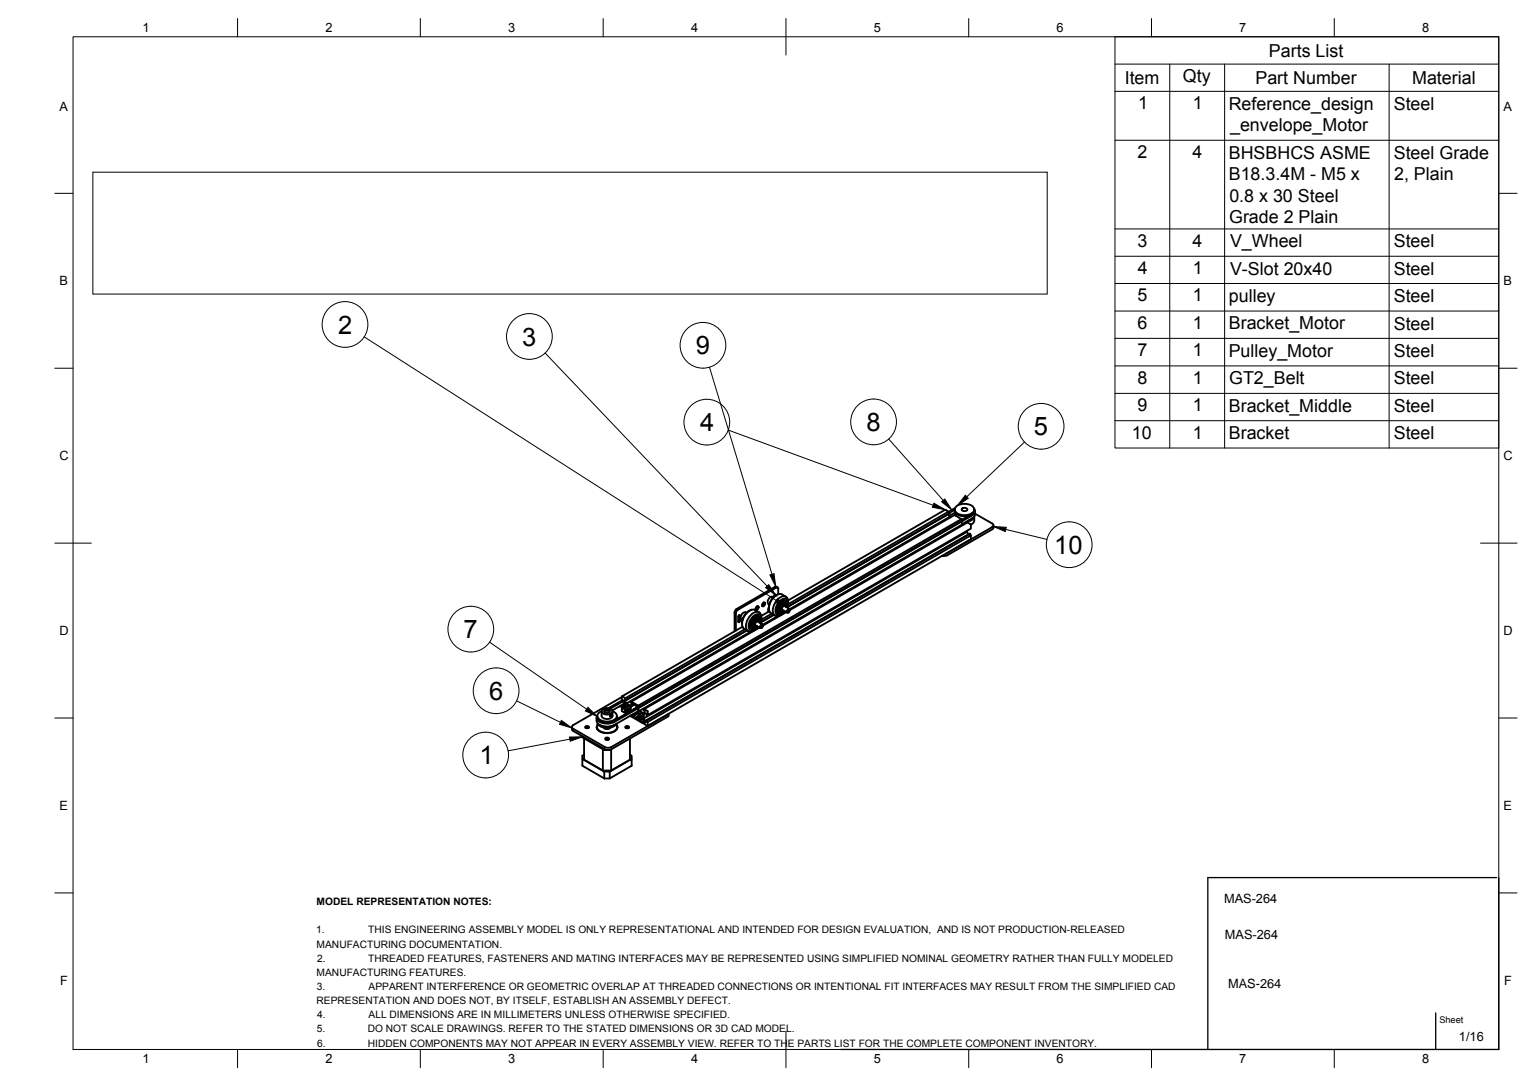
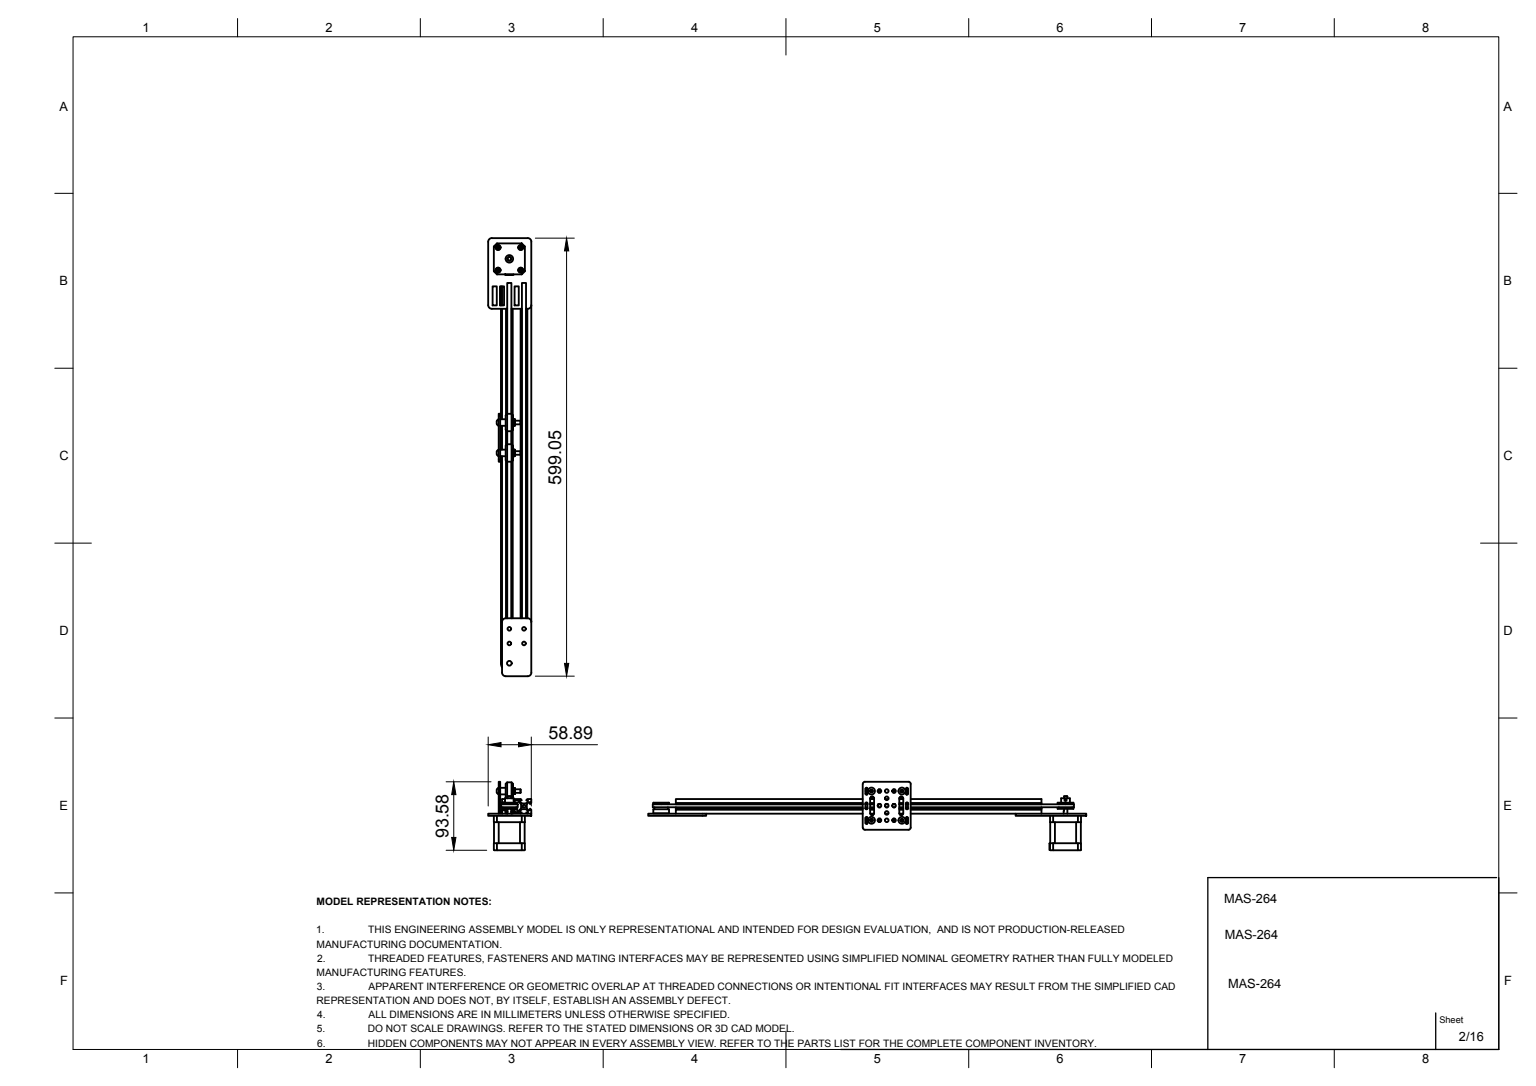
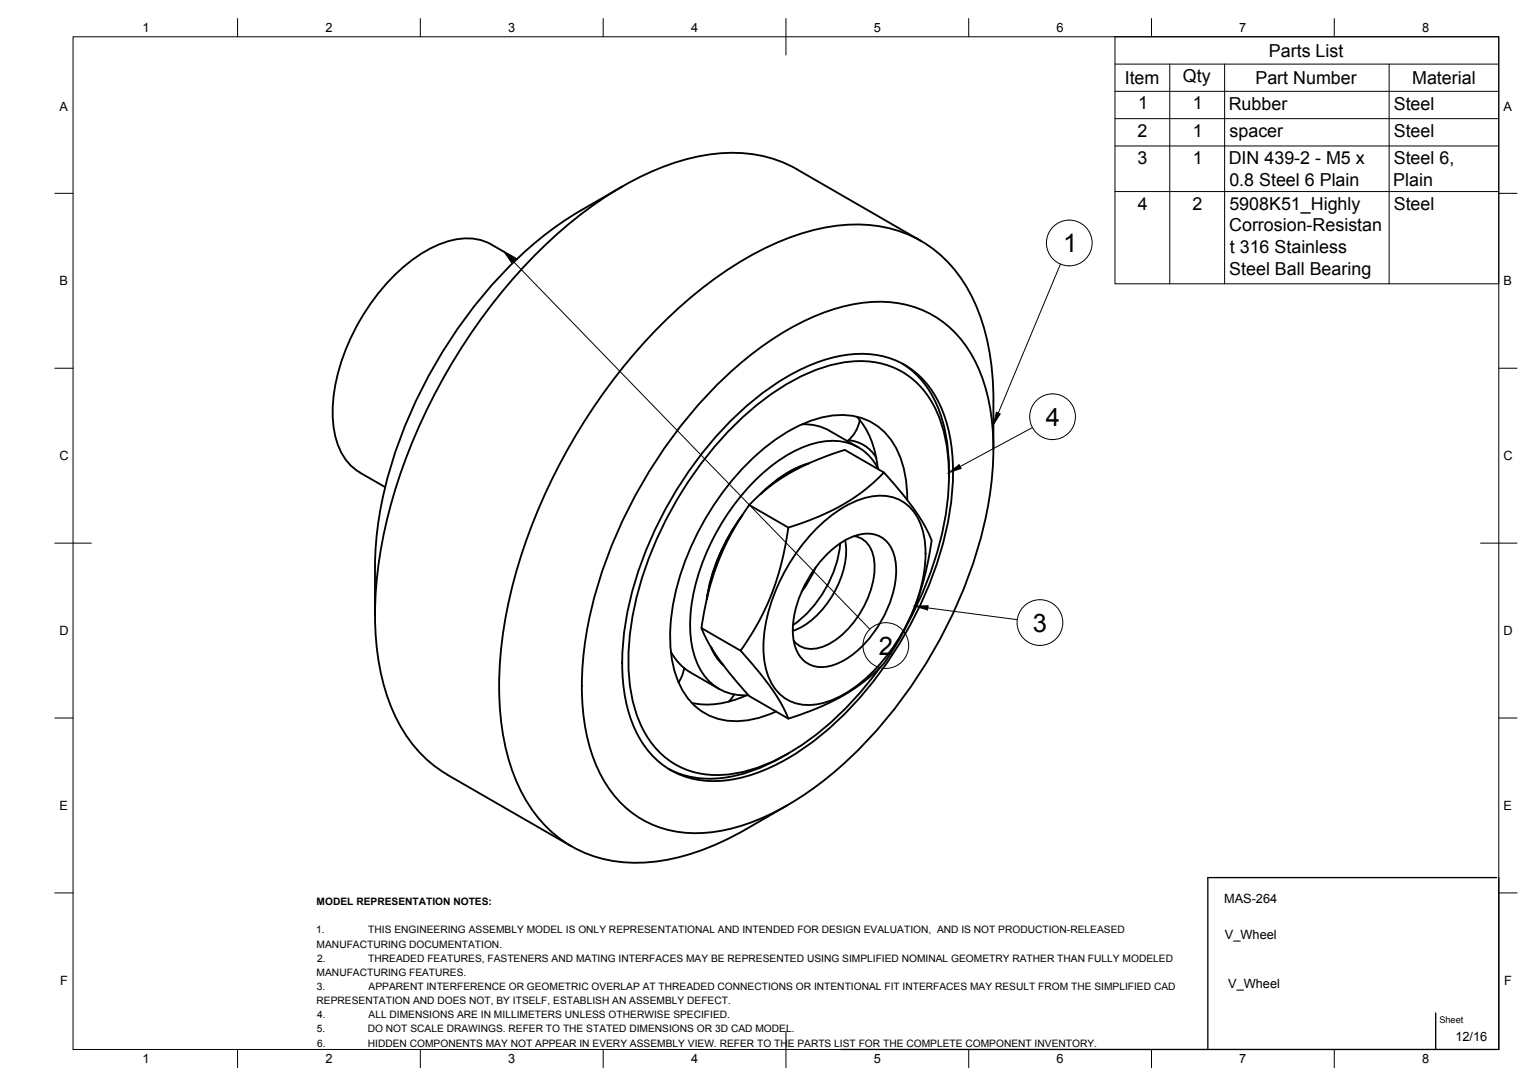
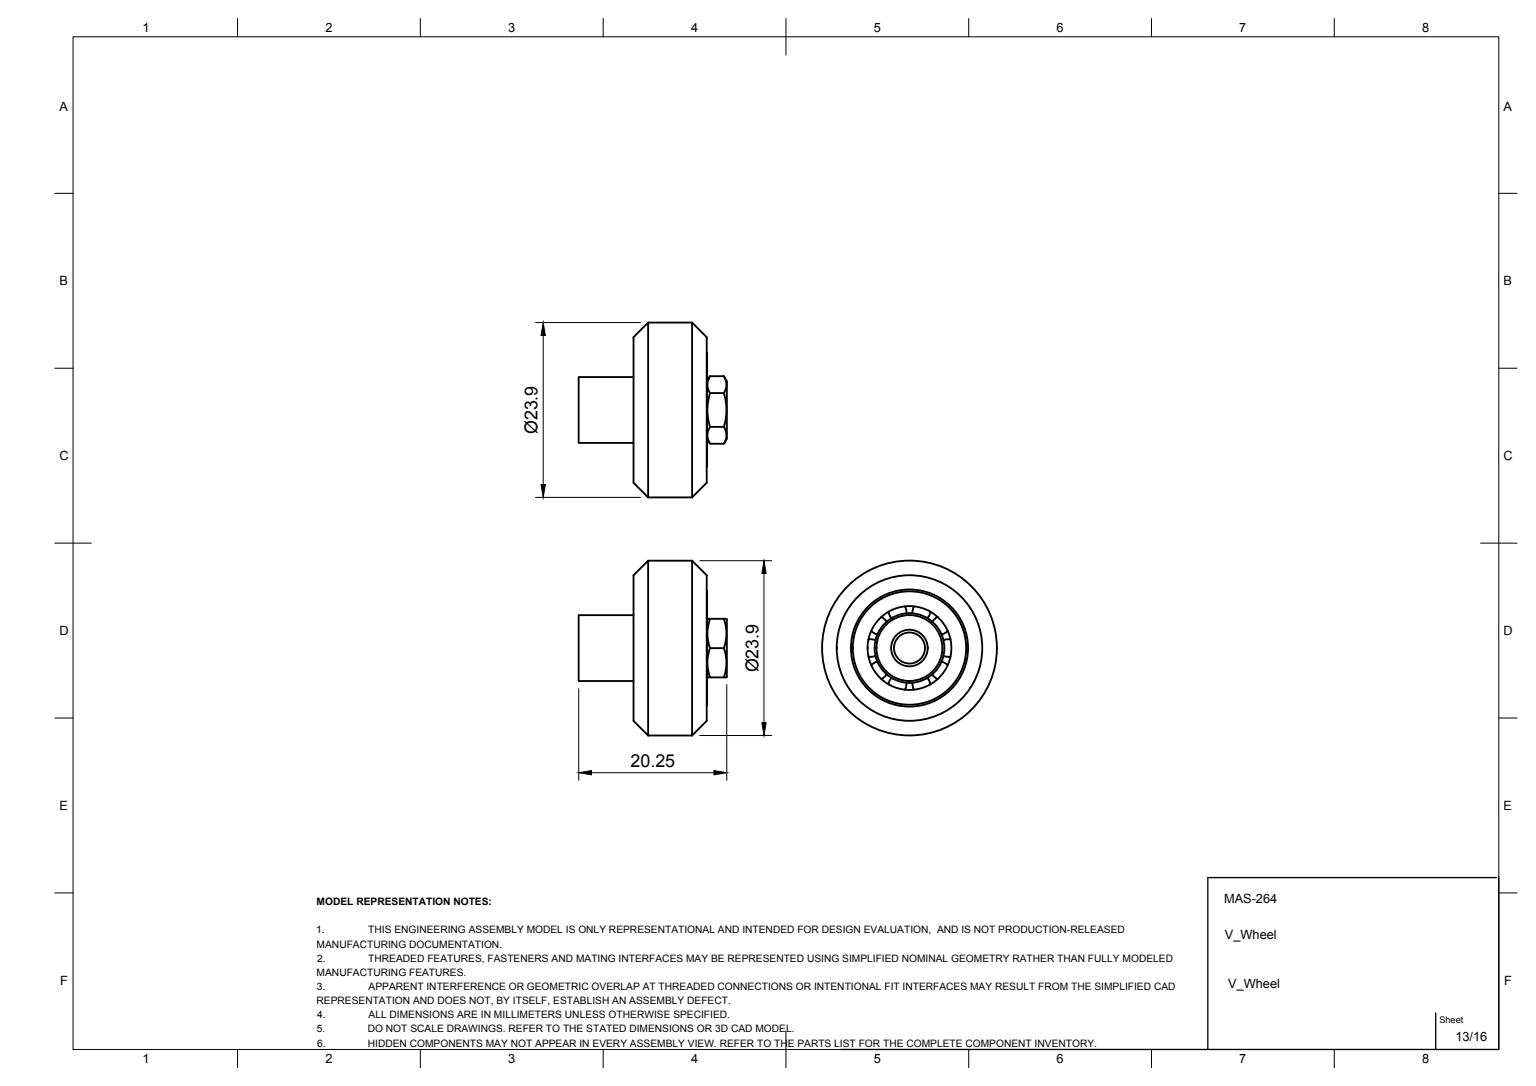
ISO-10303-21;
HEADER;
/* Generated by software containing ST-Developer
 * from STEP Tools, Inc. (www.steptools.com) 
 */

FILE_DESCRIPTION(
/* description */ (''),
/* implementation_level */ '2;1');

FILE_NAME(
/* name */ 'MAS-264',
/* time_stamp */ '2026-10-12T15:37:13-07:00',
/* author */ (''),
/* organization */ (''),
/* preprocessor_version */ 'ST-DEVELOPER v20.2',
/* originating_system */ 'Autodesk Translation Framework v15.15.0.0',
/* authorisation */ '');

FILE_SCHEMA (('AUTOMOTIVE_DESIGN { 1 0 10303 214 3 1 1 }'));
ENDSEC;

DATA;
#10=MECHANICAL_DESIGN_GEOMETRIC_PRESENTATION_REPRESENTATION('',(#326,#327,
#328,#329,#330,#331,#332,#333,#334,#335,#336,#337,#338,#339,#340,#341,#342,
#343,#344,#345,#346,#347,#348,#349,#350,#351,#352,#353,#354,#355,#356,#357),
#36460);
#11=ITEM_DEFINED_TRANSFORMATION($,$,#11888,#12004);
#12=ITEM_DEFINED_TRANSFORMATION($,$,#11901,#12005);
#13=ITEM_DEFINED_TRANSFORMATION($,$,#11910,#12006);
#14=ITEM_DEFINED_TRANSFORMATION($,$,#11930,#12007);
#15=ITEM_DEFINED_TRANSFORMATION($,$,#11930,#12008);
#16=ITEM_DEFINED_TRANSFORMATION($,$,#11439,#12421);
#17=ITEM_DEFINED_TRANSFORMATION($,$,#12393,#12422);
#18=ITEM_DEFINED_TRANSFORMATION($,$,#11887,#12423);
#19=ITEM_DEFINED_TRANSFORMATION($,$,#11887,#12424);
#20=ITEM_DEFINED_TRANSFORMATION($,$,#11887,#12425);
#21=ITEM_DEFINED_TRANSFORMATION($,$,#11887,#12426);
#22=ITEM_DEFINED_TRANSFORMATION($,$,#12009,#12427);
#23=ITEM_DEFINED_TRANSFORMATION($,$,#12118,#12428);
#24=ITEM_DEFINED_TRANSFORMATION($,$,#12135,#12429);
#25=ITEM_DEFINED_TRANSFORMATION($,$,#12189,#12430);
#26=ITEM_DEFINED_TRANSFORMATION($,$,#12212,#12431);
#27=ITEM_DEFINED_TRANSFORMATION($,$,#12231,#12432);
#28=ITEM_DEFINED_TRANSFORMATION($,$,#12359,#12433);
#29=ITEM_DEFINED_TRANSFORMATION($,$,#12393,#12434);
#30=ITEM_DEFINED_TRANSFORMATION($,$,#12393,#12435);
#31=ITEM_DEFINED_TRANSFORMATION($,$,#12393,#12436);
#32=(
REPRESENTATION_RELATIONSHIP($,$,#36519,#36518)
REPRESENTATION_RELATIONSHIP_WITH_TRANSFORMATION(#11)
SHAPE_REPRESENTATION_RELATIONSHIP()
);
#33=(
REPRESENTATION_RELATIONSHIP($,$,#36520,#36518)
REPRESENTATION_RELATIONSHIP_WITH_TRANSFORMATION(#12)
SHAPE_REPRESENTATION_RELATIONSHIP()
);
#34=(
REPRESENTATION_RELATIONSHIP($,$,#36521,#36518)
REPRESENTATION_RELATIONSHIP_WITH_TRANSFORMATION(#13)
SHAPE_REPRESENTATION_RELATIONSHIP()
);
#35=(
REPRESENTATION_RELATIONSHIP($,$,#36522,#36518)
REPRESENTATION_RELATIONSHIP_WITH_TRANSFORMATION(#14)
SHAPE_REPRESENTATION_RELATIONSHIP()
);
#36=(
REPRESENTATION_RELATIONSHIP($,$,#36522,#36518)
REPRESENTATION_RELATIONSHIP_WITH_TRANSFORMATION(#15)
SHAPE_REPRESENTATION_RELATIONSHIP()
);
#37=(
REPRESENTATION_RELATIONSHIP($,$,#36517,#36516)
REPRESENTATION_RELATIONSHIP_WITH_TRANSFORMATION(#16)
SHAPE_REPRESENTATION_RELATIONSHIP()
);
#38=(
REPRESENTATION_RELATIONSHIP($,$,#36530,#36516)
REPRESENTATION_RELATIONSHIP_WITH_TRANSFORMATION(#17)
SHAPE_REPRESENTATION_RELATIONSHIP()
);
#39=(
REPRESENTATION_RELATIONSHIP($,$,#36518,#36516)
REPRESENTATION_RELATIONSHIP_WITH_TRANSFORMATION(#18)
SHAPE_REPRESENTATION_RELATIONSHIP()
);
#40=(
REPRESENTATION_RELATIONSHIP($,$,#36518,#36516)
REPRESENTATION_RELATIONSHIP_WITH_TRANSFORMATION(#19)
SHAPE_REPRESENTATION_RELATIONSHIP()
);
#41=(
REPRESENTATION_RELATIONSHIP($,$,#36518,#36516)
REPRESENTATION_RELATIONSHIP_WITH_TRANSFORMATION(#20)
SHAPE_REPRESENTATION_RELATIONSHIP()
);
#42=(
REPRESENTATION_RELATIONSHIP($,$,#36518,#36516)
REPRESENTATION_RELATIONSHIP_WITH_TRANSFORMATION(#21)
SHAPE_REPRESENTATION_RELATIONSHIP()
);
#43=(
REPRESENTATION_RELATIONSHIP($,$,#36523,#36516)
REPRESENTATION_RELATIONSHIP_WITH_TRANSFORMATION(#22)
SHAPE_REPRESENTATION_RELATIONSHIP()
);
#44=(
REPRESENTATION_RELATIONSHIP($,$,#36524,#36516)
REPRESENTATION_RELATIONSHIP_WITH_TRANSFORMATION(#23)
SHAPE_REPRESENTATION_RELATIONSHIP()
);
#45=(
REPRESENTATION_RELATIONSHIP($,$,#36525,#36516)
REPRESENTATION_RELATIONSHIP_WITH_TRANSFORMATION(#24)
SHAPE_REPRESENTATION_RELATIONSHIP()
);
#46=(
REPRESENTATION_RELATIONSHIP($,$,#36526,#36516)
REPRESENTATION_RELATIONSHIP_WITH_TRANSFORMATION(#25)
SHAPE_REPRESENTATION_RELATIONSHIP()
);
#47=(
REPRESENTATION_RELATIONSHIP($,$,#36527,#36516)
REPRESENTATION_RELATIONSHIP_WITH_TRANSFORMATION(#26)
SHAPE_REPRESENTATION_RELATIONSHIP()
);
#48=(
REPRESENTATION_RELATIONSHIP($,$,#36528,#36516)
REPRESENTATION_RELATIONSHIP_WITH_TRANSFORMATION(#27)
SHAPE_REPRESENTATION_RELATIONSHIP()
);
#49=(
REPRESENTATION_RELATIONSHIP($,$,#36529,#36516)
REPRESENTATION_RELATIONSHIP_WITH_TRANSFORMATION(#28)
SHAPE_REPRESENTATION_RELATIONSHIP()
);
#50=(
REPRESENTATION_RELATIONSHIP($,$,#36530,#36516)
REPRESENTATION_RELATIONSHIP_WITH_TRANSFORMATION(#29)
SHAPE_REPRESENTATION_RELATIONSHIP()
);
#51=(
REPRESENTATION_RELATIONSHIP($,$,#36530,#36516)
REPRESENTATION_RELATIONSHIP_WITH_TRANSFORMATION(#30)
SHAPE_REPRESENTATION_RELATIONSHIP()
);
#52=(
REPRESENTATION_RELATIONSHIP($,$,#36530,#36516)
REPRESENTATION_RELATIONSHIP_WITH_TRANSFORMATION(#31)
SHAPE_REPRESENTATION_RELATIONSHIP()
);
#53=CONTEXT_DEPENDENT_SHAPE_REPRESENTATION(#32,#36487);
#54=CONTEXT_DEPENDENT_SHAPE_REPRESENTATION(#33,#36488);
#55=CONTEXT_DEPENDENT_SHAPE_REPRESENTATION(#34,#36489);
#56=CONTEXT_DEPENDENT_SHAPE_REPRESENTATION(#35,#36490);
#57=CONTEXT_DEPENDENT_SHAPE_REPRESENTATION(#36,#36491);
#58=CONTEXT_DEPENDENT_SHAPE_REPRESENTATION(#37,#36500);
#59=CONTEXT_DEPENDENT_SHAPE_REPRESENTATION(#38,#36501);
#60=CONTEXT_DEPENDENT_SHAPE_REPRESENTATION(#39,#36502);
#61=CONTEXT_DEPENDENT_SHAPE_REPRESENTATION(#40,#36503);
#62=CONTEXT_DEPENDENT_SHAPE_REPRESENTATION(#41,#36504);
#63=CONTEXT_DEPENDENT_SHAPE_REPRESENTATION(#42,#36505);
#64=CONTEXT_DEPENDENT_SHAPE_REPRESENTATION(#43,#36506);
#65=CONTEXT_DEPENDENT_SHAPE_REPRESENTATION(#44,#36507);
#66=CONTEXT_DEPENDENT_SHAPE_REPRESENTATION(#45,#36508);
#67=CONTEXT_DEPENDENT_SHAPE_REPRESENTATION(#46,#36509);
#68=CONTEXT_DEPENDENT_SHAPE_REPRESENTATION(#47,#36510);
#69=CONTEXT_DEPENDENT_SHAPE_REPRESENTATION(#48,#36511);
#70=CONTEXT_DEPENDENT_SHAPE_REPRESENTATION(#49,#36512);
#71=CONTEXT_DEPENDENT_SHAPE_REPRESENTATION(#50,#36513);
#72=CONTEXT_DEPENDENT_SHAPE_REPRESENTATION(#51,#36514);
#73=CONTEXT_DEPENDENT_SHAPE_REPRESENTATION(#52,#36515);
#74=NEXT_ASSEMBLY_USAGE_OCCURRENCE('Rubber:1','Rubber:1','Rubber:1',#36534,
#36535,'Rubber:1');
#75=NEXT_ASSEMBLY_USAGE_OCCURRENCE('Spacer:1','Spacer:1','Spacer:1',#36534,
#36536,'Spacer:1');
#76=NEXT_ASSEMBLY_USAGE_OCCURRENCE(
'Hexagon Thin Nut DIN 439-2 - M5 x 0.8 Steel 6 Plain v1:1',
'Hexagon Thin Nut DIN 439-2 - M5 x 0.8 Steel 6 Plain v1:1',
'Hexagon Thin Nut DIN 439-2 - M5 x 0.8 Steel 6 Plain v1:1',#36534,#36537,
'Hexagon Thin Nut DIN 439-2 - M5 x 0.8 Steel 6 Plain v1:1');
#77=NEXT_ASSEMBLY_USAGE_OCCURRENCE(
'5908K51_Highly Corrosion-Resistant 316 Stainless Steel Ball Bearing:1',
'5908K51_Highly Corrosion-Resistant 316 Stainless Steel Ball Bearing:1',
'5908K51_Highly Corrosion-Resistant 316 Stainless Steel Ball Bearing:1',
#36534,#36538,
'5908K51_Highly Corrosion-Resistant 316 Stainless Steel Ball Bearing:1');
#78=NEXT_ASSEMBLY_USAGE_OCCURRENCE(
'5908K51_Highly Corrosion-Resistant 316 Stainless Steel Ball Bearing:2',
'5908K51_Highly Corrosion-Resistant 316 Stainless Steel Ball Bearing:2',
'5908K51_Highly Corrosion-Resistant 316 Stainless Steel Ball Bearing:2',
#36534,#36538,
'5908K51_Highly Corrosion-Resistant 316 Stainless Steel Ball Bearing:2');
#79=NEXT_ASSEMBLY_USAGE_OCCURRENCE('Reference_design_envelope_Motor:1',
'Reference_design_envelope_Motor:1','Reference_design_envelope_Motor:1',
#36532,#36533,'Reference_design_envelope_Motor:1');
#80=NEXT_ASSEMBLY_USAGE_OCCURRENCE(
'BHSBHCS ASME B18.3.4M - M5 x 0.8 x 30 Steel Grade 2 Plain:1',
'BHSBHCS ASME B18.3.4M - M5 x 0.8 x 30 Steel Grade 2 Plain:1',
'BHSBHCS ASME B18.3.4M - M5 x 0.8 x 30 Steel Grade 2 Plain:1',#36532,#36546,
'BHSBHCS ASME B18.3.4M - M5 x 0.8 x 30 Steel Grade 2 Plain:1');
#81=NEXT_ASSEMBLY_USAGE_OCCURRENCE('V_Wheel:1','V_Wheel:1','V_Wheel:1',
#36532,#36534,'V_Wheel:1');
#82=NEXT_ASSEMBLY_USAGE_OCCURRENCE('V_Wheel:2','V_Wheel:2','V_Wheel:2',
#36532,#36534,'V_Wheel:2');
#83=NEXT_ASSEMBLY_USAGE_OCCURRENCE('V_Wheel:3','V_Wheel:3','V_Wheel:3',
#36532,#36534,'V_Wheel:3');
#84=NEXT_ASSEMBLY_USAGE_OCCURRENCE('V_Wheel:4','V_Wheel:4','V_Wheel:4',
#36532,#36534,'V_Wheel:4');
#85=NEXT_ASSEMBLY_USAGE_OCCURRENCE('V-Slot 20x40:1','V-Slot 20x40:1',
'V-Slot 20x40:1',#36532,#36539,'V-Slot 20x40:1');
#86=NEXT_ASSEMBLY_USAGE_OCCURRENCE('Pulley:1','Pulley:1','Pulley:1',#36532,
#36540,'Pulley:1');
#87=NEXT_ASSEMBLY_USAGE_OCCURRENCE('Bracket_Motor:1','Bracket_Motor:1',
'Bracket_Motor:1',#36532,#36541,'Bracket_Motor:1');
#88=NEXT_ASSEMBLY_USAGE_OCCURRENCE('Pulley_Motor:1','Pulley_Motor:1',
'Pulley_Motor:1',#36532,#36542,'Pulley_Motor:1');
#89=NEXT_ASSEMBLY_USAGE_OCCURRENCE('GT2_Belt:1','GT2_Belt:1',
'GT2_Belt:1',#36532,#36543,'GT2_Belt:1');
#90=NEXT_ASSEMBLY_USAGE_OCCURRENCE('Bracket_Middle:1',
'Bracket_Middle:1','Bracket_Middle:1',#36532,#36544,'Bracket_Middle:1');
#91=NEXT_ASSEMBLY_USAGE_OCCURRENCE('Bracket:1','Bracket:1','Bracket:1',
#36532,#36545,'Bracket:1');
#92=NEXT_ASSEMBLY_USAGE_OCCURRENCE(
'BHSBHCS ASME B18.3.4M - M5 x 0.8 x 30 Steel Grade 2 Plain:2',
'BHSBHCS ASME B18.3.4M - M5 x 0.8 x 30 Steel Grade 2 Plain:2',
'BHSBHCS ASME B18.3.4M - M5 x 0.8 x 30 Steel Grade 2 Plain:2',#36532,#36546,
'BHSBHCS ASME B18.3.4M - M5 x 0.8 x 30 Steel Grade 2 Plain:2');
#93=NEXT_ASSEMBLY_USAGE_OCCURRENCE(
'BHSBHCS ASME B18.3.4M - M5 x 0.8 x 30 Steel Grade 2 Plain:3',
'BHSBHCS ASME B18.3.4M - M5 x 0.8 x 30 Steel Grade 2 Plain:3',
'BHSBHCS ASME B18.3.4M - M5 x 0.8 x 30 Steel Grade 2 Plain:3',#36532,#36546,
'BHSBHCS ASME B18.3.4M - M5 x 0.8 x 30 Steel Grade 2 Plain:3');
#94=NEXT_ASSEMBLY_USAGE_OCCURRENCE(
'BHSBHCS ASME B18.3.4M - M5 x 0.8 x 30 Steel Grade 2 Plain:4',
'BHSBHCS ASME B18.3.4M - M5 x 0.8 x 30 Steel Grade 2 Plain:4',
'BHSBHCS ASME B18.3.4M - M5 x 0.8 x 30 Steel Grade 2 Plain:4',#36532,#36546,
'BHSBHCS ASME B18.3.4M - M5 x 0.8 x 30 Steel Grade 2 Plain:4');
#95=SPHERICAL_SURFACE('',#11984,1.21175743903915);
#96=SPHERICAL_SURFACE('',#11986,1.21175743903915);
#97=SPHERICAL_SURFACE('',#11988,1.21175743903915);
#98=SPHERICAL_SURFACE('',#11990,1.21175743903915);
#99=SPHERICAL_SURFACE('',#11992,1.21175743903915);
#100=SPHERICAL_SURFACE('',#11994,1.21175743903915);
#101=SPHERICAL_SURFACE('',#11996,1.21175743903915);
#102=SPHERICAL_SURFACE('',#11998,1.21175743903915);
#103=SPHERICAL_SURFACE('',#12000,1.21175743903915);
#104=SPHERICAL_SURFACE('',#12002,1.21175743903915);
#105=SPHERICAL_SURFACE('',#12419,5.16792277674902);
#106=SHAPE_REPRESENTATION_RELATIONSHIP('SRR','None',#36517,#119);
#107=SHAPE_REPRESENTATION_RELATIONSHIP('SRR','None',#36519,#120);
#108=SHAPE_REPRESENTATION_RELATIONSHIP('SRR','None',#36520,#121);
#109=SHAPE_REPRESENTATION_RELATIONSHIP('SRR','None',#36521,#122);
#110=SHAPE_REPRESENTATION_RELATIONSHIP('SRR','None',#36522,#123);
#111=SHAPE_REPRESENTATION_RELATIONSHIP('SRR','None',#36523,#124);
#112=SHAPE_REPRESENTATION_RELATIONSHIP('SRR','None',#36524,#125);
#113=SHAPE_REPRESENTATION_RELATIONSHIP('SRR','None',#36525,#126);
#114=SHAPE_REPRESENTATION_RELATIONSHIP('SRR','None',#36526,#127);
#115=SHAPE_REPRESENTATION_RELATIONSHIP('SRR','None',#36527,#128);
#116=SHAPE_REPRESENTATION_RELATIONSHIP('SRR','None',#36528,#129);
#117=SHAPE_REPRESENTATION_RELATIONSHIP('SRR','None',#36529,#130);
#118=SHAPE_REPRESENTATION_RELATIONSHIP('SRR','None',#36530,#131);
#119=ADVANCED_BREP_SHAPE_REPRESENTATION('',(#358,#359,#360,#361,#362,#363,
#364,#365),#36446);
#120=ADVANCED_BREP_SHAPE_REPRESENTATION('',(#366),#36448);
#121=ADVANCED_BREP_SHAPE_REPRESENTATION('',(#367),#36449);
#122=ADVANCED_BREP_SHAPE_REPRESENTATION('',(#368),#36450);
#123=ADVANCED_BREP_SHAPE_REPRESENTATION('',(#369,#370,#371,#372,#373,#374,
#375,#376,#377,#378,#379,#380,#381),#36451);
#124=ADVANCED_BREP_SHAPE_REPRESENTATION('',(#382),#36452);
#125=ADVANCED_BREP_SHAPE_REPRESENTATION('',(#383),#36453);
#126=ADVANCED_BREP_SHAPE_REPRESENTATION('',(#384),#36454);
#127=ADVANCED_BREP_SHAPE_REPRESENTATION('',(#385),#36455);
#128=ADVANCED_BREP_SHAPE_REPRESENTATION('',(#386),#36456);
#129=ADVANCED_BREP_SHAPE_REPRESENTATION('',(#387),#36457);
#130=ADVANCED_BREP_SHAPE_REPRESENTATION('',(#388),#36458);
#131=ADVANCED_BREP_SHAPE_REPRESENTATION('',(#389),#36459);
#132=FACE_BOUND('',#1845,.T.);
#133=FACE_BOUND('',#1846,.T.);
#134=FACE_BOUND('',#1847,.T.);
#135=FACE_BOUND('',#1848,.T.);
#136=FACE_BOUND('',#1849,.T.);
#137=FACE_BOUND('',#1863,.T.);
#138=FACE_BOUND('',#1865,.T.);
#139=FACE_BOUND('',#1883,.T.);
#140=FACE_BOUND('',#1884,.T.);
#141=FACE_BOUND('',#1885,.T.);
#142=FACE_BOUND('',#1886,.T.);
#143=FACE_BOUND('',#1887,.T.);
#144=FACE_BOUND('',#1893,.T.);
#145=FACE_BOUND('',#1917,.T.);
#146=FACE_BOUND('',#1920,.T.);
#147=FACE_BOUND('',#1921,.T.);
#148=FACE_BOUND('',#1922,.T.);
#149=FACE_BOUND('',#1923,.T.);
#150=FACE_BOUND('',#1924,.T.);
#151=FACE_BOUND('',#1945,.T.);
#152=FACE_BOUND('',#1947,.T.);
#153=FACE_BOUND('',#1954,.T.);
#154=FACE_BOUND('',#1956,.T.);
#155=FACE_BOUND('',#1957,.T.);
#156=FACE_BOUND('',#1958,.T.);
#157=FACE_BOUND('',#1959,.T.);
#158=FACE_BOUND('',#1960,.T.);
#159=FACE_BOUND('',#1976,.T.);
#160=FACE_BOUND('',#1979,.T.);
#161=FACE_BOUND('',#1984,.T.);
#162=FACE_BOUND('',#1986,.T.);
#163=FACE_BOUND('',#1997,.T.);
#164=FACE_BOUND('',#2000,.T.);
#165=FACE_BOUND('',#2009,.T.);
#166=FACE_BOUND('',#2011,.T.);
#167=FACE_BOUND('',#2017,.T.);
#168=FACE_BOUND('',#2019,.T.);
#169=FACE_BOUND('',#2028,.T.);
#170=FACE_BOUND('',#2030,.T.);
#171=FACE_BOUND('',#2032,.T.);
#172=FACE_BOUND('',#2091,.T.);
#173=FACE_BOUND('',#2092,.T.);
#174=FACE_BOUND('',#2093,.T.);
#175=FACE_BOUND('',#2142,.T.);
#176=FACE_BOUND('',#2143,.T.);
#177=FACE_BOUND('',#2144,.T.);
#178=FACE_BOUND('',#2146,.T.);
#179=FACE_BOUND('',#2149,.T.);
#180=FACE_BOUND('',#2151,.T.);
#181=FACE_BOUND('',#2155,.T.);
#182=FACE_BOUND('',#2191,.T.);
#183=FACE_BOUND('',#2192,.T.);
#184=FACE_BOUND('',#2193,.T.);
#185=FACE_BOUND('',#2194,.T.);
#186=FACE_BOUND('',#2195,.T.);
#187=FACE_BOUND('',#2196,.T.);
#188=FACE_BOUND('',#2197,.T.);
#189=FACE_BOUND('',#2198,.T.);
#190=FACE_BOUND('',#2200,.T.);
#191=FACE_BOUND('',#2201,.T.);
#192=FACE_BOUND('',#2202,.T.);
#193=FACE_BOUND('',#2203,.T.);
#194=FACE_BOUND('',#2204,.T.);
#195=FACE_BOUND('',#2205,.T.);
#196=FACE_BOUND('',#2206,.T.);
#197=FACE_BOUND('',#2207,.T.);
#198=FACE_BOUND('',#2211,.T.);
#199=FACE_BOUND('',#2213,.T.);
#200=FACE_BOUND('',#2215,.T.);
#201=FACE_BOUND('',#2218,.T.);
#202=FACE_BOUND('',#2221,.T.);
#203=FACE_BOUND('',#2224,.T.);
#204=FACE_BOUND('',#2226,.T.);
#205=FACE_BOUND('',#2228,.T.);
#206=FACE_BOUND('',#2238,.T.);
#207=FACE_BOUND('',#2295,.T.);
#208=FACE_BOUND('',#2296,.T.);
#209=FACE_BOUND('',#2297,.T.);
#210=FACE_BOUND('',#2298,.T.);
#211=FACE_BOUND('',#2299,.T.);
#212=FACE_BOUND('',#2300,.T.);
#213=FACE_BOUND('',#2301,.T.);
#214=FACE_BOUND('',#2302,.T.);
#215=FACE_BOUND('',#2303,.T.);
#216=FACE_BOUND('',#2304,.T.);
#217=FACE_BOUND('',#2305,.T.);
#218=FACE_BOUND('',#2306,.T.);
#219=FACE_BOUND('',#2307,.T.);
#220=FACE_BOUND('',#2308,.T.);
#221=FACE_BOUND('',#2309,.T.);
#222=FACE_BOUND('',#2310,.T.);
#223=FACE_BOUND('',#2311,.T.);
#224=FACE_BOUND('',#2312,.T.);
#225=FACE_BOUND('',#2313,.T.);
#226=FACE_BOUND('',#2314,.T.);
#227=FACE_BOUND('',#2315,.T.);
#228=FACE_BOUND('',#2316,.T.);
#229=FACE_BOUND('',#2317,.T.);
#230=FACE_BOUND('',#2319,.T.);
#231=FACE_BOUND('',#2320,.T.);
#232=FACE_BOUND('',#2321,.T.);
#233=FACE_BOUND('',#2322,.T.);
#234=FACE_BOUND('',#2323,.T.);
#235=FACE_BOUND('',#2324,.T.);
#236=FACE_BOUND('',#2325,.T.);
#237=FACE_BOUND('',#2326,.T.);
#238=FACE_BOUND('',#2327,.T.);
#239=FACE_BOUND('',#2328,.T.);
#240=FACE_BOUND('',#2329,.T.);
#241=FACE_BOUND('',#2330,.T.);
#242=FACE_BOUND('',#2331,.T.);
#243=FACE_BOUND('',#2332,.T.);
#244=FACE_BOUND('',#2333,.T.);
#245=FACE_BOUND('',#2334,.T.);
#246=FACE_BOUND('',#2335,.T.);
#247=FACE_BOUND('',#2336,.T.);
#248=FACE_BOUND('',#2337,.T.);
#249=FACE_BOUND('',#2338,.T.);
#250=FACE_BOUND('',#2339,.T.);
#251=FACE_BOUND('',#2340,.T.);
#252=FACE_BOUND('',#2341,.T.);
#253=FACE_BOUND('',#2356,.T.);
#254=FACE_BOUND('',#2357,.T.);
#255=FACE_BOUND('',#2358,.T.);
#256=FACE_BOUND('',#2359,.T.);
#257=FACE_BOUND('',#2360,.T.);
#258=FACE_BOUND('',#2362,.T.);
#259=FACE_BOUND('',#2363,.T.);
#260=FACE_BOUND('',#2364,.T.);
#261=FACE_BOUND('',#2365,.T.);
#262=FACE_BOUND('',#2366,.T.);
#263=FACE_BOUND('',#2370,.T.);
#264=FACE_BOUND('',#2386,.T.);
#265=(
BOUNDED_CURVE()
B_SPLINE_CURVE(2,(#24742,#24743,#24744,#24745,#24746,#24747,#24748,#24749,
#24750,#24751,#24752,#24753,#24754,#24755,#24756,#24757,#24758,#24759,#24760,
#24761,#24762,#24763,#24764,#24765,#24766,#24767,#24768,#24769,#24770,#24771,
#24772,#24773,#24774,#24775,#24776,#24777,#24778,#24779,#24780,#24781,#24782,
#24783,#24784,#24785,#24786,#24787,#24788,#24789,#24790,#24791,#24792,#24793,
#24794,#24795,#24796,#24797,#24798,#24799,#24800,#24801,#24802,#24803,#24804,
#24805,#24806,#24807,#24808,#24809,#24810,#24811,#24812,#24813,#24814,#24815,
#24816,#24817,#24818,#24819,#24820,#24821,#24822,#24823,#24824,#24825,#24826,
#24827,#24828,#24829,#24830,#24831,#24832,#24833,#24834,#24835,#24836,#24837,
#24838,#24839,#24840,#24841,#24842,#24843,#24844,#24845,#24846,#24847,#24848,
#24849,#24850,#24851,#24852,#24853,#24854,#24855,#24856,#24857,#24858,#24859,
#24860,#24861,#24862,#24863,#24864,#24865,#24866,#24867,#24868,#24869,#24870,
#24871,#24872,#24873,#24874,#24875,#24876,#24877,#24878,#24879,#24880,#24881,
#24882,#24883,#24884,#24885,#24886,#24887,#24888,#24889,#24890,#24891,#24892,
#24893,#24894,#24895,#24896,#24897,#24898,#24899,#24900,#24901,#24902,#24903,
#24904,#24905,#24906,#24907,#24908,#24909,#24910,#24911,#24912,#24913,#24914,
#24915,#24916,#24917,#24918,#24919,#24920,#24921,#24922,#24923,#24924,#24925,
#24926,#24927,#24928,#24929,#24930,#24931,#24932,#24933,#24934,#24935,#24936,
#24937,#24938,#24939,#24940,#24941,#24942,#24943,#24944,#24945,#24946,#24947,
#24948,#24949,#24950,#24951,#24952,#24953,#24954,#24955,#24956,#24957,#24958,
#24959,#24960,#24961,#24962,#24963,#24964,#24965,#24966,#24967,#24968,#24969,
#24970,#24971,#24972,#24973,#24974,#24975,#24976,#24977,#24978,#24979,#24980,
#24981,#24982,#24983,#24984,#24985,#24986,#24987,#24988,#24989,#24990,#24991,
#24992,#24993,#24994,#24995,#24996,#24997,#24998,#24999,#25000,#25001,#25002,
#25003,#25004,#25005,#25006,#25007,#25008,#25009,#25010,#25011,#25012,#25013,
#25014,#25015,#25016,#25017,#25018,#25019,#25020,#25021,#25022,#25023,#25024,
#25025,#25026,#25027,#25028,#25029,#25030,#25031,#25032,#25033,#25034,#25035,
#25036,#25037,#25038,#25039,#25040,#25041,#25042),.UNSPECIFIED.,.F.,.F.)
B_SPLINE_CURVE_WITH_KNOTS((3,2,2,2,2,2,2,2,2,2,2,2,2,2,2,2,2,2,2,2,2,2,
2,2,2,2,2,2,2,2,2,2,2,2,2,2,2,2,2,2,2,2,2,2,2,2,2,2,2,2,2,2,2,2,2,2,2,2,
2,2,2,2,2,2,2,2,2,2,2,2,2,2,2,2,2,2,2,2,2,2,2,2,2,2,2,2,2,2,2,2,2,2,2,2,
2,2,2,2,2,2,2,2,2,2,2,2,2,2,2,2,2,2,2,2,2,2,2,2,2,2,2,2,2,2,2,2,2,2,2,2,
2,2,2,2,2,2,2,2,2,2,2,2,2,2,2,2,2,2,2,2,3),(0.0578262804341777,0.063130434027066,
0.0694434774297724,0.0757565208324788,0.0820695642351851,0.0883826076378915,
0.0946956510405978,0.101008694443304,0.107321737846011,0.113634781248717,
0.119947824651423,0.12626086805413,0.132573911456836,0.138886954859542,
0.145199998262249,0.151513041664955,0.157826085067661,0.164139128470368,
0.170452171873074,0.17676521527578,0.183078258678487,0.189391302081193,
0.195704345483899,0.202017388886606,0.208330432289312,0.214643475692019,
0.220956519094725,0.227269562497431,0.233582605900138,0.239895649302844,
0.24620869270555,0.252521736108257,0.258834779510963,0.265147822913669,
0.271460866316376,0.277773909719082,0.284086953121788,0.290399996524495,
0.296713039927201,0.303026083329907,0.309339126732614,0.31565217013532,
0.321965213538027,0.328278256940733,0.334591300343439,0.340904343746146,
0.347217387148852,0.353530430551558,0.359843473954265,0.366156517356971,
0.372469560759677,0.378782604162384,0.38509564756509,0.391408690967797,
0.397721734370503,0.404034777773209,0.410347821175916,0.416660864578622,
0.422973907981328,0.429286951384035,0.435599994786741,0.441913038189447,
0.448226081592154,0.45453912499486,0.460852168397566,0.467165211800273,
0.473478255202979,0.479791298605685,0.486104342008392,0.492417385411098,
0.498730428813805,0.505043472216511,0.511356515619217,0.517669559021924,
0.52398260242463,0.530295645827336,0.536608689230043,0.542921732632749,
0.549234776035455,0.555547819438162,0.561860862840868,0.568173906243575,
0.574486949646281,0.580799993048987,0.587113036451693,0.5934260798544,0.599739123257106,
0.606052166659813,0.612365210062519,0.618678253465225,0.624991296867932,
0.631304340270638,0.637617383673344,0.643930427076051,0.650243470478757,
0.656556513881463,0.66286955728417,0.669182600686876,0.675495644089582,
0.681808687492289,0.688121730894995,0.694434774297702,0.700747817700408,
0.707060861103114,0.71337390450582,0.719686947908527,0.725999991311233,
0.732313034713939,0.738626078116646,0.744939121519352,0.751252164922059,
0.757565208324765,0.763878251727471,0.770191295130178,0.776504338532884,
0.78281738193559,0.789130425338297,0.795443468741003,0.80175651214371,0.808069555546416,
0.814382598949122,0.820695642351829,0.827008685754535,0.833321729157241,
0.839634772559948,0.845947815962654,0.85226085936536,0.858573902768067,
0.864886946170773,0.871199989573479,0.877513032976186,0.883826076378892,
0.890139119781598,0.896452163184305,0.902765206587011,0.909078249989718,
0.915391293392424,0.92170433679513,0.928017380197837,0.934330423600543,
0.940643467003249,0.946956510405956,0.953269553808662,0.959582597211368,
0.965895640614075,0.972208684016781,0.978521727419488,0.984834770822194,
0.9911478142249,0.997460857627607,1.),.UNSPECIFIED.)
CURVE()
GEOMETRIC_REPRESENTATION_ITEM()
RATIONAL_B_SPLINE_CURVE((0.964022189566827,0.887435933741894,1.,0.866025403784439,
1.,0.866025403784439,1.,0.866025403784439,1.,0.866025403784439,1.,0.866025403784439,
1.,0.866025403784439,1.,0.866025403784439,1.,0.866025403784439,1.,0.866025403784439,
1.,0.866025403784439,1.,0.866025403784439,1.,0.866025403784439,1.,0.866025403784439,
1.,0.866025403784439,1.,0.866025403784439,1.,0.866025403784439,1.,0.866025403784439,
1.,0.866025403784439,1.,0.866025403784439,1.,0.866025403784439,1.,0.866025403784439,
1.,0.866025403784439,1.,0.866025403784439,1.,0.866025403784439,1.,0.866025403784439,
1.,0.866025403784439,1.,0.866025403784439,1.,0.866025403784439,1.,0.866025403784439,
1.,0.866025403784439,1.,0.866025403784439,1.,0.866025403784439,1.,0.866025403784439,
1.,0.866025403784439,1.,0.866025403784439,1.,0.866025403784439,1.,0.866025403784439,
1.,0.866025403784439,1.,0.866025403784439,1.,0.866025403784439,1.,0.866025403784439,
1.,0.866025403784439,1.,0.866025403784439,1.,0.866025403784439,1.,0.866025403784439,
1.,0.866025403784439,1.,0.866025403784439,1.,0.866025403784439,1.,0.866025403784439,
1.,0.866025403784439,1.,0.866025403784439,1.,0.866025403784439,1.,0.866025403784439,
1.,0.866025403784439,1.,0.866025403784439,1.,0.866025403784439,1.,0.866025403784439,
1.,0.866025403784439,1.,0.866025403784439,1.,0.866025403784439,1.,0.866025403784439,
1.,0.866025403784439,1.,0.866025403784439,1.,0.866025403784439,1.,0.866025403784439,
1.,0.866025403784439,1.,0.866025403784439,1.,0.866025403784439,1.,0.866025403784439,
1.,0.866025403784439,1.,0.866025403784439,1.,0.866025403784439,1.,0.866025403784439,
1.,0.866025403784439,1.,0.866025403784439,1.,0.866025403784439,1.,0.866025403784439,
1.,0.866025403784439,1.,0.866025403784439,1.,0.866025403784439,1.,0.866025403784439,
1.,0.866025403784439,1.,0.866025403784439,1.,0.866025403784439,1.,0.866025403784439,
1.,0.866025403784439,1.,0.866025403784439,1.,0.866025403784439,1.,0.866025403784439,
1.,0.866025403784439,1.,0.866025403784439,1.,0.866025403784439,1.,0.866025403784439,
1.,0.866025403784439,1.,0.866025403784439,1.,0.866025403784439,1.,0.866025403784439,
1.,0.866025403784439,1.,0.866025403784439,1.,0.866025403784439,1.,0.866025403784439,
1.,0.866025403784439,1.,0.866025403784439,1.,0.866025403784439,1.,0.866025403784439,
1.,0.866025403784439,1.,0.866025403784439,1.,0.866025403784439,1.,0.866025403784439,
1.,0.866025403784439,1.,0.866025403784439,1.,0.866025403784439,1.,0.866025403784439,
1.,0.866025403784439,1.,0.866025403784439,1.,0.866025403784439,1.,0.866025403784439,
1.,0.866025403784439,1.,0.866025403784439,1.,0.866025403784439,1.,0.866025403784439,
1.,0.866025403784439,1.,0.866025403784439,1.,0.866025403784439,1.,0.866025403784439,
1.,0.866025403784439,1.,0.866025403784439,1.,0.866025403784439,1.,0.866025403784439,
1.,0.866025403784439,1.,0.866025403784439,1.,0.866025403784439,1.,0.866025403784439,
1.,0.866025403784439,1.,0.866025403784439,1.,0.866025403784439,1.,0.866025403784439,
1.,0.866025403784439,1.,0.866025403784439,1.,0.866025403784439,1.,0.866025403784439,
1.,0.866025403784439,1.,0.866025403784439,1.,0.866025403784439,1.,0.866025403784439,
1.,0.866025403784439,1.,0.866025403784439,1.,0.866025403784439,1.,0.946114646712328,
0.93557529156098))
REPRESENTATION_ITEM('')
);
#266=(
BOUNDED_CURVE()
B_SPLINE_CURVE(2,(#25685,#25686,#25687,#25688,#25689,#25690,#25691,#25692,
#25693,#25694,#25695,#25696,#25697,#25698,#25699,#25700,#25701,#25702,#25703,
#25704,#25705,#25706,#25707,#25708,#25709,#25710,#25711,#25712,#25713,#25714,
#25715,#25716,#25717,#25718,#25719,#25720,#25721,#25722,#25723,#25724,#25725,
#25726,#25727,#25728,#25729,#25730,#25731,#25732,#25733,#25734,#25735,#25736,
#25737,#25738,#25739,#25740,#25741,#25742,#25743,#25744,#25745,#25746,#25747,
#25748,#25749,#25750,#25751,#25752,#25753,#25754,#25755,#25756,#25757,#25758,
#25759,#25760,#25761,#25762,#25763,#25764,#25765,#25766,#25767,#25768,#25769,
#25770,#25771,#25772,#25773,#25774,#25775,#25776,#25777,#25778,#25779,#25780,
#25781,#25782,#25783,#25784,#25785,#25786,#25787,#25788,#25789,#25790,#25791,
#25792,#25793,#25794,#25795,#25796,#25797,#25798,#25799,#25800,#25801,#25802,
#25803,#25804,#25805,#25806,#25807,#25808,#25809,#25810,#25811,#25812,#25813,
#25814,#25815,#25816,#25817,#25818,#25819,#25820,#25821,#25822,#25823,#25824,
#25825,#25826,#25827,#25828,#25829,#25830,#25831,#25832,#25833,#25834,#25835,
#25836,#25837,#25838,#25839,#25840,#25841,#25842,#25843,#25844,#25845,#25846,
#25847,#25848,#25849,#25850,#25851,#25852,#25853,#25854,#25855,#25856,#25857,
#25858,#25859,#25860,#25861,#25862,#25863,#25864,#25865,#25866,#25867,#25868,
#25869,#25870,#25871,#25872,#25873,#25874,#25875,#25876,#25877,#25878,#25879,
#25880,#25881,#25882,#25883,#25884,#25885,#25886,#25887,#25888,#25889,#25890,
#25891,#25892,#25893,#25894,#25895,#25896,#25897,#25898,#25899,#25900,#25901,
#25902,#25903,#25904,#25905,#25906,#25907,#25908,#25909,#25910,#25911,#25912,
#25913,#25914,#25915,#25916,#25917,#25918,#25919,#25920,#25921,#25922,#25923,
#25924,#25925,#25926,#25927,#25928,#25929,#25930,#25931,#25932,#25933,#25934,
#25935,#25936,#25937,#25938,#25939,#25940,#25941,#25942,#25943,#25944,#25945,
#25946,#25947,#25948,#25949,#25950,#25951,#25952,#25953,#25954,#25955,#25956,
#25957,#25958,#25959,#25960,#25961,#25962,#25963,#25964,#25965,#25966,#25967,
#25968,#25969,#25970,#25971,#25972,#25973,#25974,#25975,#25976,#25977,#25978,
#25979,#25980,#25981,#25982,#25983,#25984,#25985),.UNSPECIFIED.,.F.,.F.)
B_SPLINE_CURVE_WITH_KNOTS((3,2,2,2,2,2,2,2,2,2,2,2,2,2,2,2,2,2,2,2,2,2,
2,2,2,2,2,2,2,2,2,2,2,2,2,2,2,2,2,2,2,2,2,2,2,2,2,2,2,2,2,2,2,2,2,2,2,2,
2,2,2,2,2,2,2,2,2,2,2,2,2,2,2,2,2,2,2,2,2,2,2,2,2,2,2,2,2,2,2,2,2,2,2,2,
2,2,2,2,2,2,2,2,2,2,2,2,2,2,2,2,2,2,2,2,2,2,2,2,2,2,2,2,2,2,2,2,2,2,2,2,
2,2,2,2,2,2,2,2,2,2,2,2,2,2,2,2,2,2,2,2,3),(0.0624132680173737,0.063130431687086,
0.0694434748554471,0.0757565180238082,0.0820695611921693,0.0883826043605304,
0.0946956475288915,0.101008690697253,0.107321733865614,0.113634777033975,
0.119947820202336,0.126260863370697,0.132573906539058,0.138886949707419,
0.14519999287578,0.151513036044142,0.157826079212503,0.164139122380864,
0.170452165549225,0.176765208717586,0.183078251885947,0.189391295054308,
0.195704338222669,0.20201738139103,0.208330424559392,0.214643467727753,
0.220956510896114,0.227269554064475,0.233582597232836,0.239895640401197,
0.246208683569558,0.252521726737919,0.258834769906281,0.265147813074642,
0.271460856243003,0.277773899411364,0.284086942579725,0.290399985748086,
0.296713028916447,0.303026072084808,0.309339115253169,0.31565215842153,
0.321965201589892,0.328278244758253,0.334591287926614,0.340904331094975,
0.347217374263336,0.353530417431697,0.359843460600058,0.366156503768419,
0.37246954693678,0.378782590105142,0.385095633273503,0.391408676441864,
0.397721719610225,0.404034762778586,0.410347805946947,0.416660849115308,
0.422973892283669,0.42928693545203,0.435599978620392,0.441913021788753,
0.448226064957114,0.454539108125475,0.460852151293836,0.467165194462197,
0.473478237630558,0.479791280798919,0.48610432396728,0.492417367135642,
0.498730410304003,0.505043453472364,0.511356496640725,0.517669539809086,
0.523982582977447,0.530295626145808,0.536608669314169,0.542921712482531,
0.549234755650892,0.555547798819253,0.561860841987614,0.568173885155975,
0.574486928324336,0.580799971492697,0.587113014661058,0.593426057829419,
0.599739100997781,0.606052144166142,0.612365187334503,0.618678230502864,
0.624991273671225,0.631304316839586,0.637617360007947,0.643930403176308,
0.650243446344669,0.656556489513031,0.662869532681392,0.669182575849753,
0.675495619018114,0.681808662186475,0.688121705354836,0.694434748523197,
0.700747791691558,0.707060834859919,0.713373878028281,0.719686921196642,
0.725999964365003,0.732313007533364,0.738626050701725,0.744939093870086,
0.751252137038447,0.757565180206808,0.763878223375169,0.770191266543531,
0.776504309711892,0.782817352880253,0.789130396048614,0.795443439216975,
0.801756482385336,0.808069525553697,0.814382568722058,0.820695611890419,
0.827008655058781,0.833321698227142,0.839634741395503,0.845947784563864,
0.852260827732225,0.858573870900586,0.864886914068947,0.871199957237308,
0.87751300040567,0.88382604357403,0.890139086742392,0.896452129910753,0.902765173079114,
0.909078216247475,0.915391259415836,0.921704302584197,0.928017345752558,
0.934330388920919,0.940643432089281,0.946956475257642,0.953269518426003,
0.959582561594364,0.965895604762725,0.972208647931086,0.978521691099447,
0.984834734267808,0.99114777743617,0.997460820604531,1.),.UNSPECIFIED.)
CURVE()
GEOMETRIC_REPRESENTATION_ITEM()
RATIONAL_B_SPLINE_CURVE((0.973018780871376,0.984780444152242,1.,0.866025403784439,
1.,0.866025403784439,1.,0.866025403784439,1.,0.866025403784439,1.,0.866025403784439,
1.,0.866025403784439,1.,0.866025403784439,1.,0.866025403784439,1.,0.866025403784439,
1.,0.866025403784439,1.,0.866025403784439,1.,0.866025403784439,1.,0.866025403784439,
1.,0.866025403784439,1.,0.866025403784439,1.,0.866025403784439,1.,0.866025403784439,
1.,0.866025403784439,1.,0.866025403784439,1.,0.866025403784439,1.,0.866025403784439,
1.,0.866025403784439,1.,0.866025403784439,1.,0.866025403784439,1.,0.866025403784439,
1.,0.866025403784439,1.,0.866025403784439,1.,0.866025403784439,1.,0.866025403784439,
1.,0.866025403784439,1.,0.866025403784439,1.,0.866025403784439,1.,0.866025403784439,
1.,0.866025403784439,1.,0.866025403784439,1.,0.866025403784439,1.,0.866025403784439,
1.,0.866025403784439,1.,0.866025403784439,1.,0.866025403784439,1.,0.866025403784439,
1.,0.866025403784439,1.,0.866025403784439,1.,0.866025403784439,1.,0.866025403784439,
1.,0.866025403784439,1.,0.866025403784439,1.,0.866025403784439,1.,0.866025403784439,
1.,0.866025403784439,1.,0.866025403784439,1.,0.866025403784439,1.,0.866025403784439,
1.,0.866025403784439,1.,0.866025403784439,1.,0.866025403784439,1.,0.866025403784439,
1.,0.866025403784439,1.,0.866025403784439,1.,0.866025403784439,1.,0.866025403784439,
1.,0.866025403784439,1.,0.866025403784439,1.,0.866025403784439,1.,0.866025403784439,
1.,0.866025403784439,1.,0.866025403784439,1.,0.866025403784439,1.,0.866025403784439,
1.,0.866025403784439,1.,0.866025403784439,1.,0.866025403784439,1.,0.866025403784439,
1.,0.866025403784439,1.,0.866025403784439,1.,0.866025403784439,1.,0.866025403784439,
1.,0.866025403784439,1.,0.866025403784439,1.,0.866025403784439,1.,0.866025403784439,
1.,0.866025403784439,1.,0.866025403784439,1.,0.866025403784439,1.,0.866025403784439,
1.,0.866025403784439,1.,0.866025403784439,1.,0.866025403784439,1.,0.866025403784439,
1.,0.866025403784439,1.,0.866025403784439,1.,0.866025403784439,1.,0.866025403784439,
1.,0.866025403784439,1.,0.866025403784439,1.,0.866025403784439,1.,0.866025403784439,
1.,0.866025403784439,1.,0.866025403784439,1.,0.866025403784439,1.,0.866025403784439,
1.,0.866025403784439,1.,0.866025403784439,1.,0.866025403784439,1.,0.866025403784439,
1.,0.866025403784439,1.,0.866025403784439,1.,0.866025403784439,1.,0.866025403784439,
1.,0.866025403784439,1.,0.866025403784439,1.,0.866025403784439,1.,0.866025403784439,
1.,0.866025403784439,1.,0.866025403784439,1.,0.866025403784439,1.,0.866025403784439,
1.,0.866025403784439,1.,0.866025403784439,1.,0.866025403784439,1.,0.866025403784439,
1.,0.866025403784439,1.,0.866025403784439,1.,0.866025403784439,1.,0.866025403784439,
1.,0.866025403784439,1.,0.866025403784439,1.,0.866025403784439,1.,0.866025403784439,
1.,0.866025403784439,1.,0.866025403784439,1.,0.866025403784439,1.,0.866025403784439,
1.,0.866025403784439,1.,0.866025403784439,1.,0.866025403784439,1.,0.866025403784439,
1.,0.866025403784439,1.,0.866025403784439,1.,0.866025403784439,1.,0.866025403784439,
1.,0.866025403784439,1.,0.866025403784439,1.,0.866025403784439,1.,0.866025403784439,
1.,0.866025403784439,1.,0.866025403784439,1.,0.866025403784439,1.,0.946114646713198,
0.93557529156132))
REPRESENTATION_ITEM('')
);
#267=(
BOUNDED_CURVE()
B_SPLINE_CURVE(2,(#27292,#27293,#27294,#27295,#27296,#27297,#27298,#27299,
#27300,#27301,#27302,#27303,#27304,#27305,#27306,#27307,#27308,#27309,#27310,
#27311,#27312,#27313,#27314,#27315,#27316,#27317,#27318,#27319,#27320,#27321,
#27322,#27323,#27324,#27325,#27326,#27327,#27328,#27329,#27330,#27331,#27332,
#27333,#27334,#27335,#27336,#27337,#27338,#27339,#27340,#27341,#27342,#27343,
#27344,#27345,#27346,#27347,#27348,#27349,#27350,#27351,#27352,#27353,#27354,
#27355,#27356,#27357,#27358,#27359,#27360,#27361,#27362,#27363,#27364,#27365,
#27366,#27367,#27368,#27369,#27370,#27371,#27372,#27373,#27374,#27375,#27376,
#27377,#27378,#27379,#27380,#27381,#27382,#27383,#27384,#27385,#27386,#27387,
#27388,#27389,#27390,#27391,#27392,#27393,#27394,#27395,#27396,#27397,#27398,
#27399,#27400,#27401,#27402,#27403,#27404,#27405,#27406,#27407,#27408,#27409,
#27410,#27411,#27412,#27413,#27414,#27415,#27416,#27417,#27418,#27419,#27420,
#27421,#27422,#27423,#27424,#27425,#27426,#27427,#27428,#27429,#27430,#27431,
#27432,#27433,#27434,#27435,#27436,#27437,#27438,#27439,#27440,#27441,#27442,
#27443,#27444,#27445,#27446,#27447,#27448,#27449,#27450,#27451,#27452,#27453,
#27454,#27455,#27456,#27457,#27458,#27459,#27460,#27461,#27462,#27463,#27464,
#27465,#27466,#27467,#27468,#27469,#27470,#27471,#27472,#27473,#27474,#27475,
#27476,#27477,#27478,#27479,#27480,#27481,#27482,#27483,#27484,#27485,#27486,
#27487,#27488,#27489,#27490,#27491,#27492,#27493,#27494,#27495,#27496,#27497,
#27498,#27499,#27500,#27501,#27502,#27503,#27504,#27505,#27506,#27507,#27508,
#27509,#27510,#27511,#27512,#27513,#27514,#27515,#27516,#27517,#27518,#27519,
#27520,#27521,#27522,#27523,#27524,#27525,#27526,#27527,#27528,#27529,#27530,
#27531,#27532,#27533,#27534,#27535,#27536,#27537,#27538,#27539,#27540,#27541,
#27542,#27543,#27544,#27545,#27546,#27547,#27548,#27549,#27550,#27551,#27552,
#27553,#27554,#27555,#27556,#27557,#27558,#27559,#27560,#27561,#27562,#27563,
#27564,#27565,#27566,#27567,#27568,#27569,#27570,#27571,#27572,#27573,#27574,
#27575,#27576,#27577,#27578,#27579,#27580,#27581,#27582,#27583,#27584,#27585,
#27586,#27587,#27588,#27589,#27590,#27591,#27592),.UNSPECIFIED.,.F.,.F.)
B_SPLINE_CURVE_WITH_KNOTS((3,2,2,2,2,2,2,2,2,2,2,2,2,2,2,2,2,2,2,2,2,2,
2,2,2,2,2,2,2,2,2,2,2,2,2,2,2,2,2,2,2,2,2,2,2,2,2,2,2,2,2,2,2,2,2,2,2,2,
2,2,2,2,2,2,2,2,2,2,2,2,2,2,2,2,2,2,2,2,2,2,2,2,2,2,2,2,2,2,2,2,2,2,2,2,
2,2,2,2,2,2,2,2,2,2,2,2,2,2,2,2,2,2,2,2,2,2,2,2,2,2,2,2,2,2,2,2,2,2,2,2,
2,2,2,2,2,2,2,2,2,2,2,2,2,2,2,2,2,2,2,2,3),(0.0578262804341777,0.0631304340270661,
0.0694434774297724,0.0757565208324788,0.0820695642351851,0.0883826076378915,
0.0946956510405978,0.101008694443304,0.107321737846011,0.113634781248717,
0.119947824651423,0.12626086805413,0.132573911456836,0.138886954859542,
0.145199998262249,0.151513041664955,0.157826085067661,0.164139128470368,
0.170452171873074,0.17676521527578,0.183078258678487,0.189391302081193,
0.195704345483899,0.202017388886606,0.208330432289312,0.214643475692019,
0.220956519094725,0.227269562497431,0.233582605900138,0.239895649302844,
0.24620869270555,0.252521736108257,0.258834779510963,0.265147822913669,
0.271460866316376,0.277773909719082,0.284086953121788,0.290399996524495,
0.296713039927201,0.303026083329908,0.309339126732614,0.31565217013532,
0.321965213538027,0.328278256940733,0.334591300343439,0.340904343746146,
0.347217387148852,0.353530430551558,0.359843473954265,0.366156517356971,
0.372469560759677,0.378782604162384,0.38509564756509,0.391408690967797,
0.397721734370503,0.404034777773209,0.410347821175916,0.416660864578622,
0.422973907981328,0.429286951384035,0.435599994786741,0.441913038189447,
0.448226081592154,0.45453912499486,0.460852168397566,0.467165211800273,
0.473478255202979,0.479791298605685,0.486104342008392,0.492417385411098,
0.498730428813805,0.505043472216511,0.511356515619217,0.517669559021924,
0.52398260242463,0.530295645827336,0.536608689230043,0.542921732632749,
0.549234776035455,0.555547819438162,0.561860862840868,0.568173906243575,
0.574486949646281,0.580799993048987,0.587113036451693,0.5934260798544,0.599739123257106,
0.606052166659813,0.612365210062519,0.618678253465225,0.624991296867932,
0.631304340270638,0.637617383673344,0.643930427076051,0.650243470478757,
0.656556513881463,0.66286955728417,0.669182600686876,0.675495644089582,
0.681808687492289,0.688121730894995,0.694434774297702,0.700747817700408,
0.707060861103114,0.71337390450582,0.719686947908527,0.725999991311233,
0.732313034713939,0.738626078116646,0.744939121519352,0.751252164922059,
0.757565208324765,0.763878251727471,0.770191295130178,0.776504338532884,
0.78281738193559,0.789130425338297,0.795443468741003,0.80175651214371,0.808069555546416,
0.814382598949122,0.820695642351829,0.827008685754535,0.833321729157241,
0.839634772559948,0.845947815962654,0.85226085936536,0.858573902768067,
0.864886946170773,0.871199989573479,0.877513032976186,0.883826076378892,
0.890139119781598,0.896452163184305,0.902765206587011,0.909078249989718,
0.915391293392424,0.92170433679513,0.928017380197837,0.934330423600543,
0.940643467003249,0.946956510405956,0.953269553808662,0.959582597211368,
0.965895640614075,0.972208684016781,0.978521727419488,0.984834770822194,
0.9911478142249,0.997460857627607,1.),.UNSPECIFIED.)
CURVE()
GEOMETRIC_REPRESENTATION_ITEM()
RATIONAL_B_SPLINE_CURVE((0.964022189566827,0.887435933741894,1.,0.866025403784439,
1.,0.866025403784439,1.,0.866025403784439,1.,0.866025403784439,1.,0.866025403784439,
1.,0.866025403784439,1.,0.866025403784439,1.,0.866025403784439,1.,0.866025403784439,
1.,0.866025403784439,1.,0.866025403784439,1.,0.866025403784439,1.,0.866025403784439,
1.,0.866025403784439,1.,0.866025403784439,1.,0.866025403784439,1.,0.866025403784439,
1.,0.866025403784439,1.,0.866025403784439,1.,0.866025403784439,1.,0.866025403784439,
1.,0.866025403784439,1.,0.866025403784439,1.,0.866025403784439,1.,0.866025403784439,
1.,0.866025403784439,1.,0.866025403784439,1.,0.866025403784439,1.,0.866025403784439,
1.,0.866025403784439,1.,0.866025403784439,1.,0.866025403784439,1.,0.866025403784439,
1.,0.866025403784439,1.,0.866025403784439,1.,0.866025403784439,1.,0.866025403784439,
1.,0.866025403784439,1.,0.866025403784439,1.,0.866025403784439,1.,0.866025403784439,
1.,0.866025403784439,1.,0.866025403784439,1.,0.866025403784439,1.,0.866025403784439,
1.,0.866025403784439,1.,0.866025403784439,1.,0.866025403784439,1.,0.866025403784439,
1.,0.866025403784439,1.,0.866025403784439,1.,0.866025403784439,1.,0.866025403784439,
1.,0.866025403784439,1.,0.866025403784439,1.,0.866025403784439,1.,0.866025403784439,
1.,0.866025403784439,1.,0.866025403784439,1.,0.866025403784439,1.,0.866025403784439,
1.,0.866025403784439,1.,0.866025403784439,1.,0.866025403784439,1.,0.866025403784439,
1.,0.866025403784439,1.,0.866025403784439,1.,0.866025403784439,1.,0.866025403784439,
1.,0.866025403784439,1.,0.866025403784439,1.,0.866025403784439,1.,0.866025403784439,
1.,0.866025403784439,1.,0.866025403784439,1.,0.866025403784439,1.,0.866025403784439,
1.,0.866025403784439,1.,0.866025403784439,1.,0.866025403784439,1.,0.866025403784439,
1.,0.866025403784439,1.,0.866025403784439,1.,0.866025403784439,1.,0.866025403784439,
1.,0.866025403784439,1.,0.866025403784439,1.,0.866025403784439,1.,0.866025403784439,
1.,0.866025403784439,1.,0.866025403784439,1.,0.866025403784439,1.,0.866025403784439,
1.,0.866025403784439,1.,0.866025403784439,1.,0.866025403784439,1.,0.866025403784439,
1.,0.866025403784439,1.,0.866025403784439,1.,0.866025403784439,1.,0.866025403784439,
1.,0.866025403784439,1.,0.866025403784439,1.,0.866025403784439,1.,0.866025403784439,
1.,0.866025403784439,1.,0.866025403784439,1.,0.866025403784439,1.,0.866025403784439,
1.,0.866025403784439,1.,0.866025403784439,1.,0.866025403784439,1.,0.866025403784439,
1.,0.866025403784439,1.,0.866025403784439,1.,0.866025403784439,1.,0.866025403784439,
1.,0.866025403784439,1.,0.866025403784439,1.,0.866025403784439,1.,0.866025403784439,
1.,0.866025403784439,1.,0.866025403784439,1.,0.866025403784439,1.,0.866025403784439,
1.,0.866025403784439,1.,0.866025403784439,1.,0.866025403784439,1.,0.866025403784439,
1.,0.866025403784439,1.,0.866025403784439,1.,0.866025403784439,1.,0.866025403784439,
1.,0.866025403784439,1.,0.866025403784439,1.,0.866025403784439,1.,0.866025403784439,
1.,0.866025403784439,1.,0.866025403784439,1.,0.866025403784439,1.,0.866025403784439,
1.,0.866025403784439,1.,0.866025403784439,1.,0.866025403784439,1.,0.866025403784439,
1.,0.866025403784439,1.,0.866025403784439,1.,0.866025403784439,1.,0.946114646712328,
0.93557529156098))
REPRESENTATION_ITEM('')
);
#268=(
BOUNDED_CURVE()
B_SPLINE_CURVE(2,(#28234,#28235,#28236,#28237,#28238,#28239,#28240,#28241,
#28242,#28243,#28244,#28245,#28246,#28247,#28248,#28249,#28250,#28251,#28252,
#28253,#28254,#28255,#28256,#28257,#28258,#28259,#28260,#28261,#28262,#28263,
#28264,#28265,#28266,#28267,#28268,#28269,#28270,#28271,#28272,#28273,#28274,
#28275,#28276,#28277,#28278,#28279,#28280,#28281,#28282,#28283,#28284,#28285,
#28286,#28287,#28288,#28289,#28290,#28291,#28292,#28293,#28294,#28295,#28296,
#28297,#28298,#28299,#28300,#28301,#28302,#28303,#28304,#28305,#28306,#28307,
#28308,#28309,#28310,#28311,#28312,#28313,#28314,#28315,#28316,#28317,#28318,
#28319,#28320,#28321,#28322,#28323,#28324,#28325,#28326,#28327,#28328,#28329,
#28330,#28331,#28332,#28333,#28334,#28335,#28336,#28337,#28338,#28339,#28340,
#28341,#28342,#28343,#28344,#28345,#28346,#28347,#28348,#28349,#28350,#28351,
#28352,#28353,#28354,#28355,#28356,#28357,#28358,#28359,#28360,#28361,#28362,
#28363,#28364,#28365,#28366,#28367,#28368,#28369,#28370,#28371,#28372,#28373,
#28374,#28375,#28376,#28377,#28378,#28379,#28380,#28381,#28382,#28383,#28384,
#28385,#28386,#28387,#28388,#28389,#28390,#28391,#28392,#28393,#28394,#28395,
#28396,#28397,#28398,#28399,#28400,#28401,#28402,#28403,#28404,#28405,#28406,
#28407,#28408,#28409,#28410,#28411,#28412,#28413,#28414,#28415,#28416,#28417,
#28418,#28419,#28420,#28421,#28422,#28423,#28424,#28425,#28426,#28427,#28428,
#28429,#28430,#28431,#28432,#28433,#28434,#28435,#28436,#28437,#28438,#28439,
#28440,#28441,#28442,#28443,#28444,#28445,#28446,#28447,#28448,#28449,#28450,
#28451,#28452,#28453,#28454,#28455,#28456,#28457,#28458,#28459,#28460,#28461,
#28462,#28463,#28464,#28465,#28466,#28467,#28468,#28469,#28470,#28471,#28472,
#28473,#28474,#28475,#28476,#28477,#28478,#28479,#28480,#28481,#28482,#28483,
#28484,#28485,#28486,#28487,#28488,#28489,#28490,#28491,#28492,#28493,#28494,
#28495,#28496,#28497,#28498,#28499,#28500,#28501,#28502,#28503,#28504,#28505,
#28506,#28507,#28508,#28509,#28510,#28511,#28512,#28513,#28514,#28515,#28516,
#28517,#28518,#28519,#28520,#28521,#28522,#28523,#28524,#28525,#28526,#28527,
#28528,#28529,#28530,#28531,#28532,#28533,#28534),.UNSPECIFIED.,.F.,.F.)
B_SPLINE_CURVE_WITH_KNOTS((3,2,2,2,2,2,2,2,2,2,2,2,2,2,2,2,2,2,2,2,2,2,
2,2,2,2,2,2,2,2,2,2,2,2,2,2,2,2,2,2,2,2,2,2,2,2,2,2,2,2,2,2,2,2,2,2,2,2,
2,2,2,2,2,2,2,2,2,2,2,2,2,2,2,2,2,2,2,2,2,2,2,2,2,2,2,2,2,2,2,2,2,2,2,2,
2,2,2,2,2,2,2,2,2,2,2,2,2,2,2,2,2,2,2,2,2,2,2,2,2,2,2,2,2,2,2,2,2,2,2,2,
2,2,2,2,2,2,2,2,2,2,2,2,2,2,2,2,2,2,2,2,3),(0.0624132680173737,0.0631304316871764,
0.0694434748563336,0.0757565180254908,0.082069561194648,0.0883826043638051,
0.0946956475329623,0.101008690702119,0.107321733871277,0.113634777040434,
0.119947820209591,0.126260863378748,0.132573906547905,0.138886949717063,
0.14519999288622,0.151513036055377,0.157826079224534,0.164139122393691,
0.170452165562848,0.176765208732006,0.183078251901163,0.18939129507032,
0.195704338239477,0.202017381408634,0.208330424577791,0.214643467746949,
0.220956510916106,0.227269554085263,0.23358259725442,0.239895640423577,
0.246208683592735,0.252521726761892,0.258834769931049,0.265147813100206,
0.271460856269363,0.27777389943852,0.284086942607678,0.290399985776835,
0.296713028945992,0.303026072115149,0.309339115284306,0.315652158453464,
0.321965201622621,0.328278244791778,0.334591287960935,0.340904331130092,
0.347217374299249,0.353530417468407,0.359843460637564,0.366156503806721,
0.372469546975878,0.378782590145035,0.385095633314192,0.39140867648335,
0.397721719652507,0.404034762821664,0.410347805990821,0.416660849159978,
0.422973892329136,0.429286935498293,0.43559997866745,0.441913021836607,
0.448226065005764,0.454539108174921,0.460852151344079,0.467165194513236,
0.473478237682393,0.47979128085155,0.486104324020707,0.492417367189865,
0.498730410359022,0.505043453528179,0.511356496697336,0.517669539866493,
0.52398258303565,0.530295626204808,0.536608669373965,0.542921712543122,
0.549234755712279,0.555547798881436,0.561860842050594,0.568173885219751,
0.574486928388908,0.580799971558065,0.587113014727222,0.593426057896379,
0.599739101065537,0.606052144234694,0.612365187403851,0.618678230573008,
0.624991273742165,0.631304316911322,0.63761736008048,0.643930403249637,
0.650243446418794,0.656556489587951,0.662869532757108,0.669182575926266,
0.675495619095423,0.68180866226458,0.688121705433737,0.694434748602894,
0.700747791772051,0.707060834941208,0.713373878110366,0.719686921279523,
0.72599996444868,0.732313007617837,0.738626050786994,0.744939093956152,
0.751252137125309,0.757565180294466,0.763878223463623,0.77019126663278,
0.776504309801938,0.782817352971095,0.789130396140252,0.795443439309409,
0.801756482478566,0.808069525647723,0.814382568816881,0.820695611986038,
0.827008655155195,0.833321698324352,0.839634741493509,0.845947784662667,
0.852260827831824,0.858573871000981,0.864886914170138,0.871199957339295,
0.877513000508452,0.883826043677609,0.890139086846767,0.896452130015924,
0.902765173185081,0.909078216354238,0.915391259523395,0.921704302692553,
0.92801734586171,0.934330389030867,0.940643432200024,0.946956475369181,
0.953269518538338,0.959582561707496,0.965895604876653,0.97220864804581,
0.978521691214967,0.984834734384124,0.991147777553281,0.997460820722439,
1.),.UNSPECIFIED.)
CURVE()
GEOMETRIC_REPRESENTATION_ITEM()
RATIONAL_B_SPLINE_CURVE((0.973018780871375,0.984780444152242,1.,0.866025403784439,
1.,0.866025403784439,1.,0.866025403784439,1.,0.866025403784439,1.,0.866025403784439,
1.,0.866025403784439,1.,0.866025403784439,1.,0.866025403784439,1.,0.866025403784439,
1.,0.866025403784439,1.,0.866025403784439,1.,0.866025403784439,1.,0.866025403784439,
1.,0.866025403784439,1.,0.866025403784439,1.,0.866025403784439,1.,0.866025403784439,
1.,0.866025403784439,1.,0.866025403784439,1.,0.866025403784439,1.,0.866025403784439,
1.,0.866025403784439,1.,0.866025403784439,1.,0.866025403784439,1.,0.866025403784439,
1.,0.866025403784439,1.,0.866025403784439,1.,0.866025403784439,1.,0.866025403784439,
1.,0.866025403784439,1.,0.866025403784439,1.,0.866025403784439,1.,0.866025403784439,
1.,0.866025403784439,1.,0.866025403784439,1.,0.866025403784439,1.,0.866025403784439,
1.,0.866025403784439,1.,0.866025403784439,1.,0.866025403784439,1.,0.866025403784439,
1.,0.866025403784439,1.,0.866025403784439,1.,0.866025403784439,1.,0.866025403784439,
1.,0.866025403784439,1.,0.866025403784439,1.,0.866025403784439,1.,0.866025403784439,
1.,0.866025403784439,1.,0.866025403784439,1.,0.866025403784439,1.,0.866025403784439,
1.,0.866025403784439,1.,0.866025403784439,1.,0.866025403784439,1.,0.866025403784439,
1.,0.866025403784439,1.,0.866025403784439,1.,0.866025403784439,1.,0.866025403784439,
1.,0.866025403784439,1.,0.866025403784439,1.,0.866025403784439,1.,0.866025403784439,
1.,0.866025403784439,1.,0.866025403784439,1.,0.866025403784439,1.,0.866025403784439,
1.,0.866025403784439,1.,0.866025403784439,1.,0.866025403784439,1.,0.866025403784439,
1.,0.866025403784439,1.,0.866025403784439,1.,0.866025403784439,1.,0.866025403784439,
1.,0.866025403784439,1.,0.866025403784439,1.,0.866025403784439,1.,0.866025403784439,
1.,0.866025403784439,1.,0.866025403784439,1.,0.866025403784439,1.,0.866025403784439,
1.,0.866025403784439,1.,0.866025403784439,1.,0.866025403784439,1.,0.866025403784439,
1.,0.866025403784439,1.,0.866025403784439,1.,0.866025403784439,1.,0.866025403784439,
1.,0.866025403784439,1.,0.866025403784439,1.,0.866025403784439,1.,0.866025403784439,
1.,0.866025403784439,1.,0.866025403784439,1.,0.866025403784439,1.,0.866025403784439,
1.,0.866025403784439,1.,0.866025403784439,1.,0.866025403784439,1.,0.866025403784439,
1.,0.866025403784439,1.,0.866025403784439,1.,0.866025403784439,1.,0.866025403784439,
1.,0.866025403784439,1.,0.866025403784439,1.,0.866025403784439,1.,0.866025403784439,
1.,0.866025403784439,1.,0.866025403784439,1.,0.866025403784439,1.,0.866025403784439,
1.,0.866025403784439,1.,0.866025403784439,1.,0.866025403784439,1.,0.866025403784439,
1.,0.866025403784439,1.,0.866025403784439,1.,0.866025403784439,1.,0.866025403784439,
1.,0.866025403784439,1.,0.866025403784439,1.,0.866025403784439,1.,0.866025403784439,
1.,0.866025403784439,1.,0.866025403784439,1.,0.866025403784439,1.,0.866025403784439,
1.,0.866025403784439,1.,0.866025403784439,1.,0.866025403784439,1.,0.866025403784439,
1.,0.866025403784439,1.,0.866025403784439,1.,0.866025403784439,1.,0.866025403784439,
1.,0.866025403784439,1.,0.866025403784439,1.,0.866025403784439,1.,0.866025403784439,
1.,0.866025403784439,1.,0.866025403784439,1.,0.866025403784439,1.,0.946114646713198,
0.93557529156132))
REPRESENTATION_ITEM('')
);
#269=(
BOUNDED_CURVE()
B_SPLINE_CURVE(2,(#29818,#29819,#29820,#29821,#29822,#29823,#29824,#29825,
#29826,#29827,#29828,#29829,#29830,#29831,#29832,#29833,#29834,#29835,#29836,
#29837,#29838,#29839,#29840,#29841,#29842,#29843,#29844,#29845,#29846,#29847,
#29848,#29849,#29850,#29851,#29852,#29853,#29854,#29855,#29856,#29857,#29858,
#29859,#29860,#29861,#29862,#29863,#29864,#29865,#29866,#29867,#29868,#29869,
#29870,#29871,#29872,#29873,#29874,#29875,#29876,#29877,#29878,#29879,#29880,
#29881,#29882,#29883,#29884,#29885,#29886,#29887,#29888,#29889,#29890,#29891,
#29892,#29893,#29894,#29895,#29896,#29897,#29898,#29899,#29900,#29901,#29902,
#29903,#29904,#29905,#29906,#29907,#29908,#29909,#29910,#29911,#29912,#29913,
#29914,#29915,#29916,#29917,#29918,#29919,#29920,#29921,#29922,#29923,#29924,
#29925,#29926,#29927,#29928,#29929,#29930,#29931,#29932,#29933,#29934,#29935,
#29936,#29937,#29938,#29939,#29940,#29941,#29942,#29943,#29944,#29945,#29946,
#29947,#29948,#29949,#29950,#29951,#29952,#29953,#29954,#29955,#29956,#29957,
#29958,#29959,#29960,#29961,#29962,#29963,#29964,#29965,#29966,#29967,#29968,
#29969,#29970,#29971,#29972,#29973,#29974,#29975,#29976,#29977,#29978,#29979,
#29980,#29981,#29982,#29983,#29984,#29985,#29986,#29987,#29988,#29989,#29990,
#29991,#29992,#29993,#29994,#29995,#29996,#29997,#29998,#29999,#30000,#30001,
#30002,#30003,#30004,#30005,#30006,#30007,#30008,#30009,#30010,#30011,#30012,
#30013,#30014,#30015,#30016,#30017,#30018,#30019,#30020,#30021,#30022,#30023,
#30024,#30025,#30026,#30027,#30028,#30029,#30030,#30031,#30032,#30033,#30034,
#30035,#30036,#30037,#30038,#30039,#30040,#30041,#30042,#30043,#30044,#30045,
#30046,#30047,#30048,#30049,#30050,#30051,#30052,#30053,#30054,#30055,#30056,
#30057,#30058,#30059,#30060,#30061,#30062,#30063,#30064,#30065,#30066,#30067,
#30068,#30069,#30070,#30071,#30072,#30073,#30074,#30075,#30076,#30077,#30078,
#30079,#30080,#30081,#30082,#30083,#30084,#30085,#30086,#30087,#30088,#30089,
#30090,#30091,#30092,#30093,#30094,#30095,#30096,#30097,#30098,#30099,#30100,
#30101,#30102,#30103,#30104,#30105,#30106,#30107,#30108,#30109,#30110,#30111,
#30112,#30113,#30114,#30115,#30116,#30117,#30118),.UNSPECIFIED.,.F.,.F.)
B_SPLINE_CURVE_WITH_KNOTS((3,2,2,2,2,2,2,2,2,2,2,2,2,2,2,2,2,2,2,2,2,2,
2,2,2,2,2,2,2,2,2,2,2,2,2,2,2,2,2,2,2,2,2,2,2,2,2,2,2,2,2,2,2,2,2,2,2,2,
2,2,2,2,2,2,2,2,2,2,2,2,2,2,2,2,2,2,2,2,2,2,2,2,2,2,2,2,2,2,2,2,2,2,2,2,
2,2,2,2,2,2,2,2,2,2,2,2,2,2,2,2,2,2,2,2,2,2,2,2,2,2,2,2,2,2,2,2,2,2,2,2,
2,2,2,2,2,2,2,2,2,2,2,2,2,2,2,2,2,2,2,2,3),(0.0578262804341777,0.063130434027066,
0.0694434774297724,0.0757565208324788,0.0820695642351851,0.0883826076378915,
0.0946956510405978,0.101008694443304,0.107321737846011,0.113634781248717,
0.119947824651423,0.12626086805413,0.132573911456836,0.138886954859542,
0.145199998262249,0.151513041664955,0.157826085067661,0.164139128470368,
0.170452171873074,0.17676521527578,0.183078258678487,0.189391302081193,
0.195704345483899,0.202017388886606,0.208330432289312,0.214643475692019,
0.220956519094725,0.227269562497431,0.233582605900138,0.239895649302844,
0.24620869270555,0.252521736108257,0.258834779510963,0.265147822913669,
0.271460866316376,0.277773909719082,0.284086953121788,0.290399996524495,
0.296713039927201,0.303026083329907,0.309339126732614,0.31565217013532,
0.321965213538027,0.328278256940733,0.334591300343439,0.340904343746146,
0.347217387148852,0.353530430551558,0.359843473954265,0.366156517356971,
0.372469560759677,0.378782604162384,0.38509564756509,0.391408690967797,
0.397721734370503,0.404034777773209,0.410347821175916,0.416660864578622,
0.422973907981328,0.429286951384035,0.435599994786741,0.441913038189447,
0.448226081592154,0.45453912499486,0.460852168397566,0.467165211800273,
0.473478255202979,0.479791298605685,0.486104342008392,0.492417385411098,
0.498730428813805,0.505043472216511,0.511356515619217,0.517669559021924,
0.52398260242463,0.530295645827336,0.536608689230043,0.542921732632749,
0.549234776035455,0.555547819438162,0.561860862840868,0.568173906243575,
0.574486949646281,0.580799993048987,0.587113036451693,0.5934260798544,0.599739123257106,
0.606052166659813,0.612365210062519,0.618678253465225,0.624991296867932,
0.631304340270638,0.637617383673344,0.643930427076051,0.650243470478757,
0.656556513881463,0.66286955728417,0.669182600686876,0.675495644089582,
0.681808687492289,0.688121730894995,0.694434774297702,0.700747817700408,
0.707060861103114,0.71337390450582,0.719686947908527,0.725999991311233,
0.732313034713939,0.738626078116646,0.744939121519352,0.751252164922059,
0.757565208324765,0.763878251727471,0.770191295130178,0.776504338532884,
0.78281738193559,0.789130425338297,0.795443468741003,0.80175651214371,0.808069555546416,
0.814382598949122,0.820695642351829,0.827008685754535,0.833321729157241,
0.839634772559948,0.845947815962654,0.85226085936536,0.858573902768067,
0.864886946170773,0.871199989573479,0.877513032976186,0.883826076378892,
0.890139119781598,0.896452163184305,0.902765206587011,0.909078249989718,
0.915391293392424,0.92170433679513,0.928017380197837,0.934330423600543,
0.940643467003249,0.946956510405956,0.953269553808662,0.959582597211368,
0.965895640614075,0.972208684016781,0.978521727419488,0.984834770822194,
0.9911478142249,0.997460857627607,1.),.UNSPECIFIED.)
CURVE()
GEOMETRIC_REPRESENTATION_ITEM()
RATIONAL_B_SPLINE_CURVE((0.964022189566827,0.887435933741894,1.,0.866025403784439,
1.,0.866025403784439,1.,0.866025403784439,1.,0.866025403784439,1.,0.866025403784439,
1.,0.866025403784439,1.,0.866025403784439,1.,0.866025403784439,1.,0.866025403784439,
1.,0.866025403784439,1.,0.866025403784439,1.,0.866025403784439,1.,0.866025403784439,
1.,0.866025403784439,1.,0.866025403784439,1.,0.866025403784439,1.,0.866025403784439,
1.,0.866025403784439,1.,0.866025403784439,1.,0.866025403784439,1.,0.866025403784439,
1.,0.866025403784439,1.,0.866025403784439,1.,0.866025403784439,1.,0.866025403784439,
1.,0.866025403784439,1.,0.866025403784439,1.,0.866025403784439,1.,0.866025403784439,
1.,0.866025403784439,1.,0.866025403784439,1.,0.866025403784439,1.,0.866025403784439,
1.,0.866025403784439,1.,0.866025403784439,1.,0.866025403784439,1.,0.866025403784439,
1.,0.866025403784439,1.,0.866025403784439,1.,0.866025403784439,1.,0.866025403784439,
1.,0.866025403784439,1.,0.866025403784439,1.,0.866025403784439,1.,0.866025403784439,
1.,0.866025403784439,1.,0.866025403784439,1.,0.866025403784439,1.,0.866025403784439,
1.,0.866025403784439,1.,0.866025403784439,1.,0.866025403784439,1.,0.866025403784439,
1.,0.866025403784439,1.,0.866025403784439,1.,0.866025403784439,1.,0.866025403784439,
1.,0.866025403784439,1.,0.866025403784439,1.,0.866025403784439,1.,0.866025403784439,
1.,0.866025403784439,1.,0.866025403784439,1.,0.866025403784439,1.,0.866025403784439,
1.,0.866025403784439,1.,0.866025403784439,1.,0.866025403784439,1.,0.866025403784439,
1.,0.866025403784439,1.,0.866025403784439,1.,0.866025403784439,1.,0.866025403784439,
1.,0.866025403784439,1.,0.866025403784439,1.,0.866025403784439,1.,0.866025403784439,
1.,0.866025403784439,1.,0.866025403784439,1.,0.866025403784439,1.,0.866025403784439,
1.,0.866025403784439,1.,0.866025403784439,1.,0.866025403784439,1.,0.866025403784439,
1.,0.866025403784439,1.,0.866025403784439,1.,0.866025403784439,1.,0.866025403784439,
1.,0.866025403784439,1.,0.866025403784439,1.,0.866025403784439,1.,0.866025403784439,
1.,0.866025403784439,1.,0.866025403784439,1.,0.866025403784439,1.,0.866025403784439,
1.,0.866025403784439,1.,0.866025403784439,1.,0.866025403784439,1.,0.866025403784439,
1.,0.866025403784439,1.,0.866025403784439,1.,0.866025403784439,1.,0.866025403784439,
1.,0.866025403784439,1.,0.866025403784439,1.,0.866025403784439,1.,0.866025403784439,
1.,0.866025403784439,1.,0.866025403784439,1.,0.866025403784439,1.,0.866025403784439,
1.,0.866025403784439,1.,0.866025403784439,1.,0.866025403784439,1.,0.866025403784439,
1.,0.866025403784439,1.,0.866025403784439,1.,0.866025403784439,1.,0.866025403784439,
1.,0.866025403784439,1.,0.866025403784439,1.,0.866025403784439,1.,0.866025403784439,
1.,0.866025403784439,1.,0.866025403784439,1.,0.866025403784439,1.,0.866025403784439,
1.,0.866025403784439,1.,0.866025403784439,1.,0.866025403784439,1.,0.866025403784439,
1.,0.866025403784439,1.,0.866025403784439,1.,0.866025403784439,1.,0.866025403784439,
1.,0.866025403784439,1.,0.866025403784439,1.,0.866025403784439,1.,0.866025403784439,
1.,0.866025403784439,1.,0.866025403784439,1.,0.866025403784439,1.,0.866025403784439,
1.,0.866025403784439,1.,0.866025403784439,1.,0.866025403784439,1.,0.946114646712328,
0.93557529156098))
REPRESENTATION_ITEM('')
);
#270=(
BOUNDED_CURVE()
B_SPLINE_CURVE(2,(#30760,#30761,#30762,#30763,#30764,#30765,#30766,#30767,
#30768,#30769,#30770,#30771,#30772,#30773,#30774,#30775,#30776,#30777,#30778,
#30779,#30780,#30781,#30782,#30783,#30784,#30785,#30786,#30787,#30788,#30789,
#30790,#30791,#30792,#30793,#30794,#30795,#30796,#30797,#30798,#30799,#30800,
#30801,#30802,#30803,#30804,#30805,#30806,#30807,#30808,#30809,#30810,#30811,
#30812,#30813,#30814,#30815,#30816,#30817,#30818,#30819,#30820,#30821,#30822,
#30823,#30824,#30825,#30826,#30827,#30828,#30829,#30830,#30831,#30832,#30833,
#30834,#30835,#30836,#30837,#30838,#30839,#30840,#30841,#30842,#30843,#30844,
#30845,#30846,#30847,#30848,#30849,#30850,#30851,#30852,#30853,#30854,#30855,
#30856,#30857,#30858,#30859,#30860,#30861,#30862,#30863,#30864,#30865,#30866,
#30867,#30868,#30869,#30870,#30871,#30872,#30873,#30874,#30875,#30876,#30877,
#30878,#30879,#30880,#30881,#30882,#30883,#30884,#30885,#30886,#30887,#30888,
#30889,#30890,#30891,#30892,#30893,#30894,#30895,#30896,#30897,#30898,#30899,
#30900,#30901,#30902,#30903,#30904,#30905,#30906,#30907,#30908,#30909,#30910,
#30911,#30912,#30913,#30914,#30915,#30916,#30917,#30918,#30919,#30920,#30921,
#30922,#30923,#30924,#30925,#30926,#30927,#30928,#30929,#30930,#30931,#30932,
#30933,#30934,#30935,#30936,#30937,#30938,#30939,#30940,#30941,#30942,#30943,
#30944,#30945,#30946,#30947,#30948,#30949,#30950,#30951,#30952,#30953,#30954,
#30955,#30956,#30957,#30958,#30959,#30960,#30961,#30962,#30963,#30964,#30965,
#30966,#30967,#30968,#30969,#30970,#30971,#30972,#30973,#30974,#30975,#30976,
#30977,#30978,#30979,#30980,#30981,#30982,#30983,#30984,#30985,#30986,#30987,
#30988,#30989,#30990,#30991,#30992,#30993,#30994,#30995,#30996,#30997,#30998,
#30999,#31000,#31001,#31002,#31003,#31004,#31005,#31006,#31007,#31008,#31009,
#31010,#31011,#31012,#31013,#31014,#31015,#31016,#31017,#31018,#31019,#31020,
#31021,#31022,#31023,#31024,#31025,#31026,#31027,#31028,#31029,#31030,#31031,
#31032,#31033,#31034,#31035,#31036,#31037,#31038,#31039,#31040,#31041,#31042,
#31043,#31044,#31045,#31046,#31047,#31048,#31049,#31050,#31051,#31052,#31053,
#31054,#31055,#31056,#31057,#31058,#31059,#31060),.UNSPECIFIED.,.F.,.F.)
B_SPLINE_CURVE_WITH_KNOTS((3,2,2,2,2,2,2,2,2,2,2,2,2,2,2,2,2,2,2,2,2,2,
2,2,2,2,2,2,2,2,2,2,2,2,2,2,2,2,2,2,2,2,2,2,2,2,2,2,2,2,2,2,2,2,2,2,2,2,
2,2,2,2,2,2,2,2,2,2,2,2,2,2,2,2,2,2,2,2,2,2,2,2,2,2,2,2,2,2,2,2,2,2,2,2,
2,2,2,2,2,2,2,2,2,2,2,2,2,2,2,2,2,2,2,2,2,2,2,2,2,2,2,2,2,2,2,2,2,2,2,2,
2,2,2,2,2,2,2,2,2,2,2,2,2,2,2,2,2,2,2,2,3),(0.0624132680173737,0.0631304316870872,
0.0694434748554592,0.0757565180238312,0.0820695611922032,0.0883826043605751,
0.0946956475289471,0.101008690697319,0.107321733865691,0.113634777034063,
0.119947820202435,0.126260863370807,0.132573906539179,0.138886949707551,
0.145199992875923,0.151513036044295,0.157826079212667,0.164139122381039,
0.170452165549411,0.176765208717783,0.183078251886155,0.189391295054527,
0.195704338222899,0.202017381391271,0.208330424559643,0.214643467728015,
0.220956510896387,0.227269554064759,0.233582597233131,0.239895640401503,
0.246208683569875,0.252521726738247,0.258834769906619,0.26514781307499,
0.271460856243362,0.277773899411734,0.284086942580106,0.290399985748478,
0.29671302891685,0.303026072085222,0.309339115253594,0.315652158421966,
0.321965201590338,0.32827824475871,0.334591287927082,0.340904331095454,
0.347217374263826,0.353530417432198,0.35984346060057,0.366156503768942,
0.372469546937314,0.378782590105686,0.385095633274058,0.39140867644243,
0.397721719610802,0.404034762779174,0.410347805947546,0.416660849115918,
0.42297389228429,0.429286935452662,0.435599978621034,0.441913021789406,
0.448226064957778,0.45453910812615,0.460852151294522,0.467165194462894,
0.473478237631266,0.479791280799638,0.48610432396801,0.492417367136382,
0.498730410304754,0.505043453473126,0.511356496641498,0.51766953980987,
0.523982582978242,0.530295626146613,0.536608669314985,0.542921712483357,
0.549234755651729,0.555547798820101,0.561860841988473,0.568173885156845,
0.574486928325217,0.580799971493589,0.587113014661961,0.593426057830333,
0.599739100998705,0.606052144167077,0.612365187335449,0.618678230503821,
0.624991273672193,0.631304316840565,0.637617360008937,0.643930403177309,
0.650243446345681,0.656556489514053,0.662869532682425,0.669182575850797,
0.675495619019169,0.681808662187541,0.688121705355913,0.694434748524285,
0.700747791692657,0.707060834861029,0.713373878029401,0.719686921197773,
0.725999964366145,0.732313007534517,0.738626050702889,0.744939093871261,
0.751252137039633,0.757565180208005,0.763878223376377,0.770191266544749,
0.776504309713121,0.782817352881493,0.789130396049865,0.795443439218236,
0.801756482386608,0.80806952555498,0.814382568723352,0.820695611891724,
0.827008655060096,0.833321698228468,0.83963474139684,0.845947784565212,
0.852260827733584,0.858573870901956,0.864886914070328,0.8711999572387,0.877513000407072,
0.883826043575444,0.890139086743816,0.896452129912188,0.90276517308056,
0.909078216248932,0.915391259417304,0.921704302585676,0.928017345754048,
0.93433038892242,0.940643432090792,0.946956475259164,0.953269518427536,
0.959582561595908,0.96589560476428,0.972208647932652,0.978521691101024,
0.984834734269396,0.991147777437768,0.99746082060614,1.),.UNSPECIFIED.)
CURVE()
GEOMETRIC_REPRESENTATION_ITEM()
RATIONAL_B_SPLINE_CURVE((0.973018780871376,0.984780444152242,1.,0.866025403784439,
1.,0.866025403784439,1.,0.866025403784439,1.,0.866025403784439,1.,0.866025403784439,
1.,0.866025403784439,1.,0.866025403784439,1.,0.866025403784439,1.,0.866025403784439,
1.,0.866025403784439,1.,0.866025403784439,1.,0.866025403784439,1.,0.866025403784439,
1.,0.866025403784439,1.,0.866025403784439,1.,0.866025403784439,1.,0.866025403784439,
1.,0.866025403784439,1.,0.866025403784439,1.,0.866025403784439,1.,0.866025403784439,
1.,0.866025403784439,1.,0.866025403784439,1.,0.866025403784439,1.,0.866025403784439,
1.,0.866025403784439,1.,0.866025403784439,1.,0.866025403784439,1.,0.866025403784439,
1.,0.866025403784439,1.,0.866025403784439,1.,0.866025403784439,1.,0.866025403784439,
1.,0.866025403784439,1.,0.866025403784439,1.,0.866025403784439,1.,0.866025403784439,
1.,0.866025403784439,1.,0.866025403784439,1.,0.866025403784439,1.,0.866025403784439,
1.,0.866025403784439,1.,0.866025403784439,1.,0.866025403784439,1.,0.866025403784439,
1.,0.866025403784439,1.,0.866025403784439,1.,0.866025403784439,1.,0.866025403784439,
1.,0.866025403784439,1.,0.866025403784439,1.,0.866025403784439,1.,0.866025403784439,
1.,0.866025403784439,1.,0.866025403784439,1.,0.866025403784439,1.,0.866025403784439,
1.,0.866025403784439,1.,0.866025403784439,1.,0.866025403784439,1.,0.866025403784439,
1.,0.866025403784439,1.,0.866025403784439,1.,0.866025403784439,1.,0.866025403784439,
1.,0.866025403784439,1.,0.866025403784439,1.,0.866025403784439,1.,0.866025403784439,
1.,0.866025403784439,1.,0.866025403784439,1.,0.866025403784439,1.,0.866025403784439,
1.,0.866025403784439,1.,0.866025403784439,1.,0.866025403784439,1.,0.866025403784439,
1.,0.866025403784439,1.,0.866025403784439,1.,0.866025403784439,1.,0.866025403784439,
1.,0.866025403784439,1.,0.866025403784439,1.,0.866025403784439,1.,0.866025403784439,
1.,0.866025403784439,1.,0.866025403784439,1.,0.866025403784439,1.,0.866025403784439,
1.,0.866025403784439,1.,0.866025403784439,1.,0.866025403784439,1.,0.866025403784439,
1.,0.866025403784439,1.,0.866025403784439,1.,0.866025403784439,1.,0.866025403784439,
1.,0.866025403784439,1.,0.866025403784439,1.,0.866025403784439,1.,0.866025403784439,
1.,0.866025403784439,1.,0.866025403784439,1.,0.866025403784439,1.,0.866025403784439,
1.,0.866025403784439,1.,0.866025403784439,1.,0.866025403784439,1.,0.866025403784439,
1.,0.866025403784439,1.,0.866025403784439,1.,0.866025403784439,1.,0.866025403784439,
1.,0.866025403784439,1.,0.866025403784439,1.,0.866025403784439,1.,0.866025403784439,
1.,0.866025403784439,1.,0.866025403784439,1.,0.866025403784439,1.,0.866025403784439,
1.,0.866025403784439,1.,0.866025403784439,1.,0.866025403784439,1.,0.866025403784439,
1.,0.866025403784439,1.,0.866025403784439,1.,0.866025403784439,1.,0.866025403784439,
1.,0.866025403784439,1.,0.866025403784439,1.,0.866025403784439,1.,0.866025403784439,
1.,0.866025403784439,1.,0.866025403784439,1.,0.866025403784439,1.,0.866025403784439,
1.,0.866025403784439,1.,0.866025403784439,1.,0.866025403784439,1.,0.866025403784439,
1.,0.866025403784439,1.,0.866025403784439,1.,0.866025403784439,1.,0.866025403784439,
1.,0.866025403784439,1.,0.866025403784439,1.,0.866025403784439,1.,0.946114646713198,
0.93557529156132))
REPRESENTATION_ITEM('')
);
#271=(
BOUNDED_CURVE()
B_SPLINE_CURVE(2,(#32344,#32345,#32346,#32347,#32348,#32349,#32350,#32351,
#32352,#32353,#32354,#32355,#32356,#32357,#32358,#32359,#32360,#32361,#32362,
#32363,#32364,#32365,#32366,#32367,#32368,#32369,#32370,#32371,#32372,#32373,
#32374,#32375,#32376,#32377,#32378,#32379,#32380,#32381,#32382,#32383,#32384,
#32385,#32386,#32387,#32388,#32389,#32390,#32391,#32392,#32393,#32394,#32395,
#32396,#32397,#32398,#32399,#32400,#32401,#32402,#32403,#32404,#32405,#32406,
#32407,#32408,#32409,#32410,#32411,#32412,#32413,#32414,#32415,#32416,#32417,
#32418,#32419,#32420,#32421,#32422,#32423,#32424,#32425,#32426,#32427,#32428,
#32429,#32430,#32431,#32432,#32433,#32434,#32435,#32436,#32437,#32438,#32439,
#32440,#32441,#32442,#32443,#32444,#32445,#32446,#32447,#32448,#32449,#32450,
#32451,#32452,#32453,#32454,#32455,#32456,#32457,#32458,#32459,#32460,#32461,
#32462,#32463,#32464,#32465,#32466,#32467,#32468,#32469,#32470,#32471,#32472,
#32473,#32474,#32475,#32476,#32477,#32478,#32479,#32480,#32481,#32482,#32483,
#32484,#32485,#32486,#32487,#32488,#32489,#32490,#32491,#32492,#32493,#32494,
#32495,#32496,#32497,#32498,#32499,#32500,#32501,#32502,#32503,#32504,#32505,
#32506,#32507,#32508,#32509,#32510,#32511,#32512,#32513,#32514,#32515,#32516,
#32517,#32518,#32519,#32520,#32521,#32522,#32523,#32524,#32525,#32526,#32527,
#32528,#32529,#32530,#32531,#32532,#32533,#32534,#32535,#32536,#32537,#32538,
#32539,#32540,#32541,#32542,#32543,#32544,#32545,#32546,#32547,#32548,#32549,
#32550,#32551,#32552,#32553,#32554,#32555,#32556,#32557,#32558,#32559,#32560,
#32561,#32562,#32563,#32564,#32565,#32566,#32567,#32568,#32569,#32570,#32571,
#32572,#32573,#32574,#32575,#32576,#32577,#32578,#32579,#32580,#32581,#32582,
#32583,#32584,#32585,#32586,#32587,#32588,#32589,#32590,#32591,#32592,#32593,
#32594,#32595,#32596,#32597,#32598,#32599,#32600,#32601,#32602,#32603,#32604,
#32605,#32606,#32607,#32608,#32609,#32610,#32611,#32612,#32613,#32614,#32615,
#32616,#32617,#32618,#32619,#32620,#32621,#32622,#32623,#32624,#32625,#32626,
#32627,#32628,#32629,#32630,#32631,#32632,#32633,#32634,#32635,#32636,#32637,
#32638,#32639,#32640,#32641,#32642,#32643,#32644),.UNSPECIFIED.,.F.,.F.)
B_SPLINE_CURVE_WITH_KNOTS((3,2,2,2,2,2,2,2,2,2,2,2,2,2,2,2,2,2,2,2,2,2,
2,2,2,2,2,2,2,2,2,2,2,2,2,2,2,2,2,2,2,2,2,2,2,2,2,2,2,2,2,2,2,2,2,2,2,2,
2,2,2,2,2,2,2,2,2,2,2,2,2,2,2,2,2,2,2,2,2,2,2,2,2,2,2,2,2,2,2,2,2,2,2,2,
2,2,2,2,2,2,2,2,2,2,2,2,2,2,2,2,2,2,2,2,2,2,2,2,2,2,2,2,2,2,2,2,2,2,2,2,
2,2,2,2,2,2,2,2,2,2,2,2,2,2,2,2,2,2,2,2,3),(0.0578262804341777,0.0631304340270661,
0.0694434774297724,0.0757565208324788,0.0820695642351851,0.0883826076378915,
0.0946956510405978,0.101008694443304,0.107321737846011,0.113634781248717,
0.119947824651423,0.12626086805413,0.132573911456836,0.138886954859542,
0.145199998262249,0.151513041664955,0.157826085067661,0.164139128470368,
0.170452171873074,0.17676521527578,0.183078258678487,0.189391302081193,
0.195704345483899,0.202017388886606,0.208330432289312,0.214643475692019,
0.220956519094725,0.227269562497431,0.233582605900138,0.239895649302844,
0.24620869270555,0.252521736108257,0.258834779510963,0.265147822913669,
0.271460866316376,0.277773909719082,0.284086953121788,0.290399996524495,
0.296713039927201,0.303026083329907,0.309339126732614,0.31565217013532,
0.321965213538027,0.328278256940733,0.334591300343439,0.340904343746146,
0.347217387148852,0.353530430551558,0.359843473954265,0.366156517356971,
0.372469560759677,0.378782604162384,0.38509564756509,0.391408690967796,
0.397721734370503,0.404034777773209,0.410347821175916,0.416660864578622,
0.422973907981328,0.429286951384035,0.435599994786741,0.441913038189447,
0.448226081592154,0.45453912499486,0.460852168397566,0.467165211800273,
0.473478255202979,0.479791298605685,0.486104342008392,0.492417385411098,
0.498730428813805,0.505043472216511,0.511356515619217,0.517669559021924,
0.52398260242463,0.530295645827336,0.536608689230043,0.542921732632749,
0.549234776035455,0.555547819438162,0.561860862840868,0.568173906243574,
0.574486949646281,0.580799993048987,0.587113036451694,0.5934260798544,0.599739123257106,
0.606052166659813,0.612365210062519,0.618678253465225,0.624991296867932,
0.631304340270638,0.637617383673344,0.643930427076051,0.650243470478757,
0.656556513881463,0.66286955728417,0.669182600686876,0.675495644089583,
0.681808687492289,0.688121730894995,0.694434774297702,0.700747817700408,
0.707060861103114,0.71337390450582,0.719686947908527,0.725999991311233,
0.73231303471394,0.738626078116646,0.744939121519352,0.751252164922059,
0.757565208324765,0.763878251727471,0.770191295130178,0.776504338532884,
0.78281738193559,0.789130425338297,0.795443468741003,0.80175651214371,0.808069555546416,
0.814382598949122,0.820695642351829,0.827008685754535,0.833321729157241,
0.839634772559948,0.845947815962654,0.85226085936536,0.858573902768067,
0.864886946170773,0.871199989573479,0.877513032976186,0.883826076378892,
0.890139119781598,0.896452163184305,0.902765206587011,0.909078249989718,
0.915391293392424,0.92170433679513,0.928017380197837,0.934330423600543,
0.940643467003249,0.946956510405956,0.953269553808662,0.959582597211368,
0.965895640614075,0.972208684016781,0.978521727419487,0.984834770822194,
0.9911478142249,0.997460857627607,1.),.UNSPECIFIED.)
CURVE()
GEOMETRIC_REPRESENTATION_ITEM()
RATIONAL_B_SPLINE_CURVE((0.964022189566828,0.887435933741894,1.,0.866025403784439,
1.,0.866025403784439,1.,0.866025403784439,1.,0.866025403784439,1.,0.866025403784439,
1.,0.866025403784439,1.,0.866025403784439,1.,0.866025403784439,1.,0.866025403784439,
1.,0.866025403784439,1.,0.866025403784439,1.,0.866025403784439,1.,0.866025403784439,
1.,0.866025403784439,1.,0.866025403784439,1.,0.866025403784439,1.,0.866025403784439,
1.,0.866025403784439,1.,0.866025403784439,1.,0.866025403784439,1.,0.866025403784439,
1.,0.866025403784439,1.,0.866025403784439,1.,0.866025403784439,1.,0.866025403784439,
1.,0.866025403784439,1.,0.866025403784439,1.,0.866025403784439,1.,0.866025403784439,
1.,0.866025403784439,1.,0.866025403784439,1.,0.866025403784439,1.,0.866025403784439,
1.,0.866025403784439,1.,0.866025403784439,1.,0.866025403784439,1.,0.866025403784439,
1.,0.866025403784439,1.,0.866025403784439,1.,0.866025403784439,1.,0.866025403784439,
1.,0.866025403784439,1.,0.866025403784439,1.,0.866025403784439,1.,0.866025403784439,
1.,0.866025403784439,1.,0.866025403784439,1.,0.866025403784439,1.,0.866025403784439,
1.,0.866025403784439,1.,0.866025403784439,1.,0.866025403784439,1.,0.866025403784439,
1.,0.866025403784439,1.,0.866025403784439,1.,0.866025403784439,1.,0.866025403784439,
1.,0.866025403784439,1.,0.866025403784439,1.,0.866025403784439,1.,0.866025403784439,
1.,0.866025403784439,1.,0.866025403784439,1.,0.866025403784439,1.,0.866025403784439,
1.,0.866025403784439,1.,0.866025403784439,1.,0.866025403784439,1.,0.866025403784439,
1.,0.866025403784439,1.,0.866025403784439,1.,0.866025403784439,1.,0.866025403784439,
1.,0.866025403784439,1.,0.866025403784439,1.,0.866025403784439,1.,0.866025403784439,
1.,0.866025403784439,1.,0.866025403784439,1.,0.866025403784439,1.,0.866025403784439,
1.,0.866025403784439,1.,0.866025403784439,1.,0.866025403784439,1.,0.866025403784439,
1.,0.866025403784439,1.,0.866025403784439,1.,0.866025403784439,1.,0.866025403784439,
1.,0.866025403784439,1.,0.866025403784439,1.,0.866025403784439,1.,0.866025403784439,
1.,0.866025403784439,1.,0.866025403784439,1.,0.866025403784439,1.,0.866025403784439,
1.,0.866025403784439,1.,0.866025403784439,1.,0.866025403784439,1.,0.866025403784439,
1.,0.866025403784439,1.,0.866025403784439,1.,0.866025403784439,1.,0.866025403784439,
1.,0.866025403784439,1.,0.866025403784439,1.,0.866025403784439,1.,0.866025403784439,
1.,0.866025403784439,1.,0.866025403784439,1.,0.866025403784439,1.,0.866025403784439,
1.,0.866025403784439,1.,0.866025403784439,1.,0.866025403784439,1.,0.866025403784439,
1.,0.866025403784439,1.,0.866025403784439,1.,0.866025403784439,1.,0.866025403784439,
1.,0.866025403784439,1.,0.866025403784439,1.,0.866025403784439,1.,0.866025403784439,
1.,0.866025403784439,1.,0.866025403784439,1.,0.866025403784439,1.,0.866025403784439,
1.,0.866025403784439,1.,0.866025403784439,1.,0.866025403784439,1.,0.866025403784439,
1.,0.866025403784439,1.,0.866025403784439,1.,0.866025403784439,1.,0.866025403784439,
1.,0.866025403784439,1.,0.866025403784439,1.,0.866025403784439,1.,0.866025403784439,
1.,0.866025403784439,1.,0.866025403784439,1.,0.866025403784439,1.,0.866025403784439,
1.,0.866025403784439,1.,0.866025403784439,1.,0.866025403784439,1.,0.946114646712328,
0.93557529156098))
REPRESENTATION_ITEM('')
);
#272=(
BOUNDED_CURVE()
B_SPLINE_CURVE(2,(#33286,#33287,#33288,#33289,#33290,#33291,#33292,#33293,
#33294,#33295,#33296,#33297,#33298,#33299,#33300,#33301,#33302,#33303,#33304,
#33305,#33306,#33307,#33308,#33309,#33310,#33311,#33312,#33313,#33314,#33315,
#33316,#33317,#33318,#33319,#33320,#33321,#33322,#33323,#33324,#33325,#33326,
#33327,#33328,#33329,#33330,#33331,#33332,#33333,#33334,#33335,#33336,#33337,
#33338,#33339,#33340,#33341,#33342,#33343,#33344,#33345,#33346,#33347,#33348,
#33349,#33350,#33351,#33352,#33353,#33354,#33355,#33356,#33357,#33358,#33359,
#33360,#33361,#33362,#33363,#33364,#33365,#33366,#33367,#33368,#33369,#33370,
#33371,#33372,#33373,#33374,#33375,#33376,#33377,#33378,#33379,#33380,#33381,
#33382,#33383,#33384,#33385,#33386,#33387,#33388,#33389,#33390,#33391,#33392,
#33393,#33394,#33395,#33396,#33397,#33398,#33399,#33400,#33401,#33402,#33403,
#33404,#33405,#33406,#33407,#33408,#33409,#33410,#33411,#33412,#33413,#33414,
#33415,#33416,#33417,#33418,#33419,#33420,#33421,#33422,#33423,#33424,#33425,
#33426,#33427,#33428,#33429,#33430,#33431,#33432,#33433,#33434,#33435,#33436,
#33437,#33438,#33439,#33440,#33441,#33442,#33443,#33444,#33445,#33446,#33447,
#33448,#33449,#33450,#33451,#33452,#33453,#33454,#33455,#33456,#33457,#33458,
#33459,#33460,#33461,#33462,#33463,#33464,#33465,#33466,#33467,#33468,#33469,
#33470,#33471,#33472,#33473,#33474,#33475,#33476,#33477,#33478,#33479,#33480,
#33481,#33482,#33483,#33484,#33485,#33486,#33487,#33488,#33489,#33490,#33491,
#33492,#33493,#33494,#33495,#33496,#33497,#33498,#33499,#33500,#33501,#33502,
#33503,#33504,#33505,#33506,#33507,#33508,#33509,#33510,#33511,#33512,#33513,
#33514,#33515,#33516,#33517,#33518,#33519,#33520,#33521,#33522,#33523,#33524,
#33525,#33526,#33527,#33528,#33529,#33530,#33531,#33532,#33533,#33534,#33535,
#33536,#33537,#33538,#33539,#33540,#33541,#33542,#33543,#33544,#33545,#33546,
#33547,#33548,#33549,#33550,#33551,#33552,#33553,#33554,#33555,#33556,#33557,
#33558,#33559,#33560,#33561,#33562,#33563,#33564,#33565,#33566,#33567,#33568,
#33569,#33570,#33571,#33572,#33573,#33574,#33575,#33576,#33577,#33578,#33579,
#33580,#33581,#33582,#33583,#33584,#33585,#33586),.UNSPECIFIED.,.F.,.F.)
B_SPLINE_CURVE_WITH_KNOTS((3,2,2,2,2,2,2,2,2,2,2,2,2,2,2,2,2,2,2,2,2,2,
2,2,2,2,2,2,2,2,2,2,2,2,2,2,2,2,2,2,2,2,2,2,2,2,2,2,2,2,2,2,2,2,2,2,2,2,
2,2,2,2,2,2,2,2,2,2,2,2,2,2,2,2,2,2,2,2,2,2,2,2,2,2,2,2,2,2,2,2,2,2,2,2,
2,2,2,2,2,2,2,2,2,2,2,2,2,2,2,2,2,2,2,2,2,2,2,2,2,2,2,2,2,2,2,2,2,2,2,2,
2,2,2,2,2,2,2,2,2,2,2,2,2,2,2,2,2,2,2,2,3),(0.0624132680173737,0.0631304316872321,
0.0694434748568796,0.0757565180265271,0.0820695611961746,0.088382604365822,
0.0946956475354695,0.101008690705117,0.107321733874764,0.113634777044412,
0.119947820214059,0.126260863383707,0.132573906553354,0.138886949723002,
0.145199992892649,0.151513036062297,0.157826079231944,0.164139122401592,
0.170452165571239,0.176765208740887,0.183078251910534,0.189391295080182,
0.195704338249829,0.202017381419477,0.208330424589124,0.214643467758772,
0.220956510928419,0.227269554098067,0.233582597267714,0.239895640437362,
0.246208683607009,0.252521726776657,0.258834769946304,0.265147813115952,
0.271460856285599,0.277773899455247,0.284086942624894,0.290399985794542,
0.296713028964189,0.303026072133836,0.309339115303484,0.315652158473131,
0.321965201642779,0.328278244812426,0.334591287982074,0.340904331151721,
0.347217374321369,0.353530417491016,0.359843460660664,0.366156503830311,
0.372469546999959,0.378782590169606,0.385095633339254,0.391408676508901,
0.397721719678549,0.404034762848196,0.410347806017844,0.416660849187491,
0.422973892357139,0.429286935526786,0.435599978696434,0.441913021866081,
0.448226065035729,0.454539108205376,0.460852151375024,0.467165194544671,
0.473478237714319,0.479791280883966,0.486104324053614,0.492417367223261,
0.498730410392908,0.505043453562556,0.511356496732204,0.517669539901851,
0.523982583071499,0.530295626241146,0.536608669410793,0.542921712580441,
0.549234755750089,0.555547798919736,0.561860842089383,0.568173885259031,
0.574486928428678,0.580799971598326,0.587113014767973,0.593426057937621,
0.599739101107268,0.606052144276916,0.612365187446563,0.618678230616211,
0.624991273785858,0.631304316955506,0.637617360125153,0.643930403294801,
0.650243446464448,0.656556489634096,0.662869532803743,0.669182575973391,
0.675495619143038,0.681808662312686,0.688121705482333,0.694434748651981,
0.700747791821628,0.707060834991275,0.713373878160923,0.719686921330571,
0.725999964500218,0.732313007669865,0.738626050839513,0.74493909400916,
0.751252137178808,0.757565180348455,0.763878223518103,0.77019126668775,
0.776504309857398,0.782817353027045,0.789130396196693,0.79544343936634,
0.801756482535988,0.808069525705635,0.814382568875283,0.82069561204493,
0.827008655214578,0.833321698384225,0.839634741553873,0.84594778472352,
0.852260827893168,0.858573871062815,0.864886914232463,0.87119995740211,
0.877513000571758,0.883826043741405,0.890139086911052,0.8964521300807,0.902765173250348,
0.909078216419995,0.915391259589642,0.92170430275929,0.928017345928937,
0.934330389098585,0.940643432268232,0.94695647543788,0.953269518607527,
0.959582561777175,0.965895604946822,0.97220864811647,0.978521691286117,
0.984834734455765,0.991147777625412,0.99746082079506,1.),.UNSPECIFIED.)
CURVE()
GEOMETRIC_REPRESENTATION_ITEM()
RATIONAL_B_SPLINE_CURVE((0.973018780871376,0.984780444152243,1.,0.866025403784439,
1.,0.866025403784439,1.,0.866025403784439,1.,0.866025403784439,1.,0.866025403784439,
1.,0.866025403784439,1.,0.866025403784439,1.,0.866025403784439,1.,0.866025403784439,
1.,0.866025403784439,1.,0.866025403784439,1.,0.866025403784439,1.,0.866025403784439,
1.,0.866025403784439,1.,0.866025403784439,1.,0.866025403784439,1.,0.866025403784439,
1.,0.866025403784439,1.,0.866025403784439,1.,0.866025403784439,1.,0.866025403784439,
1.,0.866025403784439,1.,0.866025403784439,1.,0.866025403784439,1.,0.866025403784439,
1.,0.866025403784439,1.,0.866025403784439,1.,0.866025403784439,1.,0.866025403784439,
1.,0.866025403784439,1.,0.866025403784439,1.,0.866025403784439,1.,0.866025403784439,
1.,0.866025403784439,1.,0.866025403784439,1.,0.866025403784439,1.,0.866025403784439,
1.,0.866025403784439,1.,0.866025403784439,1.,0.866025403784439,1.,0.866025403784439,
1.,0.866025403784439,1.,0.866025403784439,1.,0.866025403784439,1.,0.866025403784439,
1.,0.866025403784439,1.,0.866025403784439,1.,0.866025403784439,1.,0.866025403784439,
1.,0.866025403784439,1.,0.866025403784439,1.,0.866025403784439,1.,0.866025403784439,
1.,0.866025403784439,1.,0.866025403784439,1.,0.866025403784439,1.,0.866025403784439,
1.,0.866025403784439,1.,0.866025403784439,1.,0.866025403784439,1.,0.866025403784439,
1.,0.866025403784439,1.,0.866025403784439,1.,0.866025403784439,1.,0.866025403784439,
1.,0.866025403784439,1.,0.866025403784439,1.,0.866025403784439,1.,0.866025403784439,
1.,0.866025403784439,1.,0.866025403784439,1.,0.866025403784439,1.,0.866025403784439,
1.,0.866025403784439,1.,0.866025403784439,1.,0.866025403784439,1.,0.866025403784439,
1.,0.866025403784439,1.,0.866025403784439,1.,0.866025403784439,1.,0.866025403784439,
1.,0.866025403784439,1.,0.866025403784439,1.,0.866025403784439,1.,0.866025403784439,
1.,0.866025403784439,1.,0.866025403784439,1.,0.866025403784439,1.,0.866025403784439,
1.,0.866025403784439,1.,0.866025403784439,1.,0.866025403784439,1.,0.866025403784439,
1.,0.866025403784439,1.,0.866025403784439,1.,0.866025403784439,1.,0.866025403784439,
1.,0.866025403784439,1.,0.866025403784439,1.,0.866025403784439,1.,0.866025403784439,
1.,0.866025403784439,1.,0.866025403784439,1.,0.866025403784439,1.,0.866025403784439,
1.,0.866025403784439,1.,0.866025403784439,1.,0.866025403784439,1.,0.866025403784439,
1.,0.866025403784439,1.,0.866025403784439,1.,0.866025403784439,1.,0.866025403784439,
1.,0.866025403784439,1.,0.866025403784439,1.,0.866025403784439,1.,0.866025403784439,
1.,0.866025403784439,1.,0.866025403784439,1.,0.866025403784439,1.,0.866025403784439,
1.,0.866025403784439,1.,0.866025403784439,1.,0.866025403784439,1.,0.866025403784439,
1.,0.866025403784439,1.,0.866025403784439,1.,0.866025403784439,1.,0.866025403784439,
1.,0.866025403784439,1.,0.866025403784439,1.,0.866025403784439,1.,0.866025403784439,
1.,0.866025403784439,1.,0.866025403784439,1.,0.866025403784439,1.,0.866025403784439,
1.,0.866025403784439,1.,0.866025403784439,1.,0.866025403784439,1.,0.866025403784439,
1.,0.866025403784439,1.,0.866025403784439,1.,0.866025403784439,1.,0.866025403784439,
1.,0.866025403784439,1.,0.866025403784439,1.,0.866025403784439,1.,0.946114646713198,
0.93557529156132))
REPRESENTATION_ITEM('')
);
#273=(
BOUNDED_CURVE()
B_SPLINE_CURVE(2,(#34305,#34306,#34307),.UNSPECIFIED.,.F.,.F.)
B_SPLINE_CURVE_WITH_KNOTS((3,3),(3.14998285709622,4.30410895504795),
 .UNSPECIFIED.)
CURVE()
GEOMETRIC_REPRESENTATION_ITEM()
RATIONAL_B_SPLINE_CURVE((6.34638554216859,6.34638554216859,5.62867319679424))
REPRESENTATION_ITEM('')
);
#274=(
BOUNDED_CURVE()
B_SPLINE_CURVE(2,(#34312,#34313,#34314),.UNSPECIFIED.,.F.,.F.)
B_SPLINE_CURVE_WITH_KNOTS((3,3),(1.9958567591426,3.14998285709622),
 .UNSPECIFIED.)
CURVE()
GEOMETRIC_REPRESENTATION_ITEM()
RATIONAL_B_SPLINE_CURVE((5.62867319679188,6.34638554216859,6.34638554216859))
REPRESENTATION_ITEM('')
);
#275=(
BOUNDED_CURVE()
B_SPLINE_CURVE(2,(#34670,#34671,#34672),.UNSPECIFIED.,.F.,.F.)
B_SPLINE_CURVE_WITH_KNOTS((3,3),(0.000209851267233562,0.467659076247017),
 .UNSPECIFIED.)
CURVE()
GEOMETRIC_REPRESENTATION_ITEM()
RATIONAL_B_SPLINE_CURVE((1.00013898062186,1.15486101937814,1.00013898062186))
REPRESENTATION_ITEM('')
);
#276=(
BOUNDED_CURVE()
B_SPLINE_CURVE(2,(#34675,#34676,#34677),.UNSPECIFIED.,.F.,.F.)
B_SPLINE_CURVE_WITH_KNOTS((3,3),(0.000209851267233844,0.467659076247017),
 .UNSPECIFIED.)
CURVE()
GEOMETRIC_REPRESENTATION_ITEM()
RATIONAL_B_SPLINE_CURVE((1.00013898062186,1.15486101937814,1.00013898062186))
REPRESENTATION_ITEM('')
);
#277=(
BOUNDED_CURVE()
B_SPLINE_CURVE(2,(#34680,#34681,#34682),.UNSPECIFIED.,.F.,.F.)
B_SPLINE_CURVE_WITH_KNOTS((3,3),(0.000209851267233554,0.467659076247016),
 .UNSPECIFIED.)
CURVE()
GEOMETRIC_REPRESENTATION_ITEM()
RATIONAL_B_SPLINE_CURVE((1.00013898062186,1.15486101937814,1.00013898062186))
REPRESENTATION_ITEM('')
);
#278=(
BOUNDED_CURVE()
B_SPLINE_CURVE(2,(#34685,#34686,#34687),.UNSPECIFIED.,.F.,.F.)
B_SPLINE_CURVE_WITH_KNOTS((3,3),(0.000209851267233599,0.467659076247016),
 .UNSPECIFIED.)
CURVE()
GEOMETRIC_REPRESENTATION_ITEM()
RATIONAL_B_SPLINE_CURVE((1.00013898062186,1.15486101937814,1.00013898062186))
REPRESENTATION_ITEM('')
);
#279=(
BOUNDED_CURVE()
B_SPLINE_CURVE(2,(#34691,#34692,#34693),.UNSPECIFIED.,.F.,.F.)
B_SPLINE_CURVE_WITH_KNOTS((3,3),(1.01019060757112,1.41893400293227),
 .UNSPECIFIED.)
CURVE()
GEOMETRIC_REPRESENTATION_ITEM()
RATIONAL_B_SPLINE_CURVE((1.78107349850061,1.78107349850061,1.65319817466611))
REPRESENTATION_ITEM('')
);
#280=(
BOUNDED_CURVE()
B_SPLINE_CURVE(2,(#34698,#34699,#34700),.UNSPECIFIED.,.F.,.F.)
B_SPLINE_CURVE_WITH_KNOTS((3,3),(0.601447212209968,1.01019060757112),
 .UNSPECIFIED.)
CURVE()
GEOMETRIC_REPRESENTATION_ITEM()
RATIONAL_B_SPLINE_CURVE((1.65319817466611,1.78107349850061,1.78107349850061))
REPRESENTATION_ITEM('')
);
#281=(
BOUNDED_CURVE()
B_SPLINE_CURVE(2,(#34702,#34703,#34704),.UNSPECIFIED.,.F.,.F.)
B_SPLINE_CURVE_WITH_KNOTS((3,3),(0.000209851267233684,0.467659076247016),
 .UNSPECIFIED.)
CURVE()
GEOMETRIC_REPRESENTATION_ITEM()
RATIONAL_B_SPLINE_CURVE((1.00013898062186,1.15486101937814,1.00013898062186))
REPRESENTATION_ITEM('')
);
#282=(
BOUNDED_CURVE()
B_SPLINE_CURVE(2,(#34705,#34706,#34707),.UNSPECIFIED.,.F.,.F.)
B_SPLINE_CURVE_WITH_KNOTS((3,3),(0.000209851267233646,0.467659076247016),
 .UNSPECIFIED.)
CURVE()
GEOMETRIC_REPRESENTATION_ITEM()
RATIONAL_B_SPLINE_CURVE((1.00013898062186,1.15486101937814,1.00013898062186))
REPRESENTATION_ITEM('')
);
#283=(
BOUNDED_CURVE()
B_SPLINE_CURVE(2,(#34708,#34709,#34710),.UNSPECIFIED.,.F.,.F.)
B_SPLINE_CURVE_WITH_KNOTS((3,3),(0.000209851267233851,0.467659076247016),
 .UNSPECIFIED.)
CURVE()
GEOMETRIC_REPRESENTATION_ITEM()
RATIONAL_B_SPLINE_CURVE((1.00013898062186,1.15486101937814,1.00013898062186))
REPRESENTATION_ITEM('')
);
#284=(
BOUNDED_CURVE()
B_SPLINE_CURVE(2,(#34713,#34714,#34715),.UNSPECIFIED.,.F.,.F.)
B_SPLINE_CURVE_WITH_KNOTS((3,3),(0.000209851267233802,0.467659076247016),
 .UNSPECIFIED.)
CURVE()
GEOMETRIC_REPRESENTATION_ITEM()
RATIONAL_B_SPLINE_CURVE((1.00013898062186,1.15486101937814,1.00013898062186))
REPRESENTATION_ITEM('')
);
#285=(
BOUNDED_CURVE()
B_SPLINE_CURVE(2,(#34719,#34720,#34721),.UNSPECIFIED.,.F.,.F.)
B_SPLINE_CURVE_WITH_KNOTS((3,3),(-1.50076840907249,-1.07539867696182),
 .UNSPECIFIED.)
CURVE()
GEOMETRIC_REPRESENTATION_ITEM()
RATIONAL_B_SPLINE_CURVE((1.71537600115701,1.84806079660852,1.84806079660852))
REPRESENTATION_ITEM('')
);
#286=(
BOUNDED_CURVE()
B_SPLINE_CURVE(2,(#34723,#34724,#34725),.UNSPECIFIED.,.F.,.F.)
B_SPLINE_CURVE_WITH_KNOTS((3,3),(-1.07539867696182,-0.650028944851149),
 .UNSPECIFIED.)
CURVE()
GEOMETRIC_REPRESENTATION_ITEM()
RATIONAL_B_SPLINE_CURVE((1.84806079660852,1.84806079660852,1.71537600115701))
REPRESENTATION_ITEM('')
);
#287=(
BOUNDED_CURVE()
B_SPLINE_CURVE(2,(#34729,#34730,#34731),.UNSPECIFIED.,.F.,.F.)
B_SPLINE_CURVE_WITH_KNOTS((3,3),(0.000209851267233587,0.467659076247016),
 .UNSPECIFIED.)
CURVE()
GEOMETRIC_REPRESENTATION_ITEM()
RATIONAL_B_SPLINE_CURVE((1.00013898062186,1.15486101937814,1.00013898062186))
REPRESENTATION_ITEM('')
);
#288=(
BOUNDED_CURVE()
B_SPLINE_CURVE(2,(#34734,#34735,#34736),.UNSPECIFIED.,.F.,.F.)
B_SPLINE_CURVE_WITH_KNOTS((3,3),(0.000209851267233473,0.467659076247016),
 .UNSPECIFIED.)
CURVE()
GEOMETRIC_REPRESENTATION_ITEM()
RATIONAL_B_SPLINE_CURVE((1.00013898062186,1.15486101937814,1.00013898062186))
REPRESENTATION_ITEM('')
);
#289=(
BOUNDED_SURFACE()
B_SPLINE_SURFACE(1,2,((#24102,#24103,#24104,#24105,#24106,#24107,#24108,
#24109,#24110,#24111,#24112,#24113,#24114,#24115,#24116,#24117,#24118,#24119,
#24120,#24121,#24122,#24123,#24124,#24125,#24126,#24127,#24128,#24129,#24130,
#24131,#24132,#24133,#24134,#24135,#24136,#24137,#24138,#24139,#24140,#24141,
#24142,#24143,#24144,#24145,#24146,#24147,#24148,#24149,#24150,#24151,#24152,
#24153,#24154,#24155,#24156,#24157,#24158,#24159,#24160,#24161,#24162,#24163,
#24164,#24165,#24166,#24167,#24168,#24169,#24170,#24171,#24172,#24173,#24174,
#24175,#24176,#24177,#24178,#24179,#24180,#24181,#24182,#24183,#24184,#24185,
#24186,#24187,#24188,#24189,#24190,#24191,#24192,#24193,#24194,#24195,#24196,
#24197,#24198,#24199,#24200,#24201,#24202,#24203,#24204,#24205,#24206,#24207,
#24208,#24209,#24210,#24211,#24212,#24213,#24214,#24215,#24216,#24217,#24218,
#24219,#24220,#24221,#24222,#24223,#24224,#24225,#24226,#24227,#24228,#24229,
#24230,#24231,#24232,#24233,#24234,#24235,#24236,#24237,#24238,#24239,#24240,
#24241,#24242,#24243,#24244,#24245,#24246,#24247,#24248,#24249,#24250,#24251,
#24252,#24253,#24254,#24255,#24256,#24257,#24258,#24259,#24260,#24261,#24262,
#24263,#24264,#24265,#24266,#24267,#24268,#24269,#24270,#24271,#24272,#24273,
#24274,#24275,#24276,#24277,#24278,#24279,#24280,#24281,#24282,#24283,#24284,
#24285,#24286,#24287,#24288,#24289,#24290,#24291,#24292,#24293,#24294,#24295,
#24296,#24297,#24298,#24299,#24300,#24301,#24302,#24303,#24304,#24305,#24306,
#24307,#24308,#24309,#24310,#24311,#24312,#24313,#24314,#24315,#24316,#24317,
#24318,#24319,#24320,#24321,#24322,#24323,#24324,#24325,#24326,#24327,#24328,
#24329,#24330,#24331,#24332,#24333,#24334,#24335,#24336,#24337,#24338,#24339,
#24340,#24341,#24342,#24343,#24344,#24345,#24346,#24347,#24348,#24349,#24350,
#24351,#24352,#24353,#24354,#24355,#24356,#24357,#24358,#24359,#24360,#24361,
#24362,#24363,#24364,#24365,#24366,#24367,#24368,#24369,#24370,#24371,#24372,
#24373,#24374,#24375,#24376,#24377,#24378,#24379,#24380,#24381,#24382,#24383,
#24384,#24385,#24386,#24387,#24388,#24389,#24390,#24391,#24392,#24393,#24394,
#24395,#24396,#24397,#24398,#24399,#24400,#24401,#24402,#24403,#24404,#24405,
#24406,#24407,#24408,#24409,#24410,#24411,#24412,#24413,#24414,#24415,#24416,
#24417,#24418,#24419,#24420),(#24421,#24422,#24423,#24424,#24425,#24426,
#24427,#24428,#24429,#24430,#24431,#24432,#24433,#24434,#24435,#24436,#24437,
#24438,#24439,#24440,#24441,#24442,#24443,#24444,#24445,#24446,#24447,#24448,
#24449,#24450,#24451,#24452,#24453,#24454,#24455,#24456,#24457,#24458,#24459,
#24460,#24461,#24462,#24463,#24464,#24465,#24466,#24467,#24468,#24469,#24470,
#24471,#24472,#24473,#24474,#24475,#24476,#24477,#24478,#24479,#24480,#24481,
#24482,#24483,#24484,#24485,#24486,#24487,#24488,#24489,#24490,#24491,#24492,
#24493,#24494,#24495,#24496,#24497,#24498,#24499,#24500,#24501,#24502,#24503,
#24504,#24505,#24506,#24507,#24508,#24509,#24510,#24511,#24512,#24513,#24514,
#24515,#24516,#24517,#24518,#24519,#24520,#24521,#24522,#24523,#24524,#24525,
#24526,#24527,#24528,#24529,#24530,#24531,#24532,#24533,#24534,#24535,#24536,
#24537,#24538,#24539,#24540,#24541,#24542,#24543,#24544,#24545,#24546,#24547,
#24548,#24549,#24550,#24551,#24552,#24553,#24554,#24555,#24556,#24557,#24558,
#24559,#24560,#24561,#24562,#24563,#24564,#24565,#24566,#24567,#24568,#24569,
#24570,#24571,#24572,#24573,#24574,#24575,#24576,#24577,#24578,#24579,#24580,
#24581,#24582,#24583,#24584,#24585,#24586,#24587,#24588,#24589,#24590,#24591,
#24592,#24593,#24594,#24595,#24596,#24597,#24598,#24599,#24600,#24601,#24602,
#24603,#24604,#24605,#24606,#24607,#24608,#24609,#24610,#24611,#24612,#24613,
#24614,#24615,#24616,#24617,#24618,#24619,#24620,#24621,#24622,#24623,#24624,
#24625,#24626,#24627,#24628,#24629,#24630,#24631,#24632,#24633,#24634,#24635,
#24636,#24637,#24638,#24639,#24640,#24641,#24642,#24643,#24644,#24645,#24646,
#24647,#24648,#24649,#24650,#24651,#24652,#24653,#24654,#24655,#24656,#24657,
#24658,#24659,#24660,#24661,#24662,#24663,#24664,#24665,#24666,#24667,#24668,
#24669,#24670,#24671,#24672,#24673,#24674,#24675,#24676,#24677,#24678,#24679,
#24680,#24681,#24682,#24683,#24684,#24685,#24686,#24687,#24688,#24689,#24690,
#24691,#24692,#24693,#24694,#24695,#24696,#24697,#24698,#24699,#24700,#24701,
#24702,#24703,#24704,#24705,#24706,#24707,#24708,#24709,#24710,#24711,#24712,
#24713,#24714,#24715,#24716,#24717,#24718,#24719,#24720,#24721,#24722,#24723,
#24724,#24725,#24726,#24727,#24728,#24729,#24730,#24731,#24732,#24733,#24734,
#24735,#24736,#24737,#24738,#24739)),.UNSPECIFIED.,.F.,.F.,.F.)
B_SPLINE_SURFACE_WITH_KNOTS((2,2),(3,2,2,2,2,2,2,2,2,2,2,2,2,2,2,2,2,2,
2,2,2,2,2,2,2,2,2,2,2,2,2,2,2,2,2,2,2,2,2,2,2,2,2,2,2,2,2,2,2,2,2,2,2,2,
2,2,2,2,2,2,2,2,2,2,2,2,2,2,2,2,2,2,2,2,2,2,2,2,2,2,2,2,2,2,2,2,2,2,2,2,
2,2,2,2,2,2,2,2,2,2,2,2,2,2,2,2,2,2,2,2,2,2,2,2,2,2,2,2,2,2,2,2,2,2,2,2,
2,2,2,2,2,2,2,2,2,2,2,2,2,2,2,2,2,2,2,2,2,2,2,2,2,2,2,2,2,2,2,2,2,3),(-2.4733869132694E-5,
1.),(0.,0.00617283950617284,0.0123456790123457,0.0185185185185185,0.0246913580246914,
0.0308641975308642,0.037037037037037,0.0432098765432099,0.0493827160493827,
0.0555555555555556,0.0617283950617284,0.0679012345679012,0.0740740740740741,
0.0802469135802469,0.0864197530864197,0.0925925925925926,0.0987654320987654,
0.104938271604938,0.111111111111111,0.117283950617284,0.123456790123457,
0.12962962962963,0.135802469135802,0.141975308641975,0.148148148148148,
0.154320987654321,0.160493827160494,0.166666666666667,0.172839506172839,
0.179012345679012,0.185185185185185,0.191358024691358,0.197530864197531,
0.203703703703704,0.209876543209877,0.216049382716049,0.222222222222222,
0.228395061728395,0.234567901234568,0.240740740740741,0.246913580246914,
0.253086419753086,0.259259259259259,0.265432098765432,0.271604938271605,
0.277777777777778,0.283950617283951,0.290123456790123,0.296296296296296,
0.302469135802469,0.308641975308642,0.314814814814815,0.320987654320988,
0.327160493827161,0.333333333333333,0.339506172839506,0.345679012345679,
0.351851851851852,0.358024691358025,0.364197530864198,0.37037037037037,
0.376543209876543,0.382716049382716,0.388888888888889,0.395061728395062,
0.401234567901235,0.407407407407407,0.41358024691358,0.419753086419753,
0.425925925925926,0.432098765432099,0.438271604938272,0.444444444444444,
0.450617283950617,0.45679012345679,0.462962962962963,0.469135802469136,
0.475308641975309,0.481481481481481,0.487654320987654,0.493827160493827,
0.5,0.506172839506173,0.512345679012346,0.518518518518518,0.524691358024691,
0.530864197530864,0.537037037037037,0.54320987654321,0.549382716049383,
0.555555555555556,0.561728395061728,0.567901234567901,0.574074074074074,
0.580246913580247,0.58641975308642,0.592592592592593,0.598765432098765,
0.604938271604938,0.611111111111111,0.617283950617284,0.623456790123457,
0.62962962962963,0.635802469135803,0.641975308641975,0.648148148148148,
0.654320987654321,0.660493827160494,0.666666666666667,0.672839506172839,
0.679012345679012,0.685185185185185,0.691358024691358,0.697530864197531,
0.703703703703704,0.709876543209877,0.716049382716049,0.722222222222222,
0.728395061728395,0.734567901234568,0.740740740740741,0.746913580246914,
0.753086419753086,0.759259259259259,0.765432098765432,0.771604938271605,
0.777777777777778,0.783950617283951,0.790123456790123,0.796296296296296,
0.802469135802469,0.808641975308642,0.814814814814815,0.820987654320988,
0.827160493827161,0.833333333333333,0.839506172839506,0.845679012345679,
0.851851851851852,0.858024691358025,0.864197530864197,0.87037037037037,
0.876543209876543,0.882716049382716,0.888888888888889,0.895061728395062,
0.901234567901235,0.907407407407407,0.91358024691358,0.919753086419753,
0.925925925925926,0.932098765432099,0.938271604938272,0.944444444444444,
0.950617283950617,0.95679012345679,0.962962962962963,0.969135802469136,
0.975308641975309,0.977791447664447),.UNSPECIFIED.)
GEOMETRIC_REPRESENTATION_ITEM()
RATIONAL_B_SPLINE_SURFACE(((1.,0.866025403784439,1.,0.866025403784439,1.,
0.866025403784439,1.,0.866025403784439,1.,0.866025403784439,1.,0.866025403784439,
1.,0.866025403784439,1.,0.866025403784439,1.,0.866025403784439,1.,0.866025403784439,
1.,0.866025403784439,1.,0.866025403784439,1.,0.866025403784439,1.,0.866025403784439,
1.,0.866025403784439,1.,0.866025403784439,1.,0.866025403784439,1.,0.866025403784439,
1.,0.866025403784439,1.,0.866025403784439,1.,0.866025403784439,1.,0.866025403784439,
1.,0.866025403784439,1.,0.866025403784439,1.,0.866025403784439,1.,0.866025403784439,
1.,0.866025403784439,1.,0.866025403784439,1.,0.866025403784439,1.,0.866025403784439,
1.,0.866025403784439,1.,0.866025403784439,1.,0.866025403784439,1.,0.866025403784439,
1.,0.866025403784439,1.,0.866025403784439,1.,0.866025403784439,1.,0.866025403784439,
1.,0.866025403784439,1.,0.866025403784439,1.,0.866025403784439,1.,0.866025403784439,
1.,0.866025403784439,1.,0.866025403784439,1.,0.866025403784439,1.,0.866025403784439,
1.,0.866025403784439,1.,0.866025403784439,1.,0.866025403784439,1.,0.866025403784439,
1.,0.866025403784439,1.,0.866025403784439,1.,0.866025403784439,1.,0.866025403784439,
1.,0.866025403784439,1.,0.866025403784439,1.,0.866025403784439,1.,0.866025403784439,
1.,0.866025403784439,1.,0.866025403784439,1.,0.866025403784439,1.,0.866025403784439,
1.,0.866025403784439,1.,0.866025403784439,1.,0.866025403784439,1.,0.866025403784439,
1.,0.866025403784439,1.,0.866025403784439,1.,0.866025403784439,1.,0.866025403784439,
1.,0.866025403784439,1.,0.866025403784439,1.,0.866025403784439,1.,0.866025403784439,
1.,0.866025403784439,1.,0.866025403784439,1.,0.866025403784439,1.,0.866025403784439,
1.,0.866025403784439,1.,0.866025403784439,1.,0.866025403784439,1.,0.866025403784439,
1.,0.866025403784439,1.,0.866025403784439,1.,0.866025403784439,1.,0.866025403784439,
1.,0.866025403784439,1.,0.866025403784439,1.,0.866025403784439,1.,0.866025403784439,
1.,0.866025403784439,1.,0.866025403784439,1.,0.866025403784439,1.,0.866025403784439,
1.,0.866025403784439,1.,0.866025403784439,1.,0.866025403784439,1.,0.866025403784439,
1.,0.866025403784439,1.,0.866025403784439,1.,0.866025403784439,1.,0.866025403784439,
1.,0.866025403784439,1.,0.866025403784439,1.,0.866025403784439,1.,0.866025403784439,
1.,0.866025403784439,1.,0.866025403784439,1.,0.866025403784439,1.,0.866025403784439,
1.,0.866025403784439,1.,0.866025403784439,1.,0.866025403784439,1.,0.866025403784439,
1.,0.866025403784439,1.,0.866025403784439,1.,0.866025403784439,1.,0.866025403784439,
1.,0.866025403784439,1.,0.866025403784439,1.,0.866025403784439,1.,0.866025403784439,
1.,0.866025403784439,1.,0.866025403784439,1.,0.866025403784439,1.,0.866025403784439,
1.,0.866025403784439,1.,0.866025403784439,1.,0.866025403784439,1.,0.866025403784439,
1.,0.866025403784439,1.,0.866025403784439,1.,0.866025403784439,1.,0.866025403784439,
1.,0.866025403784439,1.,0.866025403784439,1.,0.866025403784439,1.,0.866025403784439,
1.,0.866025403784439,1.,0.866025403784439,1.,0.866025403784439,1.,0.866025403784439,
1.,0.866025403784439,1.,0.866025403784439,1.,0.866025403784439,1.,0.866025403784439,
1.,0.866025403784439,1.,0.866025403784439,1.,0.866025403784439,1.,0.866025403784439,
1.,0.866025403784439,1.,0.866025403784439,1.,0.866025403784439,1.,0.866025403784439,
1.,0.866025403784439,1.,0.866025403784439,1.,0.866025403784439,1.,0.866025403784439,
1.,0.9461134718712,0.935574832010768),(1.,0.866025403784439,1.,0.866025403784439,
1.,0.866025403784439,1.,0.866025403784439,1.,0.866025403784439,1.,0.866025403784439,
1.,0.866025403784439,1.,0.866025403784439,1.,0.866025403784439,1.,0.866025403784439,
1.,0.866025403784439,1.,0.866025403784439,1.,0.866025403784439,1.,0.866025403784439,
1.,0.866025403784439,1.,0.866025403784439,1.,0.866025403784439,1.,0.866025403784439,
1.,0.866025403784439,1.,0.866025403784439,1.,0.866025403784439,1.,0.866025403784439,
1.,0.866025403784439,1.,0.866025403784439,1.,0.866025403784439,1.,0.866025403784439,
1.,0.866025403784439,1.,0.866025403784439,1.,0.866025403784439,1.,0.866025403784439,
1.,0.866025403784439,1.,0.866025403784439,1.,0.866025403784439,1.,0.866025403784439,
1.,0.866025403784439,1.,0.866025403784439,1.,0.866025403784439,1.,0.866025403784439,
1.,0.866025403784439,1.,0.866025403784439,1.,0.866025403784439,1.,0.866025403784439,
1.,0.866025403784439,1.,0.866025403784439,1.,0.866025403784439,1.,0.866025403784439,
1.,0.866025403784439,1.,0.866025403784439,1.,0.866025403784439,1.,0.866025403784439,
1.,0.866025403784439,1.,0.866025403784439,1.,0.866025403784439,1.,0.866025403784439,
1.,0.866025403784439,1.,0.866025403784439,1.,0.866025403784439,1.,0.866025403784439,
1.,0.866025403784439,1.,0.866025403784439,1.,0.866025403784439,1.,0.866025403784439,
1.,0.866025403784439,1.,0.866025403784439,1.,0.866025403784439,1.,0.866025403784439,
1.,0.866025403784439,1.,0.866025403784439,1.,0.866025403784439,1.,0.866025403784439,
1.,0.866025403784439,1.,0.866025403784439,1.,0.866025403784439,1.,0.866025403784439,
1.,0.866025403784439,1.,0.866025403784439,1.,0.866025403784439,1.,0.866025403784439,
1.,0.866025403784439,1.,0.866025403784439,1.,0.866025403784439,1.,0.866025403784439,
1.,0.866025403784439,1.,0.866025403784439,1.,0.866025403784439,1.,0.866025403784439,
1.,0.866025403784439,1.,0.866025403784439,1.,0.866025403784439,1.,0.866025403784439,
1.,0.866025403784439,1.,0.866025403784439,1.,0.866025403784439,1.,0.866025403784439,
1.,0.866025403784439,1.,0.866025403784439,1.,0.866025403784439,1.,0.866025403784439,
1.,0.866025403784439,1.,0.866025403784439,1.,0.866025403784439,1.,0.866025403784439,
1.,0.866025403784439,1.,0.866025403784439,1.,0.866025403784439,1.,0.866025403784439,
1.,0.866025403784439,1.,0.866025403784439,1.,0.866025403784439,1.,0.866025403784439,
1.,0.866025403784439,1.,0.866025403784439,1.,0.866025403784439,1.,0.866025403784439,
1.,0.866025403784439,1.,0.866025403784439,1.,0.866025403784439,1.,0.866025403784439,
1.,0.866025403784439,1.,0.866025403784439,1.,0.866025403784439,1.,0.866025403784439,
1.,0.866025403784439,1.,0.866025403784439,1.,0.866025403784439,1.,0.866025403784439,
1.,0.866025403784439,1.,0.866025403784439,1.,0.866025403784439,1.,0.866025403784439,
1.,0.866025403784439,1.,0.866025403784439,1.,0.866025403784439,1.,0.866025403784439,
1.,0.866025403784439,1.,0.866025403784439,1.,0.866025403784439,1.,0.866025403784439,
1.,0.866025403784439,1.,0.866025403784439,1.,0.866025403784439,1.,0.866025403784439,
1.,0.866025403784439,1.,0.866025403784439,1.,0.866025403784439,1.,0.866025403784439,
1.,0.866025403784439,1.,0.866025403784439,1.,0.866025403784439,1.,0.866025403784439,
1.,0.866025403784439,1.,0.866025403784439,1.,0.866025403784439,1.,0.866025403784439,
1.,0.866025403784439,1.,0.866025403784439,1.,0.866025403784439,1.,0.866025403784439,
1.,0.9461134718712,0.935574832010768)))
REPRESENTATION_ITEM('')
SURFACE()
);
#290=(
BOUNDED_SURFACE()
B_SPLINE_SURFACE(1,2,((#25044,#25045,#25046,#25047,#25048,#25049,#25050,
#25051,#25052,#25053,#25054,#25055,#25056,#25057,#25058,#25059,#25060,#25061,
#25062,#25063,#25064,#25065,#25066,#25067,#25068,#25069,#25070,#25071,#25072,
#25073,#25074,#25075,#25076,#25077,#25078,#25079,#25080,#25081,#25082,#25083,
#25084,#25085,#25086,#25087,#25088,#25089,#25090,#25091,#25092,#25093,#25094,
#25095,#25096,#25097,#25098,#25099,#25100,#25101,#25102,#25103,#25104,#25105,
#25106,#25107,#25108,#25109,#25110,#25111,#25112,#25113,#25114,#25115,#25116,
#25117,#25118,#25119,#25120,#25121,#25122,#25123,#25124,#25125,#25126,#25127,
#25128,#25129,#25130,#25131,#25132,#25133,#25134,#25135,#25136,#25137,#25138,
#25139,#25140,#25141,#25142,#25143,#25144,#25145,#25146,#25147,#25148,#25149,
#25150,#25151,#25152,#25153,#25154,#25155,#25156,#25157,#25158,#25159,#25160,
#25161,#25162,#25163,#25164,#25165,#25166,#25167,#25168,#25169,#25170,#25171,
#25172,#25173,#25174,#25175,#25176,#25177,#25178,#25179,#25180,#25181,#25182,
#25183,#25184,#25185,#25186,#25187,#25188,#25189,#25190,#25191,#25192,#25193,
#25194,#25195,#25196,#25197,#25198,#25199,#25200,#25201,#25202,#25203,#25204,
#25205,#25206,#25207,#25208,#25209,#25210,#25211,#25212,#25213,#25214,#25215,
#25216,#25217,#25218,#25219,#25220,#25221,#25222,#25223,#25224,#25225,#25226,
#25227,#25228,#25229,#25230,#25231,#25232,#25233,#25234,#25235,#25236,#25237,
#25238,#25239,#25240,#25241,#25242,#25243,#25244,#25245,#25246,#25247,#25248,
#25249,#25250,#25251,#25252,#25253,#25254,#25255,#25256,#25257,#25258,#25259,
#25260,#25261,#25262,#25263,#25264,#25265,#25266,#25267,#25268,#25269,#25270,
#25271,#25272,#25273,#25274,#25275,#25276,#25277,#25278,#25279,#25280,#25281,
#25282,#25283,#25284,#25285,#25286,#25287,#25288,#25289,#25290,#25291,#25292,
#25293,#25294,#25295,#25296,#25297,#25298,#25299,#25300,#25301,#25302,#25303,
#25304,#25305,#25306,#25307,#25308,#25309,#25310,#25311,#25312,#25313,#25314,
#25315,#25316,#25317,#25318,#25319,#25320,#25321,#25322,#25323,#25324,#25325,
#25326,#25327,#25328,#25329,#25330,#25331,#25332,#25333,#25334,#25335,#25336,
#25337,#25338,#25339,#25340,#25341,#25342,#25343,#25344,#25345,#25346,#25347,
#25348,#25349,#25350,#25351,#25352,#25353,#25354,#25355,#25356,#25357,#25358,
#25359,#25360,#25361,#25362),(#25363,#25364,#25365,#25366,#25367,#25368,
#25369,#25370,#25371,#25372,#25373,#25374,#25375,#25376,#25377,#25378,#25379,
#25380,#25381,#25382,#25383,#25384,#25385,#25386,#25387,#25388,#25389,#25390,
#25391,#25392,#25393,#25394,#25395,#25396,#25397,#25398,#25399,#25400,#25401,
#25402,#25403,#25404,#25405,#25406,#25407,#25408,#25409,#25410,#25411,#25412,
#25413,#25414,#25415,#25416,#25417,#25418,#25419,#25420,#25421,#25422,#25423,
#25424,#25425,#25426,#25427,#25428,#25429,#25430,#25431,#25432,#25433,#25434,
#25435,#25436,#25437,#25438,#25439,#25440,#25441,#25442,#25443,#25444,#25445,
#25446,#25447,#25448,#25449,#25450,#25451,#25452,#25453,#25454,#25455,#25456,
#25457,#25458,#25459,#25460,#25461,#25462,#25463,#25464,#25465,#25466,#25467,
#25468,#25469,#25470,#25471,#25472,#25473,#25474,#25475,#25476,#25477,#25478,
#25479,#25480,#25481,#25482,#25483,#25484,#25485,#25486,#25487,#25488,#25489,
#25490,#25491,#25492,#25493,#25494,#25495,#25496,#25497,#25498,#25499,#25500,
#25501,#25502,#25503,#25504,#25505,#25506,#25507,#25508,#25509,#25510,#25511,
#25512,#25513,#25514,#25515,#25516,#25517,#25518,#25519,#25520,#25521,#25522,
#25523,#25524,#25525,#25526,#25527,#25528,#25529,#25530,#25531,#25532,#25533,
#25534,#25535,#25536,#25537,#25538,#25539,#25540,#25541,#25542,#25543,#25544,
#25545,#25546,#25547,#25548,#25549,#25550,#25551,#25552,#25553,#25554,#25555,
#25556,#25557,#25558,#25559,#25560,#25561,#25562,#25563,#25564,#25565,#25566,
#25567,#25568,#25569,#25570,#25571,#25572,#25573,#25574,#25575,#25576,#25577,
#25578,#25579,#25580,#25581,#25582,#25583,#25584,#25585,#25586,#25587,#25588,
#25589,#25590,#25591,#25592,#25593,#25594,#25595,#25596,#25597,#25598,#25599,
#25600,#25601,#25602,#25603,#25604,#25605,#25606,#25607,#25608,#25609,#25610,
#25611,#25612,#25613,#25614,#25615,#25616,#25617,#25618,#25619,#25620,#25621,
#25622,#25623,#25624,#25625,#25626,#25627,#25628,#25629,#25630,#25631,#25632,
#25633,#25634,#25635,#25636,#25637,#25638,#25639,#25640,#25641,#25642,#25643,
#25644,#25645,#25646,#25647,#25648,#25649,#25650,#25651,#25652,#25653,#25654,
#25655,#25656,#25657,#25658,#25659,#25660,#25661,#25662,#25663,#25664,#25665,
#25666,#25667,#25668,#25669,#25670,#25671,#25672,#25673,#25674,#25675,#25676,
#25677,#25678,#25679,#25680,#25681)),.UNSPECIFIED.,.F.,.F.,.F.)
B_SPLINE_SURFACE_WITH_KNOTS((2,2),(3,2,2,2,2,2,2,2,2,2,2,2,2,2,2,2,2,2,
2,2,2,2,2,2,2,2,2,2,2,2,2,2,2,2,2,2,2,2,2,2,2,2,2,2,2,2,2,2,2,2,2,2,2,2,
2,2,2,2,2,2,2,2,2,2,2,2,2,2,2,2,2,2,2,2,2,2,2,2,2,2,2,2,2,2,2,2,2,2,2,2,
2,2,2,2,2,2,2,2,2,2,2,2,2,2,2,2,2,2,2,2,2,2,2,2,2,2,2,2,2,2,2,2,2,2,2,2,
2,2,2,2,2,2,2,2,2,2,2,2,2,2,2,2,2,2,2,2,2,2,2,2,2,2,2,2,2,2,2,2,2,3),(0.,
1.),(0.,0.00617283950617284,0.0123456790123457,0.0185185185185185,0.0246913580246914,
0.0308641975308642,0.037037037037037,0.0432098765432099,0.0493827160493827,
0.0555555555555556,0.0617283950617284,0.0679012345679012,0.0740740740740741,
0.0802469135802469,0.0864197530864197,0.0925925925925926,0.0987654320987654,
0.104938271604938,0.111111111111111,0.117283950617284,0.123456790123457,
0.12962962962963,0.135802469135802,0.141975308641975,0.148148148148148,
0.154320987654321,0.160493827160494,0.166666666666667,0.172839506172839,
0.179012345679012,0.185185185185185,0.191358024691358,0.197530864197531,
0.203703703703704,0.209876543209877,0.216049382716049,0.222222222222222,
0.228395061728395,0.234567901234568,0.240740740740741,0.246913580246914,
0.253086419753086,0.259259259259259,0.265432098765432,0.271604938271605,
0.277777777777778,0.283950617283951,0.290123456790123,0.296296296296296,
0.302469135802469,0.308641975308642,0.314814814814815,0.320987654320988,
0.327160493827161,0.333333333333333,0.339506172839506,0.345679012345679,
0.351851851851852,0.358024691358025,0.364197530864198,0.37037037037037,
0.376543209876543,0.382716049382716,0.388888888888889,0.395061728395062,
0.401234567901235,0.407407407407407,0.41358024691358,0.419753086419753,
0.425925925925926,0.432098765432099,0.438271604938272,0.444444444444444,
0.450617283950617,0.45679012345679,0.462962962962963,0.469135802469136,
0.475308641975309,0.481481481481481,0.487654320987654,0.493827160493827,
0.5,0.506172839506173,0.512345679012346,0.518518518518518,0.524691358024691,
0.530864197530864,0.537037037037037,0.54320987654321,0.549382716049383,
0.555555555555556,0.561728395061728,0.567901234567901,0.574074074074074,
0.580246913580247,0.58641975308642,0.592592592592593,0.598765432098765,
0.604938271604938,0.611111111111111,0.617283950617284,0.623456790123457,
0.62962962962963,0.635802469135803,0.641975308641975,0.648148148148148,
0.654320987654321,0.660493827160494,0.666666666666667,0.672839506172839,
0.679012345679012,0.685185185185185,0.691358024691358,0.697530864197531,
0.703703703703704,0.709876543209877,0.716049382716049,0.722222222222222,
0.728395061728395,0.734567901234568,0.740740740740741,0.746913580246914,
0.753086419753086,0.759259259259259,0.765432098765432,0.771604938271605,
0.777777777777778,0.783950617283951,0.790123456790123,0.796296296296296,
0.802469135802469,0.808641975308642,0.814814814814815,0.820987654320988,
0.827160493827161,0.833333333333333,0.839506172839506,0.845679012345679,
0.851851851851852,0.858024691358025,0.864197530864197,0.87037037037037,
0.876543209876543,0.882716049382716,0.888888888888889,0.895061728395062,
0.901234567901235,0.907407407407407,0.91358024691358,0.919753086419753,
0.925925925925926,0.932098765432099,0.938271604938272,0.944444444444444,
0.950617283950617,0.95679012345679,0.962962962962963,0.969135802469136,
0.975308641975309,0.977791440774828),.UNSPECIFIED.)
GEOMETRIC_REPRESENTATION_ITEM()
RATIONAL_B_SPLINE_SURFACE(((1.,0.866025403784439,1.,0.866025403784439,1.,
0.866025403784439,1.,0.866025403784439,1.,0.866025403784439,1.,0.866025403784439,
1.,0.866025403784439,1.,0.866025403784439,1.,0.866025403784439,1.,0.866025403784439,
1.,0.866025403784439,1.,0.866025403784439,1.,0.866025403784439,1.,0.866025403784439,
1.,0.866025403784439,1.,0.866025403784439,1.,0.866025403784439,1.,0.866025403784439,
1.,0.866025403784439,1.,0.866025403784439,1.,0.866025403784439,1.,0.866025403784439,
1.,0.866025403784439,1.,0.866025403784439,1.,0.866025403784439,1.,0.866025403784439,
1.,0.866025403784439,1.,0.866025403784439,1.,0.866025403784439,1.,0.866025403784439,
1.,0.866025403784439,1.,0.866025403784439,1.,0.866025403784439,1.,0.866025403784439,
1.,0.866025403784439,1.,0.866025403784439,1.,0.866025403784439,1.,0.866025403784439,
1.,0.866025403784439,1.,0.866025403784439,1.,0.866025403784439,1.,0.866025403784439,
1.,0.866025403784439,1.,0.866025403784439,1.,0.866025403784439,1.,0.866025403784439,
1.,0.866025403784439,1.,0.866025403784439,1.,0.866025403784439,1.,0.866025403784439,
1.,0.866025403784439,1.,0.866025403784439,1.,0.866025403784439,1.,0.866025403784439,
1.,0.866025403784439,1.,0.866025403784439,1.,0.866025403784439,1.,0.866025403784439,
1.,0.866025403784439,1.,0.866025403784439,1.,0.866025403784439,1.,0.866025403784439,
1.,0.866025403784439,1.,0.866025403784439,1.,0.866025403784439,1.,0.866025403784439,
1.,0.866025403784439,1.,0.866025403784439,1.,0.866025403784439,1.,0.866025403784439,
1.,0.866025403784439,1.,0.866025403784439,1.,0.866025403784439,1.,0.866025403784439,
1.,0.866025403784439,1.,0.866025403784439,1.,0.866025403784439,1.,0.866025403784439,
1.,0.866025403784439,1.,0.866025403784439,1.,0.866025403784439,1.,0.866025403784439,
1.,0.866025403784439,1.,0.866025403784439,1.,0.866025403784439,1.,0.866025403784439,
1.,0.866025403784439,1.,0.866025403784439,1.,0.866025403784439,1.,0.866025403784439,
1.,0.866025403784439,1.,0.866025403784439,1.,0.866025403784439,1.,0.866025403784439,
1.,0.866025403784439,1.,0.866025403784439,1.,0.866025403784439,1.,0.866025403784439,
1.,0.866025403784439,1.,0.866025403784439,1.,0.866025403784439,1.,0.866025403784439,
1.,0.866025403784439,1.,0.866025403784439,1.,0.866025403784439,1.,0.866025403784439,
1.,0.866025403784439,1.,0.866025403784439,1.,0.866025403784439,1.,0.866025403784439,
1.,0.866025403784439,1.,0.866025403784439,1.,0.866025403784439,1.,0.866025403784439,
1.,0.866025403784439,1.,0.866025403784439,1.,0.866025403784439,1.,0.866025403784439,
1.,0.866025403784439,1.,0.866025403784439,1.,0.866025403784439,1.,0.866025403784439,
1.,0.866025403784439,1.,0.866025403784439,1.,0.866025403784439,1.,0.866025403784439,
1.,0.866025403784439,1.,0.866025403784439,1.,0.866025403784439,1.,0.866025403784439,
1.,0.866025403784439,1.,0.866025403784439,1.,0.866025403784439,1.,0.866025403784439,
1.,0.866025403784439,1.,0.866025403784439,1.,0.866025403784439,1.,0.866025403784439,
1.,0.866025403784439,1.,0.866025403784439,1.,0.866025403784439,1.,0.866025403784439,
1.,0.866025403784439,1.,0.866025403784439,1.,0.866025403784439,1.,0.866025403784439,
1.,0.866025403784439,1.,0.866025403784439,1.,0.866025403784439,1.,0.866025403784439,
1.,0.866025403784439,1.,0.866025403784439,1.,0.866025403784439,1.,0.866025403784439,
1.,0.866025403784439,1.,0.866025403784439,1.,0.866025403784439,1.,0.866025403784439,
1.,0.946113621402695,0.935574890499137),(1.,0.866025403784439,1.,0.866025403784439,
1.,0.866025403784439,1.,0.866025403784439,1.,0.866025403784439,1.,0.866025403784439,
1.,0.866025403784439,1.,0.866025403784439,1.,0.866025403784439,1.,0.866025403784439,
1.,0.866025403784439,1.,0.866025403784439,1.,0.866025403784439,1.,0.866025403784439,
1.,0.866025403784439,1.,0.866025403784439,1.,0.866025403784439,1.,0.866025403784439,
1.,0.866025403784439,1.,0.866025403784439,1.,0.866025403784439,1.,0.866025403784439,
1.,0.866025403784439,1.,0.866025403784439,1.,0.866025403784439,1.,0.866025403784439,
1.,0.866025403784439,1.,0.866025403784439,1.,0.866025403784439,1.,0.866025403784439,
1.,0.866025403784439,1.,0.866025403784439,1.,0.866025403784439,1.,0.866025403784439,
1.,0.866025403784439,1.,0.866025403784439,1.,0.866025403784439,1.,0.866025403784439,
1.,0.866025403784439,1.,0.866025403784439,1.,0.866025403784439,1.,0.866025403784439,
1.,0.866025403784439,1.,0.866025403784439,1.,0.866025403784439,1.,0.866025403784439,
1.,0.866025403784439,1.,0.866025403784439,1.,0.866025403784439,1.,0.866025403784439,
1.,0.866025403784439,1.,0.866025403784439,1.,0.866025403784439,1.,0.866025403784439,
1.,0.866025403784439,1.,0.866025403784439,1.,0.866025403784439,1.,0.866025403784439,
1.,0.866025403784439,1.,0.866025403784439,1.,0.866025403784439,1.,0.866025403784439,
1.,0.866025403784439,1.,0.866025403784439,1.,0.866025403784439,1.,0.866025403784439,
1.,0.866025403784439,1.,0.866025403784439,1.,0.866025403784439,1.,0.866025403784439,
1.,0.866025403784439,1.,0.866025403784439,1.,0.866025403784439,1.,0.866025403784439,
1.,0.866025403784439,1.,0.866025403784439,1.,0.866025403784439,1.,0.866025403784439,
1.,0.866025403784439,1.,0.866025403784439,1.,0.866025403784439,1.,0.866025403784439,
1.,0.866025403784439,1.,0.866025403784439,1.,0.866025403784439,1.,0.866025403784439,
1.,0.866025403784439,1.,0.866025403784439,1.,0.866025403784439,1.,0.866025403784439,
1.,0.866025403784439,1.,0.866025403784439,1.,0.866025403784439,1.,0.866025403784439,
1.,0.866025403784439,1.,0.866025403784439,1.,0.866025403784439,1.,0.866025403784439,
1.,0.866025403784439,1.,0.866025403784439,1.,0.866025403784439,1.,0.866025403784439,
1.,0.866025403784439,1.,0.866025403784439,1.,0.866025403784439,1.,0.866025403784439,
1.,0.866025403784439,1.,0.866025403784439,1.,0.866025403784439,1.,0.866025403784439,
1.,0.866025403784439,1.,0.866025403784439,1.,0.866025403784439,1.,0.866025403784439,
1.,0.866025403784439,1.,0.866025403784439,1.,0.866025403784439,1.,0.866025403784439,
1.,0.866025403784439,1.,0.866025403784439,1.,0.866025403784439,1.,0.866025403784439,
1.,0.866025403784439,1.,0.866025403784439,1.,0.866025403784439,1.,0.866025403784439,
1.,0.866025403784439,1.,0.866025403784439,1.,0.866025403784439,1.,0.866025403784439,
1.,0.866025403784439,1.,0.866025403784439,1.,0.866025403784439,1.,0.866025403784439,
1.,0.866025403784439,1.,0.866025403784439,1.,0.866025403784439,1.,0.866025403784439,
1.,0.866025403784439,1.,0.866025403784439,1.,0.866025403784439,1.,0.866025403784439,
1.,0.866025403784439,1.,0.866025403784439,1.,0.866025403784439,1.,0.866025403784439,
1.,0.866025403784439,1.,0.866025403784439,1.,0.866025403784439,1.,0.866025403784439,
1.,0.866025403784439,1.,0.866025403784439,1.,0.866025403784439,1.,0.866025403784439,
1.,0.866025403784439,1.,0.866025403784439,1.,0.866025403784439,1.,0.866025403784439,
1.,0.946113621402695,0.935574890499137)))
REPRESENTATION_ITEM('')
SURFACE()
);
#291=(
BOUNDED_SURFACE()
B_SPLINE_SURFACE(1,2,((#25988,#25989,#25990,#25991,#25992,#25993,#25994,
#25995,#25996,#25997,#25998,#25999,#26000,#26001,#26002,#26003,#26004,#26005,
#26006,#26007,#26008,#26009,#26010,#26011,#26012,#26013,#26014,#26015,#26016,
#26017,#26018,#26019,#26020,#26021,#26022,#26023,#26024,#26025,#26026,#26027,
#26028,#26029,#26030,#26031,#26032,#26033,#26034,#26035,#26036,#26037,#26038,
#26039,#26040,#26041,#26042,#26043,#26044,#26045,#26046,#26047,#26048,#26049,
#26050,#26051,#26052,#26053,#26054,#26055,#26056,#26057,#26058,#26059,#26060,
#26061,#26062,#26063,#26064,#26065,#26066,#26067,#26068,#26069,#26070,#26071,
#26072,#26073,#26074,#26075,#26076,#26077,#26078,#26079,#26080,#26081,#26082,
#26083,#26084,#26085,#26086,#26087,#26088,#26089,#26090,#26091,#26092,#26093,
#26094,#26095,#26096,#26097,#26098,#26099,#26100,#26101,#26102,#26103,#26104,
#26105,#26106,#26107,#26108,#26109,#26110,#26111,#26112,#26113,#26114,#26115,
#26116,#26117,#26118,#26119,#26120,#26121,#26122,#26123,#26124,#26125,#26126,
#26127,#26128,#26129,#26130,#26131,#26132,#26133,#26134,#26135,#26136,#26137,
#26138,#26139,#26140,#26141,#26142,#26143,#26144,#26145,#26146,#26147,#26148,
#26149,#26150,#26151,#26152,#26153,#26154,#26155,#26156,#26157,#26158,#26159,
#26160,#26161,#26162,#26163,#26164,#26165,#26166,#26167,#26168,#26169,#26170,
#26171,#26172,#26173,#26174,#26175,#26176,#26177,#26178,#26179,#26180,#26181,
#26182,#26183,#26184,#26185,#26186,#26187,#26188,#26189,#26190,#26191,#26192,
#26193,#26194,#26195,#26196,#26197,#26198,#26199,#26200,#26201,#26202,#26203,
#26204,#26205,#26206,#26207,#26208,#26209,#26210,#26211,#26212,#26213,#26214,
#26215,#26216,#26217,#26218,#26219,#26220,#26221,#26222,#26223,#26224,#26225,
#26226,#26227,#26228,#26229,#26230,#26231,#26232,#26233,#26234,#26235,#26236,
#26237,#26238,#26239,#26240,#26241,#26242,#26243,#26244,#26245,#26246,#26247,
#26248,#26249,#26250,#26251,#26252,#26253,#26254,#26255,#26256,#26257,#26258,
#26259,#26260,#26261,#26262,#26263,#26264,#26265,#26266,#26267,#26268,#26269,
#26270,#26271,#26272,#26273,#26274,#26275,#26276,#26277,#26278,#26279,#26280,
#26281,#26282,#26283,#26284,#26285,#26286,#26287,#26288,#26289,#26290,#26291,
#26292,#26293,#26294,#26295,#26296,#26297,#26298,#26299,#26300,#26301,#26302,
#26303,#26304,#26305,#26306,#26307,#26308),(#26309,#26310,#26311,#26312,
#26313,#26314,#26315,#26316,#26317,#26318,#26319,#26320,#26321,#26322,#26323,
#26324,#26325,#26326,#26327,#26328,#26329,#26330,#26331,#26332,#26333,#26334,
#26335,#26336,#26337,#26338,#26339,#26340,#26341,#26342,#26343,#26344,#26345,
#26346,#26347,#26348,#26349,#26350,#26351,#26352,#26353,#26354,#26355,#26356,
#26357,#26358,#26359,#26360,#26361,#26362,#26363,#26364,#26365,#26366,#26367,
#26368,#26369,#26370,#26371,#26372,#26373,#26374,#26375,#26376,#26377,#26378,
#26379,#26380,#26381,#26382,#26383,#26384,#26385,#26386,#26387,#26388,#26389,
#26390,#26391,#26392,#26393,#26394,#26395,#26396,#26397,#26398,#26399,#26400,
#26401,#26402,#26403,#26404,#26405,#26406,#26407,#26408,#26409,#26410,#26411,
#26412,#26413,#26414,#26415,#26416,#26417,#26418,#26419,#26420,#26421,#26422,
#26423,#26424,#26425,#26426,#26427,#26428,#26429,#26430,#26431,#26432,#26433,
#26434,#26435,#26436,#26437,#26438,#26439,#26440,#26441,#26442,#26443,#26444,
#26445,#26446,#26447,#26448,#26449,#26450,#26451,#26452,#26453,#26454,#26455,
#26456,#26457,#26458,#26459,#26460,#26461,#26462,#26463,#26464,#26465,#26466,
#26467,#26468,#26469,#26470,#26471,#26472,#26473,#26474,#26475,#26476,#26477,
#26478,#26479,#26480,#26481,#26482,#26483,#26484,#26485,#26486,#26487,#26488,
#26489,#26490,#26491,#26492,#26493,#26494,#26495,#26496,#26497,#26498,#26499,
#26500,#26501,#26502,#26503,#26504,#26505,#26506,#26507,#26508,#26509,#26510,
#26511,#26512,#26513,#26514,#26515,#26516,#26517,#26518,#26519,#26520,#26521,
#26522,#26523,#26524,#26525,#26526,#26527,#26528,#26529,#26530,#26531,#26532,
#26533,#26534,#26535,#26536,#26537,#26538,#26539,#26540,#26541,#26542,#26543,
#26544,#26545,#26546,#26547,#26548,#26549,#26550,#26551,#26552,#26553,#26554,
#26555,#26556,#26557,#26558,#26559,#26560,#26561,#26562,#26563,#26564,#26565,
#26566,#26567,#26568,#26569,#26570,#26571,#26572,#26573,#26574,#26575,#26576,
#26577,#26578,#26579,#26580,#26581,#26582,#26583,#26584,#26585,#26586,#26587,
#26588,#26589,#26590,#26591,#26592,#26593,#26594,#26595,#26596,#26597,#26598,
#26599,#26600,#26601,#26602,#26603,#26604,#26605,#26606,#26607,#26608,#26609,
#26610,#26611,#26612,#26613,#26614,#26615,#26616,#26617,#26618,#26619,#26620,
#26621,#26622,#26623,#26624,#26625,#26626,#26627,#26628,#26629)),
 .UNSPECIFIED.,.F.,.F.,.F.)
B_SPLINE_SURFACE_WITH_KNOTS((2,2),(3,2,2,2,2,2,2,2,2,2,2,2,2,2,2,2,2,2,
2,2,2,2,2,2,2,2,2,2,2,2,2,2,2,2,2,2,2,2,2,2,2,2,2,2,2,2,2,2,2,2,2,2,2,2,
2,2,2,2,2,2,2,2,2,2,2,2,2,2,2,2,2,2,2,2,2,2,2,2,2,2,2,2,2,2,2,2,2,2,2,2,
2,2,2,2,2,2,2,2,2,2,2,2,2,2,2,2,2,2,2,2,2,2,2,2,2,2,2,2,2,2,2,2,2,2,2,2,
2,2,2,2,2,2,2,2,2,2,2,2,2,2,2,2,2,2,2,2,2,2,2,2,2,2,2,2,2,2,2,2,2,2,3),
(-0.000321975171232605,1.),(0.,0.00617283950617284,0.0123456790123457,0.0185185185185185,
0.0246913580246914,0.0308641975308642,0.037037037037037,0.0432098765432099,
0.0493827160493827,0.0555555555555556,0.0617283950617284,0.0679012345679012,
0.0740740740740741,0.0802469135802469,0.0864197530864197,0.0925925925925926,
0.0987654320987654,0.104938271604938,0.111111111111111,0.117283950617284,
0.123456790123457,0.12962962962963,0.135802469135802,0.141975308641975,
0.148148148148148,0.154320987654321,0.160493827160494,0.166666666666667,
0.172839506172839,0.179012345679012,0.185185185185185,0.191358024691358,
0.197530864197531,0.203703703703704,0.209876543209877,0.216049382716049,
0.222222222222222,0.228395061728395,0.234567901234568,0.240740740740741,
0.246913580246914,0.253086419753086,0.259259259259259,0.265432098765432,
0.271604938271605,0.277777777777778,0.283950617283951,0.290123456790123,
0.296296296296296,0.302469135802469,0.308641975308642,0.314814814814815,
0.320987654320988,0.327160493827161,0.333333333333333,0.339506172839506,
0.345679012345679,0.351851851851852,0.358024691358025,0.364197530864198,
0.37037037037037,0.376543209876543,0.382716049382716,0.388888888888889,
0.395061728395062,0.401234567901235,0.407407407407407,0.41358024691358,
0.419753086419753,0.425925925925926,0.432098765432099,0.438271604938272,
0.444444444444444,0.450617283950617,0.45679012345679,0.462962962962963,
0.469135802469136,0.475308641975309,0.481481481481481,0.487654320987654,
0.493827160493827,0.5,0.506172839506173,0.512345679012346,0.518518518518518,
0.524691358024691,0.530864197530864,0.537037037037037,0.54320987654321,
0.549382716049383,0.555555555555556,0.561728395061728,0.567901234567901,
0.574074074074074,0.580246913580247,0.58641975308642,0.592592592592593,
0.598765432098765,0.604938271604938,0.611111111111111,0.617283950617284,
0.623456790123457,0.62962962962963,0.635802469135803,0.641975308641975,
0.648148148148148,0.654320987654321,0.660493827160494,0.666666666666667,
0.672839506172839,0.679012345679012,0.685185185185185,0.691358024691358,
0.697530864197531,0.703703703703704,0.709876543209877,0.716049382716049,
0.722222222222222,0.728395061728395,0.734567901234568,0.740740740740741,
0.746913580246914,0.753086419753086,0.759259259259259,0.765432098765432,
0.771604938271605,0.777777777777778,0.783950617283951,0.790123456790123,
0.796296296296296,0.802469135802469,0.808641975308642,0.814814814814815,
0.820987654320988,0.827160493827161,0.833333333333333,0.839506172839506,
0.845679012345679,0.851851851851852,0.858024691358025,0.864197530864197,
0.87037037037037,0.876543209876543,0.882716049382716,0.888888888888889,
0.895061728395062,0.901234567901235,0.907407407407407,0.91358024691358,
0.919753086419753,0.925925925925926,0.932098765432099,0.938271604938272,
0.944444444444444,0.950617283950617,0.95679012345679,0.962962962962963,
0.969135802469136,0.975308641975309,0.977791393533952,0.987569307469292),
 .UNSPECIFIED.)
GEOMETRIC_REPRESENTATION_ITEM()
RATIONAL_B_SPLINE_SURFACE(((1.,0.866025403784439,1.,0.866025403784439,1.,
0.866025403784439,1.,0.866025403784439,1.,0.866025403784439,1.,0.866025403784439,
1.,0.866025403784439,1.,0.866025403784439,1.,0.866025403784439,1.,0.866025403784439,
1.,0.866025403784439,1.,0.866025403784439,1.,0.866025403784439,1.,0.866025403784439,
1.,0.866025403784439,1.,0.866025403784439,1.,0.866025403784439,1.,0.866025403784439,
1.,0.866025403784439,1.,0.866025403784439,1.,0.866025403784439,1.,0.866025403784439,
1.,0.866025403784439,1.,0.866025403784439,1.,0.866025403784439,1.,0.866025403784439,
1.,0.866025403784439,1.,0.866025403784439,1.,0.866025403784439,1.,0.866025403784439,
1.,0.866025403784439,1.,0.866025403784439,1.,0.866025403784439,1.,0.866025403784439,
1.,0.866025403784439,1.,0.866025403784439,1.,0.866025403784439,1.,0.866025403784439,
1.,0.866025403784439,1.,0.866025403784439,1.,0.866025403784439,1.,0.866025403784439,
1.,0.866025403784439,1.,0.866025403784439,1.,0.866025403784439,1.,0.866025403784439,
1.,0.866025403784439,1.,0.866025403784439,1.,0.866025403784439,1.,0.866025403784439,
1.,0.866025403784439,1.,0.866025403784439,1.,0.866025403784439,1.,0.866025403784439,
1.,0.866025403784439,1.,0.866025403784439,1.,0.866025403784439,1.,0.866025403784439,
1.,0.866025403784439,1.,0.866025403784439,1.,0.866025403784439,1.,0.866025403784439,
1.,0.866025403784439,1.,0.866025403784439,1.,0.866025403784439,1.,0.866025403784439,
1.,0.866025403784439,1.,0.866025403784439,1.,0.866025403784439,1.,0.866025403784439,
1.,0.866025403784439,1.,0.866025403784439,1.,0.866025403784439,1.,0.866025403784439,
1.,0.866025403784439,1.,0.866025403784439,1.,0.866025403784439,1.,0.866025403784439,
1.,0.866025403784439,1.,0.866025403784439,1.,0.866025403784439,1.,0.866025403784439,
1.,0.866025403784439,1.,0.866025403784439,1.,0.866025403784439,1.,0.866025403784439,
1.,0.866025403784439,1.,0.866025403784439,1.,0.866025403784439,1.,0.866025403784439,
1.,0.866025403784439,1.,0.866025403784439,1.,0.866025403784439,1.,0.866025403784439,
1.,0.866025403784439,1.,0.866025403784439,1.,0.866025403784439,1.,0.866025403784439,
1.,0.866025403784439,1.,0.866025403784439,1.,0.866025403784439,1.,0.866025403784439,
1.,0.866025403784439,1.,0.866025403784439,1.,0.866025403784439,1.,0.866025403784439,
1.,0.866025403784439,1.,0.866025403784439,1.,0.866025403784439,1.,0.866025403784439,
1.,0.866025403784439,1.,0.866025403784439,1.,0.866025403784439,1.,0.866025403784439,
1.,0.866025403784439,1.,0.866025403784439,1.,0.866025403784439,1.,0.866025403784439,
1.,0.866025403784439,1.,0.866025403784439,1.,0.866025403784439,1.,0.866025403784439,
1.,0.866025403784439,1.,0.866025403784439,1.,0.866025403784439,1.,0.866025403784439,
1.,0.866025403784439,1.,0.866025403784439,1.,0.866025403784439,1.,0.866025403784439,
1.,0.866025403784439,1.,0.866025403784439,1.,0.866025403784439,1.,0.866025403784439,
1.,0.866025403784439,1.,0.866025403784439,1.,0.866025403784439,1.,0.866025403784439,
1.,0.866025403784439,1.,0.866025403784439,1.,0.866025403784439,1.,0.866025403784439,
1.,0.866025403784439,1.,0.866025403784439,1.,0.866025403784439,1.,0.866025403784439,
1.,0.866025403784439,1.,0.866025403784439,1.,0.866025403784439,1.,0.866025403784439,
1.,0.866025403784439,1.,0.866025403784439,1.,0.866025403784439,1.,0.866025403784439,
1.,0.866025403784439,1.,0.866025403784439,1.,0.866025403784439,1.,0.866025403784439,
1.,0.946114646713198,0.93557529156132,0.93557529156132,0.93557529156132),
(1.,0.866025403784439,1.,0.866025403784439,1.,0.866025403784439,1.,0.866025403784439,
1.,0.866025403784439,1.,0.866025403784439,1.,0.866025403784439,1.,0.866025403784439,
1.,0.866025403784439,1.,0.866025403784439,1.,0.866025403784439,1.,0.866025403784439,
1.,0.866025403784439,1.,0.866025403784439,1.,0.866025403784439,1.,0.866025403784439,
1.,0.866025403784439,1.,0.866025403784439,1.,0.866025403784439,1.,0.866025403784439,
1.,0.866025403784439,1.,0.866025403784439,1.,0.866025403784439,1.,0.866025403784439,
1.,0.866025403784439,1.,0.866025403784439,1.,0.866025403784439,1.,0.866025403784439,
1.,0.866025403784439,1.,0.866025403784439,1.,0.866025403784439,1.,0.866025403784439,
1.,0.866025403784439,1.,0.866025403784439,1.,0.866025403784439,1.,0.866025403784439,
1.,0.866025403784439,1.,0.866025403784439,1.,0.866025403784439,1.,0.866025403784439,
1.,0.866025403784439,1.,0.866025403784439,1.,0.866025403784439,1.,0.866025403784439,
1.,0.866025403784439,1.,0.866025403784439,1.,0.866025403784439,1.,0.866025403784439,
1.,0.866025403784439,1.,0.866025403784439,1.,0.866025403784439,1.,0.866025403784439,
1.,0.866025403784439,1.,0.866025403784439,1.,0.866025403784439,1.,0.866025403784439,
1.,0.866025403784439,1.,0.866025403784439,1.,0.866025403784439,1.,0.866025403784439,
1.,0.866025403784439,1.,0.866025403784439,1.,0.866025403784439,1.,0.866025403784439,
1.,0.866025403784439,1.,0.866025403784439,1.,0.866025403784439,1.,0.866025403784439,
1.,0.866025403784439,1.,0.866025403784439,1.,0.866025403784439,1.,0.866025403784439,
1.,0.866025403784439,1.,0.866025403784439,1.,0.866025403784439,1.,0.866025403784439,
1.,0.866025403784439,1.,0.866025403784439,1.,0.866025403784439,1.,0.866025403784439,
1.,0.866025403784439,1.,0.866025403784439,1.,0.866025403784439,1.,0.866025403784439,
1.,0.866025403784439,1.,0.866025403784439,1.,0.866025403784439,1.,0.866025403784439,
1.,0.866025403784439,1.,0.866025403784439,1.,0.866025403784439,1.,0.866025403784439,
1.,0.866025403784439,1.,0.866025403784439,1.,0.866025403784439,1.,0.866025403784439,
1.,0.866025403784439,1.,0.866025403784439,1.,0.866025403784439,1.,0.866025403784439,
1.,0.866025403784439,1.,0.866025403784439,1.,0.866025403784439,1.,0.866025403784439,
1.,0.866025403784439,1.,0.866025403784439,1.,0.866025403784439,1.,0.866025403784439,
1.,0.866025403784439,1.,0.866025403784439,1.,0.866025403784439,1.,0.866025403784439,
1.,0.866025403784439,1.,0.866025403784439,1.,0.866025403784439,1.,0.866025403784439,
1.,0.866025403784439,1.,0.866025403784439,1.,0.866025403784439,1.,0.866025403784439,
1.,0.866025403784439,1.,0.866025403784439,1.,0.866025403784439,1.,0.866025403784439,
1.,0.866025403784439,1.,0.866025403784439,1.,0.866025403784439,1.,0.866025403784439,
1.,0.866025403784439,1.,0.866025403784439,1.,0.866025403784439,1.,0.866025403784439,
1.,0.866025403784439,1.,0.866025403784439,1.,0.866025403784439,1.,0.866025403784439,
1.,0.866025403784439,1.,0.866025403784439,1.,0.866025403784439,1.,0.866025403784439,
1.,0.866025403784439,1.,0.866025403784439,1.,0.866025403784439,1.,0.866025403784439,
1.,0.866025403784439,1.,0.866025403784439,1.,0.866025403784439,1.,0.866025403784439,
1.,0.866025403784439,1.,0.866025403784439,1.,0.866025403784439,1.,0.866025403784439,
1.,0.866025403784439,1.,0.866025403784439,1.,0.866025403784439,1.,0.866025403784439,
1.,0.866025403784439,1.,0.866025403784439,1.,0.946114646713198,0.93557529156132,
0.93557529156132,0.93557529156132)))
REPRESENTATION_ITEM('')
SURFACE()
);
#292=(
BOUNDED_SURFACE()
B_SPLINE_SURFACE(1,2,((#26653,#26654,#26655,#26656,#26657,#26658,#26659,
#26660,#26661,#26662,#26663,#26664,#26665,#26666,#26667,#26668,#26669,#26670,
#26671,#26672,#26673,#26674,#26675,#26676,#26677,#26678,#26679,#26680,#26681,
#26682,#26683,#26684,#26685,#26686,#26687,#26688,#26689,#26690,#26691,#26692,
#26693,#26694,#26695,#26696,#26697,#26698,#26699,#26700,#26701,#26702,#26703,
#26704,#26705,#26706,#26707,#26708,#26709,#26710,#26711,#26712,#26713,#26714,
#26715,#26716,#26717,#26718,#26719,#26720,#26721,#26722,#26723,#26724,#26725,
#26726,#26727,#26728,#26729,#26730,#26731,#26732,#26733,#26734,#26735,#26736,
#26737,#26738,#26739,#26740,#26741,#26742,#26743,#26744,#26745,#26746,#26747,
#26748,#26749,#26750,#26751,#26752,#26753,#26754,#26755,#26756,#26757,#26758,
#26759,#26760,#26761,#26762,#26763,#26764,#26765,#26766,#26767,#26768,#26769,
#26770,#26771,#26772,#26773,#26774,#26775,#26776,#26777,#26778,#26779,#26780,
#26781,#26782,#26783,#26784,#26785,#26786,#26787,#26788,#26789,#26790,#26791,
#26792,#26793,#26794,#26795,#26796,#26797,#26798,#26799,#26800,#26801,#26802,
#26803,#26804,#26805,#26806,#26807,#26808,#26809,#26810,#26811,#26812,#26813,
#26814,#26815,#26816,#26817,#26818,#26819,#26820,#26821,#26822,#26823,#26824,
#26825,#26826,#26827,#26828,#26829,#26830,#26831,#26832,#26833,#26834,#26835,
#26836,#26837,#26838,#26839,#26840,#26841,#26842,#26843,#26844,#26845,#26846,
#26847,#26848,#26849,#26850,#26851,#26852,#26853,#26854,#26855,#26856,#26857,
#26858,#26859,#26860,#26861,#26862,#26863,#26864,#26865,#26866,#26867,#26868,
#26869,#26870,#26871,#26872,#26873,#26874,#26875,#26876,#26877,#26878,#26879,
#26880,#26881,#26882,#26883,#26884,#26885,#26886,#26887,#26888,#26889,#26890,
#26891,#26892,#26893,#26894,#26895,#26896,#26897,#26898,#26899,#26900,#26901,
#26902,#26903,#26904,#26905,#26906,#26907,#26908,#26909,#26910,#26911,#26912,
#26913,#26914,#26915,#26916,#26917,#26918,#26919,#26920,#26921,#26922,#26923,
#26924,#26925,#26926,#26927,#26928,#26929,#26930,#26931,#26932,#26933,#26934,
#26935,#26936,#26937,#26938,#26939,#26940,#26941,#26942,#26943,#26944,#26945,
#26946,#26947,#26948,#26949,#26950,#26951,#26952,#26953,#26954,#26955,#26956,
#26957,#26958,#26959,#26960,#26961,#26962,#26963,#26964,#26965,#26966,#26967,
#26968,#26969,#26970,#26971),(#26972,#26973,#26974,#26975,#26976,#26977,
#26978,#26979,#26980,#26981,#26982,#26983,#26984,#26985,#26986,#26987,#26988,
#26989,#26990,#26991,#26992,#26993,#26994,#26995,#26996,#26997,#26998,#26999,
#27000,#27001,#27002,#27003,#27004,#27005,#27006,#27007,#27008,#27009,#27010,
#27011,#27012,#27013,#27014,#27015,#27016,#27017,#27018,#27019,#27020,#27021,
#27022,#27023,#27024,#27025,#27026,#27027,#27028,#27029,#27030,#27031,#27032,
#27033,#27034,#27035,#27036,#27037,#27038,#27039,#27040,#27041,#27042,#27043,
#27044,#27045,#27046,#27047,#27048,#27049,#27050,#27051,#27052,#27053,#27054,
#27055,#27056,#27057,#27058,#27059,#27060,#27061,#27062,#27063,#27064,#27065,
#27066,#27067,#27068,#27069,#27070,#27071,#27072,#27073,#27074,#27075,#27076,
#27077,#27078,#27079,#27080,#27081,#27082,#27083,#27084,#27085,#27086,#27087,
#27088,#27089,#27090,#27091,#27092,#27093,#27094,#27095,#27096,#27097,#27098,
#27099,#27100,#27101,#27102,#27103,#27104,#27105,#27106,#27107,#27108,#27109,
#27110,#27111,#27112,#27113,#27114,#27115,#27116,#27117,#27118,#27119,#27120,
#27121,#27122,#27123,#27124,#27125,#27126,#27127,#27128,#27129,#27130,#27131,
#27132,#27133,#27134,#27135,#27136,#27137,#27138,#27139,#27140,#27141,#27142,
#27143,#27144,#27145,#27146,#27147,#27148,#27149,#27150,#27151,#27152,#27153,
#27154,#27155,#27156,#27157,#27158,#27159,#27160,#27161,#27162,#27163,#27164,
#27165,#27166,#27167,#27168,#27169,#27170,#27171,#27172,#27173,#27174,#27175,
#27176,#27177,#27178,#27179,#27180,#27181,#27182,#27183,#27184,#27185,#27186,
#27187,#27188,#27189,#27190,#27191,#27192,#27193,#27194,#27195,#27196,#27197,
#27198,#27199,#27200,#27201,#27202,#27203,#27204,#27205,#27206,#27207,#27208,
#27209,#27210,#27211,#27212,#27213,#27214,#27215,#27216,#27217,#27218,#27219,
#27220,#27221,#27222,#27223,#27224,#27225,#27226,#27227,#27228,#27229,#27230,
#27231,#27232,#27233,#27234,#27235,#27236,#27237,#27238,#27239,#27240,#27241,
#27242,#27243,#27244,#27245,#27246,#27247,#27248,#27249,#27250,#27251,#27252,
#27253,#27254,#27255,#27256,#27257,#27258,#27259,#27260,#27261,#27262,#27263,
#27264,#27265,#27266,#27267,#27268,#27269,#27270,#27271,#27272,#27273,#27274,
#27275,#27276,#27277,#27278,#27279,#27280,#27281,#27282,#27283,#27284,#27285,
#27286,#27287,#27288,#27289,#27290)),.UNSPECIFIED.,.F.,.F.,.F.)
B_SPLINE_SURFACE_WITH_KNOTS((2,2),(3,2,2,2,2,2,2,2,2,2,2,2,2,2,2,2,2,2,
2,2,2,2,2,2,2,2,2,2,2,2,2,2,2,2,2,2,2,2,2,2,2,2,2,2,2,2,2,2,2,2,2,2,2,2,
2,2,2,2,2,2,2,2,2,2,2,2,2,2,2,2,2,2,2,2,2,2,2,2,2,2,2,2,2,2,2,2,2,2,2,2,
2,2,2,2,2,2,2,2,2,2,2,2,2,2,2,2,2,2,2,2,2,2,2,2,2,2,2,2,2,2,2,2,2,2,2,2,
2,2,2,2,2,2,2,2,2,2,2,2,2,2,2,2,2,2,2,2,2,2,2,2,2,2,2,2,2,2,2,2,2,3),(-2.47338691325004E-5,
1.),(0.,0.00617283950617284,0.0123456790123457,0.0185185185185185,0.0246913580246914,
0.0308641975308642,0.037037037037037,0.0432098765432099,0.0493827160493827,
0.0555555555555556,0.0617283950617284,0.0679012345679012,0.0740740740740741,
0.0802469135802469,0.0864197530864197,0.0925925925925926,0.0987654320987654,
0.104938271604938,0.111111111111111,0.117283950617284,0.123456790123457,
0.12962962962963,0.135802469135802,0.141975308641975,0.148148148148148,
0.154320987654321,0.160493827160494,0.166666666666667,0.172839506172839,
0.179012345679012,0.185185185185185,0.191358024691358,0.197530864197531,
0.203703703703704,0.209876543209877,0.216049382716049,0.222222222222222,
0.228395061728395,0.234567901234568,0.240740740740741,0.246913580246914,
0.253086419753086,0.259259259259259,0.265432098765432,0.271604938271605,
0.277777777777778,0.283950617283951,0.290123456790123,0.296296296296296,
0.302469135802469,0.308641975308642,0.314814814814815,0.320987654320988,
0.327160493827161,0.333333333333333,0.339506172839506,0.345679012345679,
0.351851851851852,0.358024691358025,0.364197530864198,0.37037037037037,
0.376543209876543,0.382716049382716,0.388888888888889,0.395061728395062,
0.401234567901235,0.407407407407407,0.41358024691358,0.419753086419753,
0.425925925925926,0.432098765432099,0.438271604938272,0.444444444444444,
0.450617283950617,0.45679012345679,0.462962962962963,0.469135802469136,
0.475308641975309,0.481481481481481,0.487654320987654,0.493827160493827,
0.5,0.506172839506173,0.512345679012346,0.518518518518518,0.524691358024691,
0.530864197530864,0.537037037037037,0.54320987654321,0.549382716049383,
0.555555555555556,0.561728395061728,0.567901234567901,0.574074074074074,
0.580246913580247,0.58641975308642,0.592592592592593,0.598765432098765,
0.604938271604938,0.611111111111111,0.617283950617284,0.623456790123457,
0.62962962962963,0.635802469135803,0.641975308641975,0.648148148148148,
0.654320987654321,0.660493827160494,0.666666666666667,0.672839506172839,
0.679012345679012,0.685185185185185,0.691358024691358,0.697530864197531,
0.703703703703704,0.709876543209877,0.716049382716049,0.722222222222222,
0.728395061728395,0.734567901234568,0.740740740740741,0.746913580246914,
0.753086419753086,0.759259259259259,0.765432098765432,0.771604938271605,
0.777777777777778,0.783950617283951,0.790123456790123,0.796296296296296,
0.802469135802469,0.808641975308642,0.814814814814815,0.820987654320988,
0.827160493827161,0.833333333333333,0.839506172839506,0.845679012345679,
0.851851851851852,0.858024691358025,0.864197530864197,0.87037037037037,
0.876543209876543,0.882716049382716,0.888888888888889,0.895061728395062,
0.901234567901235,0.907407407407407,0.91358024691358,0.919753086419753,
0.925925925925926,0.932098765432099,0.938271604938272,0.944444444444444,
0.950617283950617,0.95679012345679,0.962962962962963,0.969135802469136,
0.975308641975309,0.977791447664447),.UNSPECIFIED.)
GEOMETRIC_REPRESENTATION_ITEM()
RATIONAL_B_SPLINE_SURFACE(((1.,0.866025403784439,1.,0.866025403784439,1.,
0.866025403784439,1.,0.866025403784439,1.,0.866025403784439,1.,0.866025403784439,
1.,0.866025403784439,1.,0.866025403784439,1.,0.866025403784439,1.,0.866025403784439,
1.,0.866025403784439,1.,0.866025403784439,1.,0.866025403784439,1.,0.866025403784439,
1.,0.866025403784439,1.,0.866025403784439,1.,0.866025403784439,1.,0.866025403784439,
1.,0.866025403784439,1.,0.866025403784439,1.,0.866025403784439,1.,0.866025403784439,
1.,0.866025403784439,1.,0.866025403784439,1.,0.866025403784439,1.,0.866025403784439,
1.,0.866025403784439,1.,0.866025403784439,1.,0.866025403784439,1.,0.866025403784439,
1.,0.866025403784439,1.,0.866025403784439,1.,0.866025403784439,1.,0.866025403784439,
1.,0.866025403784439,1.,0.866025403784439,1.,0.866025403784439,1.,0.866025403784439,
1.,0.866025403784439,1.,0.866025403784439,1.,0.866025403784439,1.,0.866025403784439,
1.,0.866025403784439,1.,0.866025403784439,1.,0.866025403784439,1.,0.866025403784439,
1.,0.866025403784439,1.,0.866025403784439,1.,0.866025403784439,1.,0.866025403784439,
1.,0.866025403784439,1.,0.866025403784439,1.,0.866025403784439,1.,0.866025403784439,
1.,0.866025403784439,1.,0.866025403784439,1.,0.866025403784439,1.,0.866025403784439,
1.,0.866025403784439,1.,0.866025403784439,1.,0.866025403784439,1.,0.866025403784439,
1.,0.866025403784439,1.,0.866025403784439,1.,0.866025403784439,1.,0.866025403784439,
1.,0.866025403784439,1.,0.866025403784439,1.,0.866025403784439,1.,0.866025403784439,
1.,0.866025403784439,1.,0.866025403784439,1.,0.866025403784439,1.,0.866025403784439,
1.,0.866025403784439,1.,0.866025403784439,1.,0.866025403784439,1.,0.866025403784439,
1.,0.866025403784439,1.,0.866025403784439,1.,0.866025403784439,1.,0.866025403784439,
1.,0.866025403784439,1.,0.866025403784439,1.,0.866025403784439,1.,0.866025403784439,
1.,0.866025403784439,1.,0.866025403784439,1.,0.866025403784439,1.,0.866025403784439,
1.,0.866025403784439,1.,0.866025403784439,1.,0.866025403784439,1.,0.866025403784439,
1.,0.866025403784439,1.,0.866025403784439,1.,0.866025403784439,1.,0.866025403784439,
1.,0.866025403784439,1.,0.866025403784439,1.,0.866025403784439,1.,0.866025403784439,
1.,0.866025403784439,1.,0.866025403784439,1.,0.866025403784439,1.,0.866025403784439,
1.,0.866025403784439,1.,0.866025403784439,1.,0.866025403784439,1.,0.866025403784439,
1.,0.866025403784439,1.,0.866025403784439,1.,0.866025403784439,1.,0.866025403784439,
1.,0.866025403784439,1.,0.866025403784439,1.,0.866025403784439,1.,0.866025403784439,
1.,0.866025403784439,1.,0.866025403784439,1.,0.866025403784439,1.,0.866025403784439,
1.,0.866025403784439,1.,0.866025403784439,1.,0.866025403784439,1.,0.866025403784439,
1.,0.866025403784439,1.,0.866025403784439,1.,0.866025403784439,1.,0.866025403784439,
1.,0.866025403784439,1.,0.866025403784439,1.,0.866025403784439,1.,0.866025403784439,
1.,0.866025403784439,1.,0.866025403784439,1.,0.866025403784439,1.,0.866025403784439,
1.,0.866025403784439,1.,0.866025403784439,1.,0.866025403784439,1.,0.866025403784439,
1.,0.866025403784439,1.,0.866025403784439,1.,0.866025403784439,1.,0.866025403784439,
1.,0.866025403784439,1.,0.866025403784439,1.,0.866025403784439,1.,0.866025403784439,
1.,0.866025403784439,1.,0.866025403784439,1.,0.866025403784439,1.,0.866025403784439,
1.,0.866025403784439,1.,0.866025403784439,1.,0.866025403784439,1.,0.866025403784439,
1.,0.9461134718712,0.935574832010768),(1.,0.866025403784439,1.,0.866025403784439,
1.,0.866025403784439,1.,0.866025403784439,1.,0.866025403784439,1.,0.866025403784439,
1.,0.866025403784439,1.,0.866025403784439,1.,0.866025403784439,1.,0.866025403784439,
1.,0.866025403784439,1.,0.866025403784439,1.,0.866025403784439,1.,0.866025403784439,
1.,0.866025403784439,1.,0.866025403784439,1.,0.866025403784439,1.,0.866025403784439,
1.,0.866025403784439,1.,0.866025403784439,1.,0.866025403784439,1.,0.866025403784439,
1.,0.866025403784439,1.,0.866025403784439,1.,0.866025403784439,1.,0.866025403784439,
1.,0.866025403784439,1.,0.866025403784439,1.,0.866025403784439,1.,0.866025403784439,
1.,0.866025403784439,1.,0.866025403784439,1.,0.866025403784439,1.,0.866025403784439,
1.,0.866025403784439,1.,0.866025403784439,1.,0.866025403784439,1.,0.866025403784439,
1.,0.866025403784439,1.,0.866025403784439,1.,0.866025403784439,1.,0.866025403784439,
1.,0.866025403784439,1.,0.866025403784439,1.,0.866025403784439,1.,0.866025403784439,
1.,0.866025403784439,1.,0.866025403784439,1.,0.866025403784439,1.,0.866025403784439,
1.,0.866025403784439,1.,0.866025403784439,1.,0.866025403784439,1.,0.866025403784439,
1.,0.866025403784439,1.,0.866025403784439,1.,0.866025403784439,1.,0.866025403784439,
1.,0.866025403784439,1.,0.866025403784439,1.,0.866025403784439,1.,0.866025403784439,
1.,0.866025403784439,1.,0.866025403784439,1.,0.866025403784439,1.,0.866025403784439,
1.,0.866025403784439,1.,0.866025403784439,1.,0.866025403784439,1.,0.866025403784439,
1.,0.866025403784439,1.,0.866025403784439,1.,0.866025403784439,1.,0.866025403784439,
1.,0.866025403784439,1.,0.866025403784439,1.,0.866025403784439,1.,0.866025403784439,
1.,0.866025403784439,1.,0.866025403784439,1.,0.866025403784439,1.,0.866025403784439,
1.,0.866025403784439,1.,0.866025403784439,1.,0.866025403784439,1.,0.866025403784439,
1.,0.866025403784439,1.,0.866025403784439,1.,0.866025403784439,1.,0.866025403784439,
1.,0.866025403784439,1.,0.866025403784439,1.,0.866025403784439,1.,0.866025403784439,
1.,0.866025403784439,1.,0.866025403784439,1.,0.866025403784439,1.,0.866025403784439,
1.,0.866025403784439,1.,0.866025403784439,1.,0.866025403784439,1.,0.866025403784439,
1.,0.866025403784439,1.,0.866025403784439,1.,0.866025403784439,1.,0.866025403784439,
1.,0.866025403784439,1.,0.866025403784439,1.,0.866025403784439,1.,0.866025403784439,
1.,0.866025403784439,1.,0.866025403784439,1.,0.866025403784439,1.,0.866025403784439,
1.,0.866025403784439,1.,0.866025403784439,1.,0.866025403784439,1.,0.866025403784439,
1.,0.866025403784439,1.,0.866025403784439,1.,0.866025403784439,1.,0.866025403784439,
1.,0.866025403784439,1.,0.866025403784439,1.,0.866025403784439,1.,0.866025403784439,
1.,0.866025403784439,1.,0.866025403784439,1.,0.866025403784439,1.,0.866025403784439,
1.,0.866025403784439,1.,0.866025403784439,1.,0.866025403784439,1.,0.866025403784439,
1.,0.866025403784439,1.,0.866025403784439,1.,0.866025403784439,1.,0.866025403784439,
1.,0.866025403784439,1.,0.866025403784439,1.,0.866025403784439,1.,0.866025403784439,
1.,0.866025403784439,1.,0.866025403784439,1.,0.866025403784439,1.,0.866025403784439,
1.,0.866025403784439,1.,0.866025403784439,1.,0.866025403784439,1.,0.866025403784439,
1.,0.866025403784439,1.,0.866025403784439,1.,0.866025403784439,1.,0.866025403784439,
1.,0.866025403784439,1.,0.866025403784439,1.,0.866025403784439,1.,0.866025403784439,
1.,0.9461134718712,0.935574832010768)))
REPRESENTATION_ITEM('')
SURFACE()
);
#293=(
BOUNDED_SURFACE()
B_SPLINE_SURFACE(1,2,((#27594,#27595,#27596,#27597,#27598,#27599,#27600,
#27601,#27602,#27603,#27604,#27605,#27606,#27607,#27608,#27609,#27610,#27611,
#27612,#27613,#27614,#27615,#27616,#27617,#27618,#27619,#27620,#27621,#27622,
#27623,#27624,#27625,#27626,#27627,#27628,#27629,#27630,#27631,#27632,#27633,
#27634,#27635,#27636,#27637,#27638,#27639,#27640,#27641,#27642,#27643,#27644,
#27645,#27646,#27647,#27648,#27649,#27650,#27651,#27652,#27653,#27654,#27655,
#27656,#27657,#27658,#27659,#27660,#27661,#27662,#27663,#27664,#27665,#27666,
#27667,#27668,#27669,#27670,#27671,#27672,#27673,#27674,#27675,#27676,#27677,
#27678,#27679,#27680,#27681,#27682,#27683,#27684,#27685,#27686,#27687,#27688,
#27689,#27690,#27691,#27692,#27693,#27694,#27695,#27696,#27697,#27698,#27699,
#27700,#27701,#27702,#27703,#27704,#27705,#27706,#27707,#27708,#27709,#27710,
#27711,#27712,#27713,#27714,#27715,#27716,#27717,#27718,#27719,#27720,#27721,
#27722,#27723,#27724,#27725,#27726,#27727,#27728,#27729,#27730,#27731,#27732,
#27733,#27734,#27735,#27736,#27737,#27738,#27739,#27740,#27741,#27742,#27743,
#27744,#27745,#27746,#27747,#27748,#27749,#27750,#27751,#27752,#27753,#27754,
#27755,#27756,#27757,#27758,#27759,#27760,#27761,#27762,#27763,#27764,#27765,
#27766,#27767,#27768,#27769,#27770,#27771,#27772,#27773,#27774,#27775,#27776,
#27777,#27778,#27779,#27780,#27781,#27782,#27783,#27784,#27785,#27786,#27787,
#27788,#27789,#27790,#27791,#27792,#27793,#27794,#27795,#27796,#27797,#27798,
#27799,#27800,#27801,#27802,#27803,#27804,#27805,#27806,#27807,#27808,#27809,
#27810,#27811,#27812,#27813,#27814,#27815,#27816,#27817,#27818,#27819,#27820,
#27821,#27822,#27823,#27824,#27825,#27826,#27827,#27828,#27829,#27830,#27831,
#27832,#27833,#27834,#27835,#27836,#27837,#27838,#27839,#27840,#27841,#27842,
#27843,#27844,#27845,#27846,#27847,#27848,#27849,#27850,#27851,#27852,#27853,
#27854,#27855,#27856,#27857,#27858,#27859,#27860,#27861,#27862,#27863,#27864,
#27865,#27866,#27867,#27868,#27869,#27870,#27871,#27872,#27873,#27874,#27875,
#27876,#27877,#27878,#27879,#27880,#27881,#27882,#27883,#27884,#27885,#27886,
#27887,#27888,#27889,#27890,#27891,#27892,#27893,#27894,#27895,#27896,#27897,
#27898,#27899,#27900,#27901,#27902,#27903,#27904,#27905,#27906,#27907,#27908,
#27909,#27910,#27911,#27912),(#27913,#27914,#27915,#27916,#27917,#27918,
#27919,#27920,#27921,#27922,#27923,#27924,#27925,#27926,#27927,#27928,#27929,
#27930,#27931,#27932,#27933,#27934,#27935,#27936,#27937,#27938,#27939,#27940,
#27941,#27942,#27943,#27944,#27945,#27946,#27947,#27948,#27949,#27950,#27951,
#27952,#27953,#27954,#27955,#27956,#27957,#27958,#27959,#27960,#27961,#27962,
#27963,#27964,#27965,#27966,#27967,#27968,#27969,#27970,#27971,#27972,#27973,
#27974,#27975,#27976,#27977,#27978,#27979,#27980,#27981,#27982,#27983,#27984,
#27985,#27986,#27987,#27988,#27989,#27990,#27991,#27992,#27993,#27994,#27995,
#27996,#27997,#27998,#27999,#28000,#28001,#28002,#28003,#28004,#28005,#28006,
#28007,#28008,#28009,#28010,#28011,#28012,#28013,#28014,#28015,#28016,#28017,
#28018,#28019,#28020,#28021,#28022,#28023,#28024,#28025,#28026,#28027,#28028,
#28029,#28030,#28031,#28032,#28033,#28034,#28035,#28036,#28037,#28038,#28039,
#28040,#28041,#28042,#28043,#28044,#28045,#28046,#28047,#28048,#28049,#28050,
#28051,#28052,#28053,#28054,#28055,#28056,#28057,#28058,#28059,#28060,#28061,
#28062,#28063,#28064,#28065,#28066,#28067,#28068,#28069,#28070,#28071,#28072,
#28073,#28074,#28075,#28076,#28077,#28078,#28079,#28080,#28081,#28082,#28083,
#28084,#28085,#28086,#28087,#28088,#28089,#28090,#28091,#28092,#28093,#28094,
#28095,#28096,#28097,#28098,#28099,#28100,#28101,#28102,#28103,#28104,#28105,
#28106,#28107,#28108,#28109,#28110,#28111,#28112,#28113,#28114,#28115,#28116,
#28117,#28118,#28119,#28120,#28121,#28122,#28123,#28124,#28125,#28126,#28127,
#28128,#28129,#28130,#28131,#28132,#28133,#28134,#28135,#28136,#28137,#28138,
#28139,#28140,#28141,#28142,#28143,#28144,#28145,#28146,#28147,#28148,#28149,
#28150,#28151,#28152,#28153,#28154,#28155,#28156,#28157,#28158,#28159,#28160,
#28161,#28162,#28163,#28164,#28165,#28166,#28167,#28168,#28169,#28170,#28171,
#28172,#28173,#28174,#28175,#28176,#28177,#28178,#28179,#28180,#28181,#28182,
#28183,#28184,#28185,#28186,#28187,#28188,#28189,#28190,#28191,#28192,#28193,
#28194,#28195,#28196,#28197,#28198,#28199,#28200,#28201,#28202,#28203,#28204,
#28205,#28206,#28207,#28208,#28209,#28210,#28211,#28212,#28213,#28214,#28215,
#28216,#28217,#28218,#28219,#28220,#28221,#28222,#28223,#28224,#28225,#28226,
#28227,#28228,#28229,#28230,#28231)),.UNSPECIFIED.,.F.,.F.,.F.)
B_SPLINE_SURFACE_WITH_KNOTS((2,2),(3,2,2,2,2,2,2,2,2,2,2,2,2,2,2,2,2,2,
2,2,2,2,2,2,2,2,2,2,2,2,2,2,2,2,2,2,2,2,2,2,2,2,2,2,2,2,2,2,2,2,2,2,2,2,
2,2,2,2,2,2,2,2,2,2,2,2,2,2,2,2,2,2,2,2,2,2,2,2,2,2,2,2,2,2,2,2,2,2,2,2,
2,2,2,2,2,2,2,2,2,2,2,2,2,2,2,2,2,2,2,2,2,2,2,2,2,2,2,2,2,2,2,2,2,2,2,2,
2,2,2,2,2,2,2,2,2,2,2,2,2,2,2,2,2,2,2,2,2,2,2,2,2,2,2,2,2,2,2,2,2,3),(0.,
1.00001332089208),(0.,0.00617283950617284,0.0123456790123457,0.0185185185185185,
0.0246913580246914,0.0308641975308642,0.037037037037037,0.0432098765432099,
0.0493827160493827,0.0555555555555556,0.0617283950617284,0.0679012345679012,
0.0740740740740741,0.0802469135802469,0.0864197530864197,0.0925925925925926,
0.0987654320987654,0.104938271604938,0.111111111111111,0.117283950617284,
0.123456790123457,0.12962962962963,0.135802469135802,0.141975308641975,
0.148148148148148,0.154320987654321,0.160493827160494,0.166666666666667,
0.172839506172839,0.179012345679012,0.185185185185185,0.191358024691358,
0.197530864197531,0.203703703703704,0.209876543209877,0.216049382716049,
0.222222222222222,0.228395061728395,0.234567901234568,0.240740740740741,
0.246913580246914,0.253086419753086,0.259259259259259,0.265432098765432,
0.271604938271605,0.277777777777778,0.283950617283951,0.290123456790123,
0.296296296296296,0.302469135802469,0.308641975308642,0.314814814814815,
0.320987654320988,0.327160493827161,0.333333333333333,0.339506172839506,
0.345679012345679,0.351851851851852,0.358024691358025,0.364197530864198,
0.37037037037037,0.376543209876543,0.382716049382716,0.388888888888889,
0.395061728395062,0.401234567901235,0.407407407407407,0.41358024691358,
0.419753086419753,0.425925925925926,0.432098765432099,0.438271604938272,
0.444444444444444,0.450617283950617,0.45679012345679,0.462962962962963,
0.469135802469136,0.475308641975309,0.481481481481481,0.487654320987654,
0.493827160493827,0.5,0.506172839506173,0.512345679012346,0.518518518518518,
0.524691358024691,0.530864197530864,0.537037037037037,0.54320987654321,
0.549382716049383,0.555555555555556,0.561728395061728,0.567901234567901,
0.574074074074074,0.580246913580247,0.58641975308642,0.592592592592593,
0.598765432098765,0.604938271604938,0.611111111111111,0.617283950617284,
0.623456790123457,0.62962962962963,0.635802469135803,0.641975308641975,
0.648148148148148,0.654320987654321,0.660493827160494,0.666666666666667,
0.672839506172839,0.679012345679012,0.685185185185185,0.691358024691358,
0.697530864197531,0.703703703703704,0.709876543209877,0.716049382716049,
0.722222222222222,0.728395061728395,0.734567901234568,0.740740740740741,
0.746913580246914,0.753086419753086,0.759259259259259,0.765432098765432,
0.771604938271605,0.777777777777778,0.783950617283951,0.790123456790123,
0.796296296296296,0.802469135802469,0.808641975308642,0.814814814814815,
0.820987654320988,0.827160493827161,0.833333333333333,0.839506172839506,
0.845679012345679,0.851851851851852,0.858024691358025,0.864197530864197,
0.87037037037037,0.876543209876543,0.882716049382716,0.888888888888889,
0.895061728395062,0.901234567901235,0.907407407407407,0.91358024691358,
0.919753086419753,0.925925925925926,0.932098765432099,0.938271604938272,
0.944444444444444,0.950617283950617,0.95679012345679,0.962962962962963,
0.969135802469136,0.975308641975309,0.977791440774828),.UNSPECIFIED.)
GEOMETRIC_REPRESENTATION_ITEM()
RATIONAL_B_SPLINE_SURFACE(((1.,0.866025403784439,1.,0.866025403784439,1.,
0.866025403784439,1.,0.866025403784439,1.,0.866025403784439,1.,0.866025403784439,
1.,0.866025403784439,1.,0.866025403784439,1.,0.866025403784439,1.,0.866025403784439,
1.,0.866025403784439,1.,0.866025403784439,1.,0.866025403784439,1.,0.866025403784439,
1.,0.866025403784439,1.,0.866025403784439,1.,0.866025403784439,1.,0.866025403784439,
1.,0.866025403784439,1.,0.866025403784439,1.,0.866025403784439,1.,0.866025403784439,
1.,0.866025403784439,1.,0.866025403784439,1.,0.866025403784439,1.,0.866025403784439,
1.,0.866025403784439,1.,0.866025403784439,1.,0.866025403784439,1.,0.866025403784439,
1.,0.866025403784439,1.,0.866025403784439,1.,0.866025403784439,1.,0.866025403784439,
1.,0.866025403784439,1.,0.866025403784439,1.,0.866025403784439,1.,0.866025403784439,
1.,0.866025403784439,1.,0.866025403784439,1.,0.866025403784439,1.,0.866025403784439,
1.,0.866025403784439,1.,0.866025403784439,1.,0.866025403784439,1.,0.866025403784439,
1.,0.866025403784439,1.,0.866025403784439,1.,0.866025403784439,1.,0.866025403784439,
1.,0.866025403784439,1.,0.866025403784439,1.,0.866025403784439,1.,0.866025403784439,
1.,0.866025403784439,1.,0.866025403784439,1.,0.866025403784439,1.,0.866025403784439,
1.,0.866025403784439,1.,0.866025403784439,1.,0.866025403784439,1.,0.866025403784439,
1.,0.866025403784439,1.,0.866025403784439,1.,0.866025403784439,1.,0.866025403784439,
1.,0.866025403784439,1.,0.866025403784439,1.,0.866025403784439,1.,0.866025403784439,
1.,0.866025403784439,1.,0.866025403784439,1.,0.866025403784439,1.,0.866025403784439,
1.,0.866025403784439,1.,0.866025403784439,1.,0.866025403784439,1.,0.866025403784439,
1.,0.866025403784439,1.,0.866025403784439,1.,0.866025403784439,1.,0.866025403784439,
1.,0.866025403784439,1.,0.866025403784439,1.,0.866025403784439,1.,0.866025403784439,
1.,0.866025403784439,1.,0.866025403784439,1.,0.866025403784439,1.,0.866025403784439,
1.,0.866025403784439,1.,0.866025403784439,1.,0.866025403784439,1.,0.866025403784439,
1.,0.866025403784439,1.,0.866025403784439,1.,0.866025403784439,1.,0.866025403784439,
1.,0.866025403784439,1.,0.866025403784439,1.,0.866025403784439,1.,0.866025403784439,
1.,0.866025403784439,1.,0.866025403784439,1.,0.866025403784439,1.,0.866025403784439,
1.,0.866025403784439,1.,0.866025403784439,1.,0.866025403784439,1.,0.866025403784439,
1.,0.866025403784439,1.,0.866025403784439,1.,0.866025403784439,1.,0.866025403784439,
1.,0.866025403784439,1.,0.866025403784439,1.,0.866025403784439,1.,0.866025403784439,
1.,0.866025403784439,1.,0.866025403784439,1.,0.866025403784439,1.,0.866025403784439,
1.,0.866025403784439,1.,0.866025403784439,1.,0.866025403784439,1.,0.866025403784439,
1.,0.866025403784439,1.,0.866025403784439,1.,0.866025403784439,1.,0.866025403784439,
1.,0.866025403784439,1.,0.866025403784439,1.,0.866025403784439,1.,0.866025403784439,
1.,0.866025403784439,1.,0.866025403784439,1.,0.866025403784439,1.,0.866025403784439,
1.,0.866025403784439,1.,0.866025403784439,1.,0.866025403784439,1.,0.866025403784439,
1.,0.866025403784439,1.,0.866025403784439,1.,0.866025403784439,1.,0.866025403784439,
1.,0.866025403784439,1.,0.866025403784439,1.,0.866025403784439,1.,0.866025403784439,
1.,0.866025403784439,1.,0.866025403784439,1.,0.866025403784439,1.,0.866025403784439,
1.,0.866025403784439,1.,0.866025403784439,1.,0.866025403784439,1.,0.866025403784439,
1.,0.946113621402695,0.935574890499137),(1.,0.866025403784439,1.,0.866025403784439,
1.,0.866025403784439,1.,0.866025403784439,1.,0.866025403784439,1.,0.866025403784439,
1.,0.866025403784439,1.,0.866025403784439,1.,0.866025403784439,1.,0.866025403784439,
1.,0.866025403784439,1.,0.866025403784439,1.,0.866025403784439,1.,0.866025403784439,
1.,0.866025403784439,1.,0.866025403784439,1.,0.866025403784439,1.,0.866025403784439,
1.,0.866025403784439,1.,0.866025403784439,1.,0.866025403784439,1.,0.866025403784439,
1.,0.866025403784439,1.,0.866025403784439,1.,0.866025403784439,1.,0.866025403784439,
1.,0.866025403784439,1.,0.866025403784439,1.,0.866025403784439,1.,0.866025403784439,
1.,0.866025403784439,1.,0.866025403784439,1.,0.866025403784439,1.,0.866025403784439,
1.,0.866025403784439,1.,0.866025403784439,1.,0.866025403784439,1.,0.866025403784439,
1.,0.866025403784439,1.,0.866025403784439,1.,0.866025403784439,1.,0.866025403784439,
1.,0.866025403784439,1.,0.866025403784439,1.,0.866025403784439,1.,0.866025403784439,
1.,0.866025403784439,1.,0.866025403784439,1.,0.866025403784439,1.,0.866025403784439,
1.,0.866025403784439,1.,0.866025403784439,1.,0.866025403784439,1.,0.866025403784439,
1.,0.866025403784439,1.,0.866025403784439,1.,0.866025403784439,1.,0.866025403784439,
1.,0.866025403784439,1.,0.866025403784439,1.,0.866025403784439,1.,0.866025403784439,
1.,0.866025403784439,1.,0.866025403784439,1.,0.866025403784439,1.,0.866025403784439,
1.,0.866025403784439,1.,0.866025403784439,1.,0.866025403784439,1.,0.866025403784439,
1.,0.866025403784439,1.,0.866025403784439,1.,0.866025403784439,1.,0.866025403784439,
1.,0.866025403784439,1.,0.866025403784439,1.,0.866025403784439,1.,0.866025403784439,
1.,0.866025403784439,1.,0.866025403784439,1.,0.866025403784439,1.,0.866025403784439,
1.,0.866025403784439,1.,0.866025403784439,1.,0.866025403784439,1.,0.866025403784439,
1.,0.866025403784439,1.,0.866025403784439,1.,0.866025403784439,1.,0.866025403784439,
1.,0.866025403784439,1.,0.866025403784439,1.,0.866025403784439,1.,0.866025403784439,
1.,0.866025403784439,1.,0.866025403784439,1.,0.866025403784439,1.,0.866025403784439,
1.,0.866025403784439,1.,0.866025403784439,1.,0.866025403784439,1.,0.866025403784439,
1.,0.866025403784439,1.,0.866025403784439,1.,0.866025403784439,1.,0.866025403784439,
1.,0.866025403784439,1.,0.866025403784439,1.,0.866025403784439,1.,0.866025403784439,
1.,0.866025403784439,1.,0.866025403784439,1.,0.866025403784439,1.,0.866025403784439,
1.,0.866025403784439,1.,0.866025403784439,1.,0.866025403784439,1.,0.866025403784439,
1.,0.866025403784439,1.,0.866025403784439,1.,0.866025403784439,1.,0.866025403784439,
1.,0.866025403784439,1.,0.866025403784439,1.,0.866025403784439,1.,0.866025403784439,
1.,0.866025403784439,1.,0.866025403784439,1.,0.866025403784439,1.,0.866025403784439,
1.,0.866025403784439,1.,0.866025403784439,1.,0.866025403784439,1.,0.866025403784439,
1.,0.866025403784439,1.,0.866025403784439,1.,0.866025403784439,1.,0.866025403784439,
1.,0.866025403784439,1.,0.866025403784439,1.,0.866025403784439,1.,0.866025403784439,
1.,0.866025403784439,1.,0.866025403784439,1.,0.866025403784439,1.,0.866025403784439,
1.,0.866025403784439,1.,0.866025403784439,1.,0.866025403784439,1.,0.866025403784439,
1.,0.866025403784439,1.,0.866025403784439,1.,0.866025403784439,1.,0.866025403784439,
1.,0.866025403784439,1.,0.866025403784439,1.,0.866025403784439,1.,0.866025403784439,
1.,0.946113621402695,0.935574890499137)))
REPRESENTATION_ITEM('')
SURFACE()
);
#294=(
BOUNDED_SURFACE()
B_SPLINE_SURFACE(1,2,((#28537,#28538,#28539,#28540,#28541,#28542,#28543,
#28544,#28545,#28546,#28547,#28548,#28549,#28550,#28551,#28552,#28553,#28554,
#28555,#28556,#28557,#28558,#28559,#28560,#28561,#28562,#28563,#28564,#28565,
#28566,#28567,#28568,#28569,#28570,#28571,#28572,#28573,#28574,#28575,#28576,
#28577,#28578,#28579,#28580,#28581,#28582,#28583,#28584,#28585,#28586,#28587,
#28588,#28589,#28590,#28591,#28592,#28593,#28594,#28595,#28596,#28597,#28598,
#28599,#28600,#28601,#28602,#28603,#28604,#28605,#28606,#28607,#28608,#28609,
#28610,#28611,#28612,#28613,#28614,#28615,#28616,#28617,#28618,#28619,#28620,
#28621,#28622,#28623,#28624,#28625,#28626,#28627,#28628,#28629,#28630,#28631,
#28632,#28633,#28634,#28635,#28636,#28637,#28638,#28639,#28640,#28641,#28642,
#28643,#28644,#28645,#28646,#28647,#28648,#28649,#28650,#28651,#28652,#28653,
#28654,#28655,#28656,#28657,#28658,#28659,#28660,#28661,#28662,#28663,#28664,
#28665,#28666,#28667,#28668,#28669,#28670,#28671,#28672,#28673,#28674,#28675,
#28676,#28677,#28678,#28679,#28680,#28681,#28682,#28683,#28684,#28685,#28686,
#28687,#28688,#28689,#28690,#28691,#28692,#28693,#28694,#28695,#28696,#28697,
#28698,#28699,#28700,#28701,#28702,#28703,#28704,#28705,#28706,#28707,#28708,
#28709,#28710,#28711,#28712,#28713,#28714,#28715,#28716,#28717,#28718,#28719,
#28720,#28721,#28722,#28723,#28724,#28725,#28726,#28727,#28728,#28729,#28730,
#28731,#28732,#28733,#28734,#28735,#28736,#28737,#28738,#28739,#28740,#28741,
#28742,#28743,#28744,#28745,#28746,#28747,#28748,#28749,#28750,#28751,#28752,
#28753,#28754,#28755,#28756,#28757,#28758,#28759,#28760,#28761,#28762,#28763,
#28764,#28765,#28766,#28767,#28768,#28769,#28770,#28771,#28772,#28773,#28774,
#28775,#28776,#28777,#28778,#28779,#28780,#28781,#28782,#28783,#28784,#28785,
#28786,#28787,#28788,#28789,#28790,#28791,#28792,#28793,#28794,#28795,#28796,
#28797,#28798,#28799,#28800,#28801,#28802,#28803,#28804,#28805,#28806,#28807,
#28808,#28809,#28810,#28811,#28812,#28813,#28814,#28815,#28816,#28817,#28818,
#28819,#28820,#28821,#28822,#28823,#28824,#28825,#28826,#28827,#28828,#28829,
#28830,#28831,#28832,#28833,#28834,#28835,#28836,#28837,#28838,#28839,#28840,
#28841,#28842,#28843,#28844,#28845,#28846,#28847,#28848,#28849,#28850,#28851,
#28852,#28853,#28854,#28855,#28856,#28857),(#28858,#28859,#28860,#28861,
#28862,#28863,#28864,#28865,#28866,#28867,#28868,#28869,#28870,#28871,#28872,
#28873,#28874,#28875,#28876,#28877,#28878,#28879,#28880,#28881,#28882,#28883,
#28884,#28885,#28886,#28887,#28888,#28889,#28890,#28891,#28892,#28893,#28894,
#28895,#28896,#28897,#28898,#28899,#28900,#28901,#28902,#28903,#28904,#28905,
#28906,#28907,#28908,#28909,#28910,#28911,#28912,#28913,#28914,#28915,#28916,
#28917,#28918,#28919,#28920,#28921,#28922,#28923,#28924,#28925,#28926,#28927,
#28928,#28929,#28930,#28931,#28932,#28933,#28934,#28935,#28936,#28937,#28938,
#28939,#28940,#28941,#28942,#28943,#28944,#28945,#28946,#28947,#28948,#28949,
#28950,#28951,#28952,#28953,#28954,#28955,#28956,#28957,#28958,#28959,#28960,
#28961,#28962,#28963,#28964,#28965,#28966,#28967,#28968,#28969,#28970,#28971,
#28972,#28973,#28974,#28975,#28976,#28977,#28978,#28979,#28980,#28981,#28982,
#28983,#28984,#28985,#28986,#28987,#28988,#28989,#28990,#28991,#28992,#28993,
#28994,#28995,#28996,#28997,#28998,#28999,#29000,#29001,#29002,#29003,#29004,
#29005,#29006,#29007,#29008,#29009,#29010,#29011,#29012,#29013,#29014,#29015,
#29016,#29017,#29018,#29019,#29020,#29021,#29022,#29023,#29024,#29025,#29026,
#29027,#29028,#29029,#29030,#29031,#29032,#29033,#29034,#29035,#29036,#29037,
#29038,#29039,#29040,#29041,#29042,#29043,#29044,#29045,#29046,#29047,#29048,
#29049,#29050,#29051,#29052,#29053,#29054,#29055,#29056,#29057,#29058,#29059,
#29060,#29061,#29062,#29063,#29064,#29065,#29066,#29067,#29068,#29069,#29070,
#29071,#29072,#29073,#29074,#29075,#29076,#29077,#29078,#29079,#29080,#29081,
#29082,#29083,#29084,#29085,#29086,#29087,#29088,#29089,#29090,#29091,#29092,
#29093,#29094,#29095,#29096,#29097,#29098,#29099,#29100,#29101,#29102,#29103,
#29104,#29105,#29106,#29107,#29108,#29109,#29110,#29111,#29112,#29113,#29114,
#29115,#29116,#29117,#29118,#29119,#29120,#29121,#29122,#29123,#29124,#29125,
#29126,#29127,#29128,#29129,#29130,#29131,#29132,#29133,#29134,#29135,#29136,
#29137,#29138,#29139,#29140,#29141,#29142,#29143,#29144,#29145,#29146,#29147,
#29148,#29149,#29150,#29151,#29152,#29153,#29154,#29155,#29156,#29157,#29158,
#29159,#29160,#29161,#29162,#29163,#29164,#29165,#29166,#29167,#29168,#29169,
#29170,#29171,#29172,#29173,#29174,#29175,#29176,#29177,#29178)),
 .UNSPECIFIED.,.F.,.F.,.F.)
B_SPLINE_SURFACE_WITH_KNOTS((2,2),(3,2,2,2,2,2,2,2,2,2,2,2,2,2,2,2,2,2,
2,2,2,2,2,2,2,2,2,2,2,2,2,2,2,2,2,2,2,2,2,2,2,2,2,2,2,2,2,2,2,2,2,2,2,2,
2,2,2,2,2,2,2,2,2,2,2,2,2,2,2,2,2,2,2,2,2,2,2,2,2,2,2,2,2,2,2,2,2,2,2,2,
2,2,2,2,2,2,2,2,2,2,2,2,2,2,2,2,2,2,2,2,2,2,2,2,2,2,2,2,2,2,2,2,2,2,2,2,
2,2,2,2,2,2,2,2,2,2,2,2,2,2,2,2,2,2,2,2,2,2,2,2,2,2,2,2,2,2,2,2,2,2,3),
(-0.000321975171239186,1.),(0.,0.00617283950617284,0.0123456790123457,0.0185185185185185,
0.0246913580246914,0.0308641975308642,0.037037037037037,0.0432098765432099,
0.0493827160493827,0.0555555555555556,0.0617283950617284,0.0679012345679012,
0.0740740740740741,0.0802469135802469,0.0864197530864197,0.0925925925925926,
0.0987654320987654,0.104938271604938,0.111111111111111,0.117283950617284,
0.123456790123457,0.12962962962963,0.135802469135802,0.141975308641975,
0.148148148148148,0.154320987654321,0.160493827160494,0.166666666666667,
0.172839506172839,0.179012345679012,0.185185185185185,0.191358024691358,
0.197530864197531,0.203703703703704,0.209876543209877,0.216049382716049,
0.222222222222222,0.228395061728395,0.234567901234568,0.240740740740741,
0.246913580246914,0.253086419753086,0.259259259259259,0.265432098765432,
0.271604938271605,0.277777777777778,0.283950617283951,0.290123456790123,
0.296296296296296,0.302469135802469,0.308641975308642,0.314814814814815,
0.320987654320988,0.327160493827161,0.333333333333333,0.339506172839506,
0.345679012345679,0.351851851851852,0.358024691358025,0.364197530864198,
0.37037037037037,0.376543209876543,0.382716049382716,0.388888888888889,
0.395061728395062,0.401234567901235,0.407407407407407,0.41358024691358,
0.419753086419753,0.425925925925926,0.432098765432099,0.438271604938272,
0.444444444444444,0.450617283950617,0.45679012345679,0.462962962962963,
0.469135802469136,0.475308641975309,0.481481481481481,0.487654320987654,
0.493827160493827,0.5,0.506172839506173,0.512345679012346,0.518518518518518,
0.524691358024691,0.530864197530864,0.537037037037037,0.54320987654321,
0.549382716049383,0.555555555555556,0.561728395061728,0.567901234567901,
0.574074074074074,0.580246913580247,0.58641975308642,0.592592592592593,
0.598765432098765,0.604938271604938,0.611111111111111,0.617283950617284,
0.623456790123457,0.62962962962963,0.635802469135803,0.641975308641975,
0.648148148148148,0.654320987654321,0.660493827160494,0.666666666666667,
0.672839506172839,0.679012345679012,0.685185185185185,0.691358024691358,
0.697530864197531,0.703703703703704,0.709876543209877,0.716049382716049,
0.722222222222222,0.728395061728395,0.734567901234568,0.740740740740741,
0.746913580246914,0.753086419753086,0.759259259259259,0.765432098765432,
0.771604938271605,0.777777777777778,0.783950617283951,0.790123456790123,
0.796296296296296,0.802469135802469,0.808641975308642,0.814814814814815,
0.820987654320988,0.827160493827161,0.833333333333333,0.839506172839506,
0.845679012345679,0.851851851851852,0.858024691358025,0.864197530864197,
0.87037037037037,0.876543209876543,0.882716049382716,0.888888888888889,
0.895061728395062,0.901234567901235,0.907407407407407,0.91358024691358,
0.919753086419753,0.925925925925926,0.932098765432099,0.938271604938272,
0.944444444444444,0.950617283950617,0.95679012345679,0.962962962962963,
0.969135802469136,0.975308641975309,0.977791393533952,0.987569307469292),
 .UNSPECIFIED.)
GEOMETRIC_REPRESENTATION_ITEM()
RATIONAL_B_SPLINE_SURFACE(((1.,0.866025403784439,1.,0.866025403784439,1.,
0.866025403784439,1.,0.866025403784439,1.,0.866025403784439,1.,0.866025403784439,
1.,0.866025403784439,1.,0.866025403784439,1.,0.866025403784439,1.,0.866025403784439,
1.,0.866025403784439,1.,0.866025403784439,1.,0.866025403784439,1.,0.866025403784439,
1.,0.866025403784439,1.,0.866025403784439,1.,0.866025403784439,1.,0.866025403784439,
1.,0.866025403784439,1.,0.866025403784439,1.,0.866025403784439,1.,0.866025403784439,
1.,0.866025403784439,1.,0.866025403784439,1.,0.866025403784439,1.,0.866025403784439,
1.,0.866025403784439,1.,0.866025403784439,1.,0.866025403784439,1.,0.866025403784439,
1.,0.866025403784439,1.,0.866025403784439,1.,0.866025403784439,1.,0.866025403784439,
1.,0.866025403784439,1.,0.866025403784439,1.,0.866025403784439,1.,0.866025403784439,
1.,0.866025403784439,1.,0.866025403784439,1.,0.866025403784439,1.,0.866025403784439,
1.,0.866025403784439,1.,0.866025403784439,1.,0.866025403784439,1.,0.866025403784439,
1.,0.866025403784439,1.,0.866025403784439,1.,0.866025403784439,1.,0.866025403784439,
1.,0.866025403784439,1.,0.866025403784439,1.,0.866025403784439,1.,0.866025403784439,
1.,0.866025403784439,1.,0.866025403784439,1.,0.866025403784439,1.,0.866025403784439,
1.,0.866025403784439,1.,0.866025403784439,1.,0.866025403784439,1.,0.866025403784439,
1.,0.866025403784439,1.,0.866025403784439,1.,0.866025403784439,1.,0.866025403784439,
1.,0.866025403784439,1.,0.866025403784439,1.,0.866025403784439,1.,0.866025403784439,
1.,0.866025403784439,1.,0.866025403784439,1.,0.866025403784439,1.,0.866025403784439,
1.,0.866025403784439,1.,0.866025403784439,1.,0.866025403784439,1.,0.866025403784439,
1.,0.866025403784439,1.,0.866025403784439,1.,0.866025403784439,1.,0.866025403784439,
1.,0.866025403784439,1.,0.866025403784439,1.,0.866025403784439,1.,0.866025403784439,
1.,0.866025403784439,1.,0.866025403784439,1.,0.866025403784439,1.,0.866025403784439,
1.,0.866025403784439,1.,0.866025403784439,1.,0.866025403784439,1.,0.866025403784439,
1.,0.866025403784439,1.,0.866025403784439,1.,0.866025403784439,1.,0.866025403784439,
1.,0.866025403784439,1.,0.866025403784439,1.,0.866025403784439,1.,0.866025403784439,
1.,0.866025403784439,1.,0.866025403784439,1.,0.866025403784439,1.,0.866025403784439,
1.,0.866025403784439,1.,0.866025403784439,1.,0.866025403784439,1.,0.866025403784439,
1.,0.866025403784439,1.,0.866025403784439,1.,0.866025403784439,1.,0.866025403784439,
1.,0.866025403784439,1.,0.866025403784439,1.,0.866025403784439,1.,0.866025403784439,
1.,0.866025403784439,1.,0.866025403784439,1.,0.866025403784439,1.,0.866025403784439,
1.,0.866025403784439,1.,0.866025403784439,1.,0.866025403784439,1.,0.866025403784439,
1.,0.866025403784439,1.,0.866025403784439,1.,0.866025403784439,1.,0.866025403784439,
1.,0.866025403784439,1.,0.866025403784439,1.,0.866025403784439,1.,0.866025403784439,
1.,0.866025403784439,1.,0.866025403784439,1.,0.866025403784439,1.,0.866025403784439,
1.,0.866025403784439,1.,0.866025403784439,1.,0.866025403784439,1.,0.866025403784439,
1.,0.866025403784439,1.,0.866025403784439,1.,0.866025403784439,1.,0.866025403784439,
1.,0.866025403784439,1.,0.866025403784439,1.,0.866025403784439,1.,0.866025403784439,
1.,0.866025403784439,1.,0.866025403784439,1.,0.866025403784439,1.,0.866025403784439,
1.,0.866025403784439,1.,0.866025403784439,1.,0.866025403784439,1.,0.866025403784439,
1.,0.946114646713198,0.93557529156132,0.93557529156132,0.93557529156132),
(1.,0.866025403784439,1.,0.866025403784439,1.,0.866025403784439,1.,0.866025403784439,
1.,0.866025403784439,1.,0.866025403784439,1.,0.866025403784439,1.,0.866025403784439,
1.,0.866025403784439,1.,0.866025403784439,1.,0.866025403784439,1.,0.866025403784439,
1.,0.866025403784439,1.,0.866025403784439,1.,0.866025403784439,1.,0.866025403784439,
1.,0.866025403784439,1.,0.866025403784439,1.,0.866025403784439,1.,0.866025403784439,
1.,0.866025403784439,1.,0.866025403784439,1.,0.866025403784439,1.,0.866025403784439,
1.,0.866025403784439,1.,0.866025403784439,1.,0.866025403784439,1.,0.866025403784439,
1.,0.866025403784439,1.,0.866025403784439,1.,0.866025403784439,1.,0.866025403784439,
1.,0.866025403784439,1.,0.866025403784439,1.,0.866025403784439,1.,0.866025403784439,
1.,0.866025403784439,1.,0.866025403784439,1.,0.866025403784439,1.,0.866025403784439,
1.,0.866025403784439,1.,0.866025403784439,1.,0.866025403784439,1.,0.866025403784439,
1.,0.866025403784439,1.,0.866025403784439,1.,0.866025403784439,1.,0.866025403784439,
1.,0.866025403784439,1.,0.866025403784439,1.,0.866025403784439,1.,0.866025403784439,
1.,0.866025403784439,1.,0.866025403784439,1.,0.866025403784439,1.,0.866025403784439,
1.,0.866025403784439,1.,0.866025403784439,1.,0.866025403784439,1.,0.866025403784439,
1.,0.866025403784439,1.,0.866025403784439,1.,0.866025403784439,1.,0.866025403784439,
1.,0.866025403784439,1.,0.866025403784439,1.,0.866025403784439,1.,0.866025403784439,
1.,0.866025403784439,1.,0.866025403784439,1.,0.866025403784439,1.,0.866025403784439,
1.,0.866025403784439,1.,0.866025403784439,1.,0.866025403784439,1.,0.866025403784439,
1.,0.866025403784439,1.,0.866025403784439,1.,0.866025403784439,1.,0.866025403784439,
1.,0.866025403784439,1.,0.866025403784439,1.,0.866025403784439,1.,0.866025403784439,
1.,0.866025403784439,1.,0.866025403784439,1.,0.866025403784439,1.,0.866025403784439,
1.,0.866025403784439,1.,0.866025403784439,1.,0.866025403784439,1.,0.866025403784439,
1.,0.866025403784439,1.,0.866025403784439,1.,0.866025403784439,1.,0.866025403784439,
1.,0.866025403784439,1.,0.866025403784439,1.,0.866025403784439,1.,0.866025403784439,
1.,0.866025403784439,1.,0.866025403784439,1.,0.866025403784439,1.,0.866025403784439,
1.,0.866025403784439,1.,0.866025403784439,1.,0.866025403784439,1.,0.866025403784439,
1.,0.866025403784439,1.,0.866025403784439,1.,0.866025403784439,1.,0.866025403784439,
1.,0.866025403784439,1.,0.866025403784439,1.,0.866025403784439,1.,0.866025403784439,
1.,0.866025403784439,1.,0.866025403784439,1.,0.866025403784439,1.,0.866025403784439,
1.,0.866025403784439,1.,0.866025403784439,1.,0.866025403784439,1.,0.866025403784439,
1.,0.866025403784439,1.,0.866025403784439,1.,0.866025403784439,1.,0.866025403784439,
1.,0.866025403784439,1.,0.866025403784439,1.,0.866025403784439,1.,0.866025403784439,
1.,0.866025403784439,1.,0.866025403784439,1.,0.866025403784439,1.,0.866025403784439,
1.,0.866025403784439,1.,0.866025403784439,1.,0.866025403784439,1.,0.866025403784439,
1.,0.866025403784439,1.,0.866025403784439,1.,0.866025403784439,1.,0.866025403784439,
1.,0.866025403784439,1.,0.866025403784439,1.,0.866025403784439,1.,0.866025403784439,
1.,0.866025403784439,1.,0.866025403784439,1.,0.866025403784439,1.,0.866025403784439,
1.,0.866025403784439,1.,0.866025403784439,1.,0.866025403784439,1.,0.866025403784439,
1.,0.866025403784439,1.,0.866025403784439,1.,0.946114646713198,0.93557529156132,
0.93557529156132,0.93557529156132)))
REPRESENTATION_ITEM('')
SURFACE()
);
#295=(
BOUNDED_SURFACE()
B_SPLINE_SURFACE(1,2,((#29179,#29180,#29181,#29182,#29183,#29184,#29185,
#29186,#29187,#29188,#29189,#29190,#29191,#29192,#29193,#29194,#29195,#29196,
#29197,#29198,#29199,#29200,#29201,#29202,#29203,#29204,#29205,#29206,#29207,
#29208,#29209,#29210,#29211,#29212,#29213,#29214,#29215,#29216,#29217,#29218,
#29219,#29220,#29221,#29222,#29223,#29224,#29225,#29226,#29227,#29228,#29229,
#29230,#29231,#29232,#29233,#29234,#29235,#29236,#29237,#29238,#29239,#29240,
#29241,#29242,#29243,#29244,#29245,#29246,#29247,#29248,#29249,#29250,#29251,
#29252,#29253,#29254,#29255,#29256,#29257,#29258,#29259,#29260,#29261,#29262,
#29263,#29264,#29265,#29266,#29267,#29268,#29269,#29270,#29271,#29272,#29273,
#29274,#29275,#29276,#29277,#29278,#29279,#29280,#29281,#29282,#29283,#29284,
#29285,#29286,#29287,#29288,#29289,#29290,#29291,#29292,#29293,#29294,#29295,
#29296,#29297,#29298,#29299,#29300,#29301,#29302,#29303,#29304,#29305,#29306,
#29307,#29308,#29309,#29310,#29311,#29312,#29313,#29314,#29315,#29316,#29317,
#29318,#29319,#29320,#29321,#29322,#29323,#29324,#29325,#29326,#29327,#29328,
#29329,#29330,#29331,#29332,#29333,#29334,#29335,#29336,#29337,#29338,#29339,
#29340,#29341,#29342,#29343,#29344,#29345,#29346,#29347,#29348,#29349,#29350,
#29351,#29352,#29353,#29354,#29355,#29356,#29357,#29358,#29359,#29360,#29361,
#29362,#29363,#29364,#29365,#29366,#29367,#29368,#29369,#29370,#29371,#29372,
#29373,#29374,#29375,#29376,#29377,#29378,#29379,#29380,#29381,#29382,#29383,
#29384,#29385,#29386,#29387,#29388,#29389,#29390,#29391,#29392,#29393,#29394,
#29395,#29396,#29397,#29398,#29399,#29400,#29401,#29402,#29403,#29404,#29405,
#29406,#29407,#29408,#29409,#29410,#29411,#29412,#29413,#29414,#29415,#29416,
#29417,#29418,#29419,#29420,#29421,#29422,#29423,#29424,#29425,#29426,#29427,
#29428,#29429,#29430,#29431,#29432,#29433,#29434,#29435,#29436,#29437,#29438,
#29439,#29440,#29441,#29442,#29443,#29444,#29445,#29446,#29447,#29448,#29449,
#29450,#29451,#29452,#29453,#29454,#29455,#29456,#29457,#29458,#29459,#29460,
#29461,#29462,#29463,#29464,#29465,#29466,#29467,#29468,#29469,#29470,#29471,
#29472,#29473,#29474,#29475,#29476,#29477,#29478,#29479,#29480,#29481,#29482,
#29483,#29484,#29485,#29486,#29487,#29488,#29489,#29490,#29491,#29492,#29493,
#29494,#29495,#29496,#29497),(#29498,#29499,#29500,#29501,#29502,#29503,
#29504,#29505,#29506,#29507,#29508,#29509,#29510,#29511,#29512,#29513,#29514,
#29515,#29516,#29517,#29518,#29519,#29520,#29521,#29522,#29523,#29524,#29525,
#29526,#29527,#29528,#29529,#29530,#29531,#29532,#29533,#29534,#29535,#29536,
#29537,#29538,#29539,#29540,#29541,#29542,#29543,#29544,#29545,#29546,#29547,
#29548,#29549,#29550,#29551,#29552,#29553,#29554,#29555,#29556,#29557,#29558,
#29559,#29560,#29561,#29562,#29563,#29564,#29565,#29566,#29567,#29568,#29569,
#29570,#29571,#29572,#29573,#29574,#29575,#29576,#29577,#29578,#29579,#29580,
#29581,#29582,#29583,#29584,#29585,#29586,#29587,#29588,#29589,#29590,#29591,
#29592,#29593,#29594,#29595,#29596,#29597,#29598,#29599,#29600,#29601,#29602,
#29603,#29604,#29605,#29606,#29607,#29608,#29609,#29610,#29611,#29612,#29613,
#29614,#29615,#29616,#29617,#29618,#29619,#29620,#29621,#29622,#29623,#29624,
#29625,#29626,#29627,#29628,#29629,#29630,#29631,#29632,#29633,#29634,#29635,
#29636,#29637,#29638,#29639,#29640,#29641,#29642,#29643,#29644,#29645,#29646,
#29647,#29648,#29649,#29650,#29651,#29652,#29653,#29654,#29655,#29656,#29657,
#29658,#29659,#29660,#29661,#29662,#29663,#29664,#29665,#29666,#29667,#29668,
#29669,#29670,#29671,#29672,#29673,#29674,#29675,#29676,#29677,#29678,#29679,
#29680,#29681,#29682,#29683,#29684,#29685,#29686,#29687,#29688,#29689,#29690,
#29691,#29692,#29693,#29694,#29695,#29696,#29697,#29698,#29699,#29700,#29701,
#29702,#29703,#29704,#29705,#29706,#29707,#29708,#29709,#29710,#29711,#29712,
#29713,#29714,#29715,#29716,#29717,#29718,#29719,#29720,#29721,#29722,#29723,
#29724,#29725,#29726,#29727,#29728,#29729,#29730,#29731,#29732,#29733,#29734,
#29735,#29736,#29737,#29738,#29739,#29740,#29741,#29742,#29743,#29744,#29745,
#29746,#29747,#29748,#29749,#29750,#29751,#29752,#29753,#29754,#29755,#29756,
#29757,#29758,#29759,#29760,#29761,#29762,#29763,#29764,#29765,#29766,#29767,
#29768,#29769,#29770,#29771,#29772,#29773,#29774,#29775,#29776,#29777,#29778,
#29779,#29780,#29781,#29782,#29783,#29784,#29785,#29786,#29787,#29788,#29789,
#29790,#29791,#29792,#29793,#29794,#29795,#29796,#29797,#29798,#29799,#29800,
#29801,#29802,#29803,#29804,#29805,#29806,#29807,#29808,#29809,#29810,#29811,
#29812,#29813,#29814,#29815,#29816)),.UNSPECIFIED.,.F.,.F.,.F.)
B_SPLINE_SURFACE_WITH_KNOTS((2,2),(3,2,2,2,2,2,2,2,2,2,2,2,2,2,2,2,2,2,
2,2,2,2,2,2,2,2,2,2,2,2,2,2,2,2,2,2,2,2,2,2,2,2,2,2,2,2,2,2,2,2,2,2,2,2,
2,2,2,2,2,2,2,2,2,2,2,2,2,2,2,2,2,2,2,2,2,2,2,2,2,2,2,2,2,2,2,2,2,2,2,2,
2,2,2,2,2,2,2,2,2,2,2,2,2,2,2,2,2,2,2,2,2,2,2,2,2,2,2,2,2,2,2,2,2,2,2,2,
2,2,2,2,2,2,2,2,2,2,2,2,2,2,2,2,2,2,2,2,2,2,2,2,2,2,2,2,2,2,2,2,2,3),(-2.4733869132694E-5,
1.),(0.,0.00617283950617284,0.0123456790123457,0.0185185185185185,0.0246913580246914,
0.0308641975308642,0.037037037037037,0.0432098765432099,0.0493827160493827,
0.0555555555555556,0.0617283950617284,0.0679012345679012,0.0740740740740741,
0.0802469135802469,0.0864197530864197,0.0925925925925926,0.0987654320987654,
0.104938271604938,0.111111111111111,0.117283950617284,0.123456790123457,
0.12962962962963,0.135802469135802,0.141975308641975,0.148148148148148,
0.154320987654321,0.160493827160494,0.166666666666667,0.172839506172839,
0.179012345679012,0.185185185185185,0.191358024691358,0.197530864197531,
0.203703703703704,0.209876543209877,0.216049382716049,0.222222222222222,
0.228395061728395,0.234567901234568,0.240740740740741,0.246913580246914,
0.253086419753086,0.259259259259259,0.265432098765432,0.271604938271605,
0.277777777777778,0.283950617283951,0.290123456790123,0.296296296296296,
0.302469135802469,0.308641975308642,0.314814814814815,0.320987654320988,
0.327160493827161,0.333333333333333,0.339506172839506,0.345679012345679,
0.351851851851852,0.358024691358025,0.364197530864198,0.37037037037037,
0.376543209876543,0.382716049382716,0.388888888888889,0.395061728395062,
0.401234567901235,0.407407407407407,0.41358024691358,0.419753086419753,
0.425925925925926,0.432098765432099,0.438271604938272,0.444444444444444,
0.450617283950617,0.45679012345679,0.462962962962963,0.469135802469136,
0.475308641975309,0.481481481481481,0.487654320987654,0.493827160493827,
0.5,0.506172839506173,0.512345679012346,0.518518518518518,0.524691358024691,
0.530864197530864,0.537037037037037,0.54320987654321,0.549382716049383,
0.555555555555556,0.561728395061728,0.567901234567901,0.574074074074074,
0.580246913580247,0.58641975308642,0.592592592592593,0.598765432098765,
0.604938271604938,0.611111111111111,0.617283950617284,0.623456790123457,
0.62962962962963,0.635802469135803,0.641975308641975,0.648148148148148,
0.654320987654321,0.660493827160494,0.666666666666667,0.672839506172839,
0.679012345679012,0.685185185185185,0.691358024691358,0.697530864197531,
0.703703703703704,0.709876543209877,0.716049382716049,0.722222222222222,
0.728395061728395,0.734567901234568,0.740740740740741,0.746913580246914,
0.753086419753086,0.759259259259259,0.765432098765432,0.771604938271605,
0.777777777777778,0.783950617283951,0.790123456790123,0.796296296296296,
0.802469135802469,0.808641975308642,0.814814814814815,0.820987654320988,
0.827160493827161,0.833333333333333,0.839506172839506,0.845679012345679,
0.851851851851852,0.858024691358025,0.864197530864197,0.87037037037037,
0.876543209876543,0.882716049382716,0.888888888888889,0.895061728395062,
0.901234567901235,0.907407407407407,0.91358024691358,0.919753086419753,
0.925925925925926,0.932098765432099,0.938271604938272,0.944444444444444,
0.950617283950617,0.95679012345679,0.962962962962963,0.969135802469136,
0.975308641975309,0.977791447664447),.UNSPECIFIED.)
GEOMETRIC_REPRESENTATION_ITEM()
RATIONAL_B_SPLINE_SURFACE(((1.,0.866025403784439,1.,0.866025403784439,1.,
0.866025403784439,1.,0.866025403784439,1.,0.866025403784439,1.,0.866025403784439,
1.,0.866025403784439,1.,0.866025403784439,1.,0.866025403784439,1.,0.866025403784439,
1.,0.866025403784439,1.,0.866025403784439,1.,0.866025403784439,1.,0.866025403784439,
1.,0.866025403784439,1.,0.866025403784439,1.,0.866025403784439,1.,0.866025403784439,
1.,0.866025403784439,1.,0.866025403784439,1.,0.866025403784439,1.,0.866025403784439,
1.,0.866025403784439,1.,0.866025403784439,1.,0.866025403784439,1.,0.866025403784439,
1.,0.866025403784439,1.,0.866025403784439,1.,0.866025403784439,1.,0.866025403784439,
1.,0.866025403784439,1.,0.866025403784439,1.,0.866025403784439,1.,0.866025403784439,
1.,0.866025403784439,1.,0.866025403784439,1.,0.866025403784439,1.,0.866025403784439,
1.,0.866025403784439,1.,0.866025403784439,1.,0.866025403784439,1.,0.866025403784439,
1.,0.866025403784439,1.,0.866025403784439,1.,0.866025403784439,1.,0.866025403784439,
1.,0.866025403784439,1.,0.866025403784439,1.,0.866025403784439,1.,0.866025403784439,
1.,0.866025403784439,1.,0.866025403784439,1.,0.866025403784439,1.,0.866025403784439,
1.,0.866025403784439,1.,0.866025403784439,1.,0.866025403784439,1.,0.866025403784439,
1.,0.866025403784439,1.,0.866025403784439,1.,0.866025403784439,1.,0.866025403784439,
1.,0.866025403784439,1.,0.866025403784439,1.,0.866025403784439,1.,0.866025403784439,
1.,0.866025403784439,1.,0.866025403784439,1.,0.866025403784439,1.,0.866025403784439,
1.,0.866025403784439,1.,0.866025403784439,1.,0.866025403784439,1.,0.866025403784439,
1.,0.866025403784439,1.,0.866025403784439,1.,0.866025403784439,1.,0.866025403784439,
1.,0.866025403784439,1.,0.866025403784439,1.,0.866025403784439,1.,0.866025403784439,
1.,0.866025403784439,1.,0.866025403784439,1.,0.866025403784439,1.,0.866025403784439,
1.,0.866025403784439,1.,0.866025403784439,1.,0.866025403784439,1.,0.866025403784439,
1.,0.866025403784439,1.,0.866025403784439,1.,0.866025403784439,1.,0.866025403784439,
1.,0.866025403784439,1.,0.866025403784439,1.,0.866025403784439,1.,0.866025403784439,
1.,0.866025403784439,1.,0.866025403784439,1.,0.866025403784439,1.,0.866025403784439,
1.,0.866025403784439,1.,0.866025403784439,1.,0.866025403784439,1.,0.866025403784439,
1.,0.866025403784439,1.,0.866025403784439,1.,0.866025403784439,1.,0.866025403784439,
1.,0.866025403784439,1.,0.866025403784439,1.,0.866025403784439,1.,0.866025403784439,
1.,0.866025403784439,1.,0.866025403784439,1.,0.866025403784439,1.,0.866025403784439,
1.,0.866025403784439,1.,0.866025403784439,1.,0.866025403784439,1.,0.866025403784439,
1.,0.866025403784439,1.,0.866025403784439,1.,0.866025403784439,1.,0.866025403784439,
1.,0.866025403784439,1.,0.866025403784439,1.,0.866025403784439,1.,0.866025403784439,
1.,0.866025403784439,1.,0.866025403784439,1.,0.866025403784439,1.,0.866025403784439,
1.,0.866025403784439,1.,0.866025403784439,1.,0.866025403784439,1.,0.866025403784439,
1.,0.866025403784439,1.,0.866025403784439,1.,0.866025403784439,1.,0.866025403784439,
1.,0.866025403784439,1.,0.866025403784439,1.,0.866025403784439,1.,0.866025403784439,
1.,0.866025403784439,1.,0.866025403784439,1.,0.866025403784439,1.,0.866025403784439,
1.,0.866025403784439,1.,0.866025403784439,1.,0.866025403784439,1.,0.866025403784439,
1.,0.866025403784439,1.,0.866025403784439,1.,0.866025403784439,1.,0.866025403784439,
1.,0.9461134718712,0.935574832010768),(1.,0.866025403784439,1.,0.866025403784439,
1.,0.866025403784439,1.,0.866025403784439,1.,0.866025403784439,1.,0.866025403784439,
1.,0.866025403784439,1.,0.866025403784439,1.,0.866025403784439,1.,0.866025403784439,
1.,0.866025403784439,1.,0.866025403784439,1.,0.866025403784439,1.,0.866025403784439,
1.,0.866025403784439,1.,0.866025403784439,1.,0.866025403784439,1.,0.866025403784439,
1.,0.866025403784439,1.,0.866025403784439,1.,0.866025403784439,1.,0.866025403784439,
1.,0.866025403784439,1.,0.866025403784439,1.,0.866025403784439,1.,0.866025403784439,
1.,0.866025403784439,1.,0.866025403784439,1.,0.866025403784439,1.,0.866025403784439,
1.,0.866025403784439,1.,0.866025403784439,1.,0.866025403784439,1.,0.866025403784439,
1.,0.866025403784439,1.,0.866025403784439,1.,0.866025403784439,1.,0.866025403784439,
1.,0.866025403784439,1.,0.866025403784439,1.,0.866025403784439,1.,0.866025403784439,
1.,0.866025403784439,1.,0.866025403784439,1.,0.866025403784439,1.,0.866025403784439,
1.,0.866025403784439,1.,0.866025403784439,1.,0.866025403784439,1.,0.866025403784439,
1.,0.866025403784439,1.,0.866025403784439,1.,0.866025403784439,1.,0.866025403784439,
1.,0.866025403784439,1.,0.866025403784439,1.,0.866025403784439,1.,0.866025403784439,
1.,0.866025403784439,1.,0.866025403784439,1.,0.866025403784439,1.,0.866025403784439,
1.,0.866025403784439,1.,0.866025403784439,1.,0.866025403784439,1.,0.866025403784439,
1.,0.866025403784439,1.,0.866025403784439,1.,0.866025403784439,1.,0.866025403784439,
1.,0.866025403784439,1.,0.866025403784439,1.,0.866025403784439,1.,0.866025403784439,
1.,0.866025403784439,1.,0.866025403784439,1.,0.866025403784439,1.,0.866025403784439,
1.,0.866025403784439,1.,0.866025403784439,1.,0.866025403784439,1.,0.866025403784439,
1.,0.866025403784439,1.,0.866025403784439,1.,0.866025403784439,1.,0.866025403784439,
1.,0.866025403784439,1.,0.866025403784439,1.,0.866025403784439,1.,0.866025403784439,
1.,0.866025403784439,1.,0.866025403784439,1.,0.866025403784439,1.,0.866025403784439,
1.,0.866025403784439,1.,0.866025403784439,1.,0.866025403784439,1.,0.866025403784439,
1.,0.866025403784439,1.,0.866025403784439,1.,0.866025403784439,1.,0.866025403784439,
1.,0.866025403784439,1.,0.866025403784439,1.,0.866025403784439,1.,0.866025403784439,
1.,0.866025403784439,1.,0.866025403784439,1.,0.866025403784439,1.,0.866025403784439,
1.,0.866025403784439,1.,0.866025403784439,1.,0.866025403784439,1.,0.866025403784439,
1.,0.866025403784439,1.,0.866025403784439,1.,0.866025403784439,1.,0.866025403784439,
1.,0.866025403784439,1.,0.866025403784439,1.,0.866025403784439,1.,0.866025403784439,
1.,0.866025403784439,1.,0.866025403784439,1.,0.866025403784439,1.,0.866025403784439,
1.,0.866025403784439,1.,0.866025403784439,1.,0.866025403784439,1.,0.866025403784439,
1.,0.866025403784439,1.,0.866025403784439,1.,0.866025403784439,1.,0.866025403784439,
1.,0.866025403784439,1.,0.866025403784439,1.,0.866025403784439,1.,0.866025403784439,
1.,0.866025403784439,1.,0.866025403784439,1.,0.866025403784439,1.,0.866025403784439,
1.,0.866025403784439,1.,0.866025403784439,1.,0.866025403784439,1.,0.866025403784439,
1.,0.866025403784439,1.,0.866025403784439,1.,0.866025403784439,1.,0.866025403784439,
1.,0.866025403784439,1.,0.866025403784439,1.,0.866025403784439,1.,0.866025403784439,
1.,0.866025403784439,1.,0.866025403784439,1.,0.866025403784439,1.,0.866025403784439,
1.,0.9461134718712,0.935574832010768)))
REPRESENTATION_ITEM('')
SURFACE()
);
#296=(
BOUNDED_SURFACE()
B_SPLINE_SURFACE(1,2,((#30120,#30121,#30122,#30123,#30124,#30125,#30126,
#30127,#30128,#30129,#30130,#30131,#30132,#30133,#30134,#30135,#30136,#30137,
#30138,#30139,#30140,#30141,#30142,#30143,#30144,#30145,#30146,#30147,#30148,
#30149,#30150,#30151,#30152,#30153,#30154,#30155,#30156,#30157,#30158,#30159,
#30160,#30161,#30162,#30163,#30164,#30165,#30166,#30167,#30168,#30169,#30170,
#30171,#30172,#30173,#30174,#30175,#30176,#30177,#30178,#30179,#30180,#30181,
#30182,#30183,#30184,#30185,#30186,#30187,#30188,#30189,#30190,#30191,#30192,
#30193,#30194,#30195,#30196,#30197,#30198,#30199,#30200,#30201,#30202,#30203,
#30204,#30205,#30206,#30207,#30208,#30209,#30210,#30211,#30212,#30213,#30214,
#30215,#30216,#30217,#30218,#30219,#30220,#30221,#30222,#30223,#30224,#30225,
#30226,#30227,#30228,#30229,#30230,#30231,#30232,#30233,#30234,#30235,#30236,
#30237,#30238,#30239,#30240,#30241,#30242,#30243,#30244,#30245,#30246,#30247,
#30248,#30249,#30250,#30251,#30252,#30253,#30254,#30255,#30256,#30257,#30258,
#30259,#30260,#30261,#30262,#30263,#30264,#30265,#30266,#30267,#30268,#30269,
#30270,#30271,#30272,#30273,#30274,#30275,#30276,#30277,#30278,#30279,#30280,
#30281,#30282,#30283,#30284,#30285,#30286,#30287,#30288,#30289,#30290,#30291,
#30292,#30293,#30294,#30295,#30296,#30297,#30298,#30299,#30300,#30301,#30302,
#30303,#30304,#30305,#30306,#30307,#30308,#30309,#30310,#30311,#30312,#30313,
#30314,#30315,#30316,#30317,#30318,#30319,#30320,#30321,#30322,#30323,#30324,
#30325,#30326,#30327,#30328,#30329,#30330,#30331,#30332,#30333,#30334,#30335,
#30336,#30337,#30338,#30339,#30340,#30341,#30342,#30343,#30344,#30345,#30346,
#30347,#30348,#30349,#30350,#30351,#30352,#30353,#30354,#30355,#30356,#30357,
#30358,#30359,#30360,#30361,#30362,#30363,#30364,#30365,#30366,#30367,#30368,
#30369,#30370,#30371,#30372,#30373,#30374,#30375,#30376,#30377,#30378,#30379,
#30380,#30381,#30382,#30383,#30384,#30385,#30386,#30387,#30388,#30389,#30390,
#30391,#30392,#30393,#30394,#30395,#30396,#30397,#30398,#30399,#30400,#30401,
#30402,#30403,#30404,#30405,#30406,#30407,#30408,#30409,#30410,#30411,#30412,
#30413,#30414,#30415,#30416,#30417,#30418,#30419,#30420,#30421,#30422,#30423,
#30424,#30425,#30426,#30427,#30428,#30429,#30430,#30431,#30432,#30433,#30434,
#30435,#30436,#30437,#30438),(#30439,#30440,#30441,#30442,#30443,#30444,
#30445,#30446,#30447,#30448,#30449,#30450,#30451,#30452,#30453,#30454,#30455,
#30456,#30457,#30458,#30459,#30460,#30461,#30462,#30463,#30464,#30465,#30466,
#30467,#30468,#30469,#30470,#30471,#30472,#30473,#30474,#30475,#30476,#30477,
#30478,#30479,#30480,#30481,#30482,#30483,#30484,#30485,#30486,#30487,#30488,
#30489,#30490,#30491,#30492,#30493,#30494,#30495,#30496,#30497,#30498,#30499,
#30500,#30501,#30502,#30503,#30504,#30505,#30506,#30507,#30508,#30509,#30510,
#30511,#30512,#30513,#30514,#30515,#30516,#30517,#30518,#30519,#30520,#30521,
#30522,#30523,#30524,#30525,#30526,#30527,#30528,#30529,#30530,#30531,#30532,
#30533,#30534,#30535,#30536,#30537,#30538,#30539,#30540,#30541,#30542,#30543,
#30544,#30545,#30546,#30547,#30548,#30549,#30550,#30551,#30552,#30553,#30554,
#30555,#30556,#30557,#30558,#30559,#30560,#30561,#30562,#30563,#30564,#30565,
#30566,#30567,#30568,#30569,#30570,#30571,#30572,#30573,#30574,#30575,#30576,
#30577,#30578,#30579,#30580,#30581,#30582,#30583,#30584,#30585,#30586,#30587,
#30588,#30589,#30590,#30591,#30592,#30593,#30594,#30595,#30596,#30597,#30598,
#30599,#30600,#30601,#30602,#30603,#30604,#30605,#30606,#30607,#30608,#30609,
#30610,#30611,#30612,#30613,#30614,#30615,#30616,#30617,#30618,#30619,#30620,
#30621,#30622,#30623,#30624,#30625,#30626,#30627,#30628,#30629,#30630,#30631,
#30632,#30633,#30634,#30635,#30636,#30637,#30638,#30639,#30640,#30641,#30642,
#30643,#30644,#30645,#30646,#30647,#30648,#30649,#30650,#30651,#30652,#30653,
#30654,#30655,#30656,#30657,#30658,#30659,#30660,#30661,#30662,#30663,#30664,
#30665,#30666,#30667,#30668,#30669,#30670,#30671,#30672,#30673,#30674,#30675,
#30676,#30677,#30678,#30679,#30680,#30681,#30682,#30683,#30684,#30685,#30686,
#30687,#30688,#30689,#30690,#30691,#30692,#30693,#30694,#30695,#30696,#30697,
#30698,#30699,#30700,#30701,#30702,#30703,#30704,#30705,#30706,#30707,#30708,
#30709,#30710,#30711,#30712,#30713,#30714,#30715,#30716,#30717,#30718,#30719,
#30720,#30721,#30722,#30723,#30724,#30725,#30726,#30727,#30728,#30729,#30730,
#30731,#30732,#30733,#30734,#30735,#30736,#30737,#30738,#30739,#30740,#30741,
#30742,#30743,#30744,#30745,#30746,#30747,#30748,#30749,#30750,#30751,#30752,
#30753,#30754,#30755,#30756,#30757)),.UNSPECIFIED.,.F.,.F.,.F.)
B_SPLINE_SURFACE_WITH_KNOTS((2,2),(3,2,2,2,2,2,2,2,2,2,2,2,2,2,2,2,2,2,
2,2,2,2,2,2,2,2,2,2,2,2,2,2,2,2,2,2,2,2,2,2,2,2,2,2,2,2,2,2,2,2,2,2,2,2,
2,2,2,2,2,2,2,2,2,2,2,2,2,2,2,2,2,2,2,2,2,2,2,2,2,2,2,2,2,2,2,2,2,2,2,2,
2,2,2,2,2,2,2,2,2,2,2,2,2,2,2,2,2,2,2,2,2,2,2,2,2,2,2,2,2,2,2,2,2,2,2,2,
2,2,2,2,2,2,2,2,2,2,2,2,2,2,2,2,2,2,2,2,2,2,2,2,2,2,2,2,2,2,2,2,2,3),(0.,
1.00001332089206),(0.,0.00617283950617284,0.0123456790123457,0.0185185185185185,
0.0246913580246914,0.0308641975308642,0.037037037037037,0.0432098765432099,
0.0493827160493827,0.0555555555555556,0.0617283950617284,0.0679012345679012,
0.0740740740740741,0.0802469135802469,0.0864197530864197,0.0925925925925926,
0.0987654320987654,0.104938271604938,0.111111111111111,0.117283950617284,
0.123456790123457,0.12962962962963,0.135802469135802,0.141975308641975,
0.148148148148148,0.154320987654321,0.160493827160494,0.166666666666667,
0.172839506172839,0.179012345679012,0.185185185185185,0.191358024691358,
0.197530864197531,0.203703703703704,0.209876543209877,0.216049382716049,
0.222222222222222,0.228395061728395,0.234567901234568,0.240740740740741,
0.246913580246914,0.253086419753086,0.259259259259259,0.265432098765432,
0.271604938271605,0.277777777777778,0.283950617283951,0.290123456790123,
0.296296296296296,0.302469135802469,0.308641975308642,0.314814814814815,
0.320987654320988,0.327160493827161,0.333333333333333,0.339506172839506,
0.345679012345679,0.351851851851852,0.358024691358025,0.364197530864198,
0.37037037037037,0.376543209876543,0.382716049382716,0.388888888888889,
0.395061728395062,0.401234567901235,0.407407407407407,0.41358024691358,
0.419753086419753,0.425925925925926,0.432098765432099,0.438271604938272,
0.444444444444444,0.450617283950617,0.45679012345679,0.462962962962963,
0.469135802469136,0.475308641975309,0.481481481481481,0.487654320987654,
0.493827160493827,0.5,0.506172839506173,0.512345679012346,0.518518518518518,
0.524691358024691,0.530864197530864,0.537037037037037,0.54320987654321,
0.549382716049383,0.555555555555556,0.561728395061728,0.567901234567901,
0.574074074074074,0.580246913580247,0.58641975308642,0.592592592592593,
0.598765432098765,0.604938271604938,0.611111111111111,0.617283950617284,
0.623456790123457,0.62962962962963,0.635802469135803,0.641975308641975,
0.648148148148148,0.654320987654321,0.660493827160494,0.666666666666667,
0.672839506172839,0.679012345679012,0.685185185185185,0.691358024691358,
0.697530864197531,0.703703703703704,0.709876543209877,0.716049382716049,
0.722222222222222,0.728395061728395,0.734567901234568,0.740740740740741,
0.746913580246914,0.753086419753086,0.759259259259259,0.765432098765432,
0.771604938271605,0.777777777777778,0.783950617283951,0.790123456790123,
0.796296296296296,0.802469135802469,0.808641975308642,0.814814814814815,
0.820987654320988,0.827160493827161,0.833333333333333,0.839506172839506,
0.845679012345679,0.851851851851852,0.858024691358025,0.864197530864197,
0.87037037037037,0.876543209876543,0.882716049382716,0.888888888888889,
0.895061728395062,0.901234567901235,0.907407407407407,0.91358024691358,
0.919753086419753,0.925925925925926,0.932098765432099,0.938271604938272,
0.944444444444444,0.950617283950617,0.95679012345679,0.962962962962963,
0.969135802469136,0.975308641975309,0.977791440774828),.UNSPECIFIED.)
GEOMETRIC_REPRESENTATION_ITEM()
RATIONAL_B_SPLINE_SURFACE(((1.,0.866025403784439,1.,0.866025403784439,1.,
0.866025403784439,1.,0.866025403784439,1.,0.866025403784439,1.,0.866025403784439,
1.,0.866025403784439,1.,0.866025403784439,1.,0.866025403784439,1.,0.866025403784439,
1.,0.866025403784439,1.,0.866025403784439,1.,0.866025403784439,1.,0.866025403784439,
1.,0.866025403784439,1.,0.866025403784439,1.,0.866025403784439,1.,0.866025403784439,
1.,0.866025403784439,1.,0.866025403784439,1.,0.866025403784439,1.,0.866025403784439,
1.,0.866025403784439,1.,0.866025403784439,1.,0.866025403784439,1.,0.866025403784439,
1.,0.866025403784439,1.,0.866025403784439,1.,0.866025403784439,1.,0.866025403784439,
1.,0.866025403784439,1.,0.866025403784439,1.,0.866025403784439,1.,0.866025403784439,
1.,0.866025403784439,1.,0.866025403784439,1.,0.866025403784439,1.,0.866025403784439,
1.,0.866025403784439,1.,0.866025403784439,1.,0.866025403784439,1.,0.866025403784439,
1.,0.866025403784439,1.,0.866025403784439,1.,0.866025403784439,1.,0.866025403784439,
1.,0.866025403784439,1.,0.866025403784439,1.,0.866025403784439,1.,0.866025403784439,
1.,0.866025403784439,1.,0.866025403784439,1.,0.866025403784439,1.,0.866025403784439,
1.,0.866025403784439,1.,0.866025403784439,1.,0.866025403784439,1.,0.866025403784439,
1.,0.866025403784439,1.,0.866025403784439,1.,0.866025403784439,1.,0.866025403784439,
1.,0.866025403784439,1.,0.866025403784439,1.,0.866025403784439,1.,0.866025403784439,
1.,0.866025403784439,1.,0.866025403784439,1.,0.866025403784439,1.,0.866025403784439,
1.,0.866025403784439,1.,0.866025403784439,1.,0.866025403784439,1.,0.866025403784439,
1.,0.866025403784439,1.,0.866025403784439,1.,0.866025403784439,1.,0.866025403784439,
1.,0.866025403784439,1.,0.866025403784439,1.,0.866025403784439,1.,0.866025403784439,
1.,0.866025403784439,1.,0.866025403784439,1.,0.866025403784439,1.,0.866025403784439,
1.,0.866025403784439,1.,0.866025403784439,1.,0.866025403784439,1.,0.866025403784439,
1.,0.866025403784439,1.,0.866025403784439,1.,0.866025403784439,1.,0.866025403784439,
1.,0.866025403784439,1.,0.866025403784439,1.,0.866025403784439,1.,0.866025403784439,
1.,0.866025403784439,1.,0.866025403784439,1.,0.866025403784439,1.,0.866025403784439,
1.,0.866025403784439,1.,0.866025403784439,1.,0.866025403784439,1.,0.866025403784439,
1.,0.866025403784439,1.,0.866025403784439,1.,0.866025403784439,1.,0.866025403784439,
1.,0.866025403784439,1.,0.866025403784439,1.,0.866025403784439,1.,0.866025403784439,
1.,0.866025403784439,1.,0.866025403784439,1.,0.866025403784439,1.,0.866025403784439,
1.,0.866025403784439,1.,0.866025403784439,1.,0.866025403784439,1.,0.866025403784439,
1.,0.866025403784439,1.,0.866025403784439,1.,0.866025403784439,1.,0.866025403784439,
1.,0.866025403784439,1.,0.866025403784439,1.,0.866025403784439,1.,0.866025403784439,
1.,0.866025403784439,1.,0.866025403784439,1.,0.866025403784439,1.,0.866025403784439,
1.,0.866025403784439,1.,0.866025403784439,1.,0.866025403784439,1.,0.866025403784439,
1.,0.866025403784439,1.,0.866025403784439,1.,0.866025403784439,1.,0.866025403784439,
1.,0.866025403784439,1.,0.866025403784439,1.,0.866025403784439,1.,0.866025403784439,
1.,0.866025403784439,1.,0.866025403784439,1.,0.866025403784439,1.,0.866025403784439,
1.,0.866025403784439,1.,0.866025403784439,1.,0.866025403784439,1.,0.866025403784439,
1.,0.866025403784439,1.,0.866025403784439,1.,0.866025403784439,1.,0.866025403784439,
1.,0.946113621402695,0.935574890499137),(1.,0.866025403784439,1.,0.866025403784439,
1.,0.866025403784439,1.,0.866025403784439,1.,0.866025403784439,1.,0.866025403784439,
1.,0.866025403784439,1.,0.866025403784439,1.,0.866025403784439,1.,0.866025403784439,
1.,0.866025403784439,1.,0.866025403784439,1.,0.866025403784439,1.,0.866025403784439,
1.,0.866025403784439,1.,0.866025403784439,1.,0.866025403784439,1.,0.866025403784439,
1.,0.866025403784439,1.,0.866025403784439,1.,0.866025403784439,1.,0.866025403784439,
1.,0.866025403784439,1.,0.866025403784439,1.,0.866025403784439,1.,0.866025403784439,
1.,0.866025403784439,1.,0.866025403784439,1.,0.866025403784439,1.,0.866025403784439,
1.,0.866025403784439,1.,0.866025403784439,1.,0.866025403784439,1.,0.866025403784439,
1.,0.866025403784439,1.,0.866025403784439,1.,0.866025403784439,1.,0.866025403784439,
1.,0.866025403784439,1.,0.866025403784439,1.,0.866025403784439,1.,0.866025403784439,
1.,0.866025403784439,1.,0.866025403784439,1.,0.866025403784439,1.,0.866025403784439,
1.,0.866025403784439,1.,0.866025403784439,1.,0.866025403784439,1.,0.866025403784439,
1.,0.866025403784439,1.,0.866025403784439,1.,0.866025403784439,1.,0.866025403784439,
1.,0.866025403784439,1.,0.866025403784439,1.,0.866025403784439,1.,0.866025403784439,
1.,0.866025403784439,1.,0.866025403784439,1.,0.866025403784439,1.,0.866025403784439,
1.,0.866025403784439,1.,0.866025403784439,1.,0.866025403784439,1.,0.866025403784439,
1.,0.866025403784439,1.,0.866025403784439,1.,0.866025403784439,1.,0.866025403784439,
1.,0.866025403784439,1.,0.866025403784439,1.,0.866025403784439,1.,0.866025403784439,
1.,0.866025403784439,1.,0.866025403784439,1.,0.866025403784439,1.,0.866025403784439,
1.,0.866025403784439,1.,0.866025403784439,1.,0.866025403784439,1.,0.866025403784439,
1.,0.866025403784439,1.,0.866025403784439,1.,0.866025403784439,1.,0.866025403784439,
1.,0.866025403784439,1.,0.866025403784439,1.,0.866025403784439,1.,0.866025403784439,
1.,0.866025403784439,1.,0.866025403784439,1.,0.866025403784439,1.,0.866025403784439,
1.,0.866025403784439,1.,0.866025403784439,1.,0.866025403784439,1.,0.866025403784439,
1.,0.866025403784439,1.,0.866025403784439,1.,0.866025403784439,1.,0.866025403784439,
1.,0.866025403784439,1.,0.866025403784439,1.,0.866025403784439,1.,0.866025403784439,
1.,0.866025403784439,1.,0.866025403784439,1.,0.866025403784439,1.,0.866025403784439,
1.,0.866025403784439,1.,0.866025403784439,1.,0.866025403784439,1.,0.866025403784439,
1.,0.866025403784439,1.,0.866025403784439,1.,0.866025403784439,1.,0.866025403784439,
1.,0.866025403784439,1.,0.866025403784439,1.,0.866025403784439,1.,0.866025403784439,
1.,0.866025403784439,1.,0.866025403784439,1.,0.866025403784439,1.,0.866025403784439,
1.,0.866025403784439,1.,0.866025403784439,1.,0.866025403784439,1.,0.866025403784439,
1.,0.866025403784439,1.,0.866025403784439,1.,0.866025403784439,1.,0.866025403784439,
1.,0.866025403784439,1.,0.866025403784439,1.,0.866025403784439,1.,0.866025403784439,
1.,0.866025403784439,1.,0.866025403784439,1.,0.866025403784439,1.,0.866025403784439,
1.,0.866025403784439,1.,0.866025403784439,1.,0.866025403784439,1.,0.866025403784439,
1.,0.866025403784439,1.,0.866025403784439,1.,0.866025403784439,1.,0.866025403784439,
1.,0.866025403784439,1.,0.866025403784439,1.,0.866025403784439,1.,0.866025403784439,
1.,0.866025403784439,1.,0.866025403784439,1.,0.866025403784439,1.,0.866025403784439,
1.,0.946113621402695,0.935574890499137)))
REPRESENTATION_ITEM('')
SURFACE()
);
#297=(
BOUNDED_SURFACE()
B_SPLINE_SURFACE(1,2,((#31063,#31064,#31065,#31066,#31067,#31068,#31069,
#31070,#31071,#31072,#31073,#31074,#31075,#31076,#31077,#31078,#31079,#31080,
#31081,#31082,#31083,#31084,#31085,#31086,#31087,#31088,#31089,#31090,#31091,
#31092,#31093,#31094,#31095,#31096,#31097,#31098,#31099,#31100,#31101,#31102,
#31103,#31104,#31105,#31106,#31107,#31108,#31109,#31110,#31111,#31112,#31113,
#31114,#31115,#31116,#31117,#31118,#31119,#31120,#31121,#31122,#31123,#31124,
#31125,#31126,#31127,#31128,#31129,#31130,#31131,#31132,#31133,#31134,#31135,
#31136,#31137,#31138,#31139,#31140,#31141,#31142,#31143,#31144,#31145,#31146,
#31147,#31148,#31149,#31150,#31151,#31152,#31153,#31154,#31155,#31156,#31157,
#31158,#31159,#31160,#31161,#31162,#31163,#31164,#31165,#31166,#31167,#31168,
#31169,#31170,#31171,#31172,#31173,#31174,#31175,#31176,#31177,#31178,#31179,
#31180,#31181,#31182,#31183,#31184,#31185,#31186,#31187,#31188,#31189,#31190,
#31191,#31192,#31193,#31194,#31195,#31196,#31197,#31198,#31199,#31200,#31201,
#31202,#31203,#31204,#31205,#31206,#31207,#31208,#31209,#31210,#31211,#31212,
#31213,#31214,#31215,#31216,#31217,#31218,#31219,#31220,#31221,#31222,#31223,
#31224,#31225,#31226,#31227,#31228,#31229,#31230,#31231,#31232,#31233,#31234,
#31235,#31236,#31237,#31238,#31239,#31240,#31241,#31242,#31243,#31244,#31245,
#31246,#31247,#31248,#31249,#31250,#31251,#31252,#31253,#31254,#31255,#31256,
#31257,#31258,#31259,#31260,#31261,#31262,#31263,#31264,#31265,#31266,#31267,
#31268,#31269,#31270,#31271,#31272,#31273,#31274,#31275,#31276,#31277,#31278,
#31279,#31280,#31281,#31282,#31283,#31284,#31285,#31286,#31287,#31288,#31289,
#31290,#31291,#31292,#31293,#31294,#31295,#31296,#31297,#31298,#31299,#31300,
#31301,#31302,#31303,#31304,#31305,#31306,#31307,#31308,#31309,#31310,#31311,
#31312,#31313,#31314,#31315,#31316,#31317,#31318,#31319,#31320,#31321,#31322,
#31323,#31324,#31325,#31326,#31327,#31328,#31329,#31330,#31331,#31332,#31333,
#31334,#31335,#31336,#31337,#31338,#31339,#31340,#31341,#31342,#31343,#31344,
#31345,#31346,#31347,#31348,#31349,#31350,#31351,#31352,#31353,#31354,#31355,
#31356,#31357,#31358,#31359,#31360,#31361,#31362,#31363,#31364,#31365,#31366,
#31367,#31368,#31369,#31370,#31371,#31372,#31373,#31374,#31375,#31376,#31377,
#31378,#31379,#31380,#31381,#31382,#31383),(#31384,#31385,#31386,#31387,
#31388,#31389,#31390,#31391,#31392,#31393,#31394,#31395,#31396,#31397,#31398,
#31399,#31400,#31401,#31402,#31403,#31404,#31405,#31406,#31407,#31408,#31409,
#31410,#31411,#31412,#31413,#31414,#31415,#31416,#31417,#31418,#31419,#31420,
#31421,#31422,#31423,#31424,#31425,#31426,#31427,#31428,#31429,#31430,#31431,
#31432,#31433,#31434,#31435,#31436,#31437,#31438,#31439,#31440,#31441,#31442,
#31443,#31444,#31445,#31446,#31447,#31448,#31449,#31450,#31451,#31452,#31453,
#31454,#31455,#31456,#31457,#31458,#31459,#31460,#31461,#31462,#31463,#31464,
#31465,#31466,#31467,#31468,#31469,#31470,#31471,#31472,#31473,#31474,#31475,
#31476,#31477,#31478,#31479,#31480,#31481,#31482,#31483,#31484,#31485,#31486,
#31487,#31488,#31489,#31490,#31491,#31492,#31493,#31494,#31495,#31496,#31497,
#31498,#31499,#31500,#31501,#31502,#31503,#31504,#31505,#31506,#31507,#31508,
#31509,#31510,#31511,#31512,#31513,#31514,#31515,#31516,#31517,#31518,#31519,
#31520,#31521,#31522,#31523,#31524,#31525,#31526,#31527,#31528,#31529,#31530,
#31531,#31532,#31533,#31534,#31535,#31536,#31537,#31538,#31539,#31540,#31541,
#31542,#31543,#31544,#31545,#31546,#31547,#31548,#31549,#31550,#31551,#31552,
#31553,#31554,#31555,#31556,#31557,#31558,#31559,#31560,#31561,#31562,#31563,
#31564,#31565,#31566,#31567,#31568,#31569,#31570,#31571,#31572,#31573,#31574,
#31575,#31576,#31577,#31578,#31579,#31580,#31581,#31582,#31583,#31584,#31585,
#31586,#31587,#31588,#31589,#31590,#31591,#31592,#31593,#31594,#31595,#31596,
#31597,#31598,#31599,#31600,#31601,#31602,#31603,#31604,#31605,#31606,#31607,
#31608,#31609,#31610,#31611,#31612,#31613,#31614,#31615,#31616,#31617,#31618,
#31619,#31620,#31621,#31622,#31623,#31624,#31625,#31626,#31627,#31628,#31629,
#31630,#31631,#31632,#31633,#31634,#31635,#31636,#31637,#31638,#31639,#31640,
#31641,#31642,#31643,#31644,#31645,#31646,#31647,#31648,#31649,#31650,#31651,
#31652,#31653,#31654,#31655,#31656,#31657,#31658,#31659,#31660,#31661,#31662,
#31663,#31664,#31665,#31666,#31667,#31668,#31669,#31670,#31671,#31672,#31673,
#31674,#31675,#31676,#31677,#31678,#31679,#31680,#31681,#31682,#31683,#31684,
#31685,#31686,#31687,#31688,#31689,#31690,#31691,#31692,#31693,#31694,#31695,
#31696,#31697,#31698,#31699,#31700,#31701,#31702,#31703,#31704)),
 .UNSPECIFIED.,.F.,.F.,.F.)
B_SPLINE_SURFACE_WITH_KNOTS((2,2),(3,2,2,2,2,2,2,2,2,2,2,2,2,2,2,2,2,2,
2,2,2,2,2,2,2,2,2,2,2,2,2,2,2,2,2,2,2,2,2,2,2,2,2,2,2,2,2,2,2,2,2,2,2,2,
2,2,2,2,2,2,2,2,2,2,2,2,2,2,2,2,2,2,2,2,2,2,2,2,2,2,2,2,2,2,2,2,2,2,2,2,
2,2,2,2,2,2,2,2,2,2,2,2,2,2,2,2,2,2,2,2,2,2,2,2,2,2,2,2,2,2,2,2,2,2,2,2,
2,2,2,2,2,2,2,2,2,2,2,2,2,2,2,2,2,2,2,2,2,2,2,2,2,2,2,2,2,2,2,2,2,2,3),
(-0.000321975171240591,1.),(0.,0.00617283950617284,0.0123456790123457,0.0185185185185185,
0.0246913580246914,0.0308641975308642,0.037037037037037,0.0432098765432099,
0.0493827160493827,0.0555555555555556,0.0617283950617284,0.0679012345679012,
0.0740740740740741,0.0802469135802469,0.0864197530864197,0.0925925925925926,
0.0987654320987654,0.104938271604938,0.111111111111111,0.117283950617284,
0.123456790123457,0.12962962962963,0.135802469135802,0.141975308641975,
0.148148148148148,0.154320987654321,0.160493827160494,0.166666666666667,
0.172839506172839,0.179012345679012,0.185185185185185,0.191358024691358,
0.197530864197531,0.203703703703704,0.209876543209877,0.216049382716049,
0.222222222222222,0.228395061728395,0.234567901234568,0.240740740740741,
0.246913580246914,0.253086419753086,0.259259259259259,0.265432098765432,
0.271604938271605,0.277777777777778,0.283950617283951,0.290123456790123,
0.296296296296296,0.302469135802469,0.308641975308642,0.314814814814815,
0.320987654320988,0.327160493827161,0.333333333333333,0.339506172839506,
0.345679012345679,0.351851851851852,0.358024691358025,0.364197530864198,
0.37037037037037,0.376543209876543,0.382716049382716,0.388888888888889,
0.395061728395062,0.401234567901235,0.407407407407407,0.41358024691358,
0.419753086419753,0.425925925925926,0.432098765432099,0.438271604938272,
0.444444444444444,0.450617283950617,0.45679012345679,0.462962962962963,
0.469135802469136,0.475308641975309,0.481481481481481,0.487654320987654,
0.493827160493827,0.5,0.506172839506173,0.512345679012346,0.518518518518518,
0.524691358024691,0.530864197530864,0.537037037037037,0.54320987654321,
0.549382716049383,0.555555555555556,0.561728395061728,0.567901234567901,
0.574074074074074,0.580246913580247,0.58641975308642,0.592592592592593,
0.598765432098765,0.604938271604938,0.611111111111111,0.617283950617284,
0.623456790123457,0.62962962962963,0.635802469135803,0.641975308641975,
0.648148148148148,0.654320987654321,0.660493827160494,0.666666666666667,
0.672839506172839,0.679012345679012,0.685185185185185,0.691358024691358,
0.697530864197531,0.703703703703704,0.709876543209877,0.716049382716049,
0.722222222222222,0.728395061728395,0.734567901234568,0.740740740740741,
0.746913580246914,0.753086419753086,0.759259259259259,0.765432098765432,
0.771604938271605,0.777777777777778,0.783950617283951,0.790123456790123,
0.796296296296296,0.802469135802469,0.808641975308642,0.814814814814815,
0.820987654320988,0.827160493827161,0.833333333333333,0.839506172839506,
0.845679012345679,0.851851851851852,0.858024691358025,0.864197530864197,
0.87037037037037,0.876543209876543,0.882716049382716,0.888888888888889,
0.895061728395062,0.901234567901235,0.907407407407407,0.91358024691358,
0.919753086419753,0.925925925925926,0.932098765432099,0.938271604938272,
0.944444444444444,0.950617283950617,0.95679012345679,0.962962962962963,
0.969135802469136,0.975308641975309,0.977791393533952,0.987569307469292),
 .UNSPECIFIED.)
GEOMETRIC_REPRESENTATION_ITEM()
RATIONAL_B_SPLINE_SURFACE(((1.,0.866025403784439,1.,0.866025403784439,1.,
0.866025403784439,1.,0.866025403784439,1.,0.866025403784439,1.,0.866025403784439,
1.,0.866025403784439,1.,0.866025403784439,1.,0.866025403784439,1.,0.866025403784439,
1.,0.866025403784439,1.,0.866025403784439,1.,0.866025403784439,1.,0.866025403784439,
1.,0.866025403784439,1.,0.866025403784439,1.,0.866025403784439,1.,0.866025403784439,
1.,0.866025403784439,1.,0.866025403784439,1.,0.866025403784439,1.,0.866025403784439,
1.,0.866025403784439,1.,0.866025403784439,1.,0.866025403784439,1.,0.866025403784439,
1.,0.866025403784439,1.,0.866025403784439,1.,0.866025403784439,1.,0.866025403784439,
1.,0.866025403784439,1.,0.866025403784439,1.,0.866025403784439,1.,0.866025403784439,
1.,0.866025403784439,1.,0.866025403784439,1.,0.866025403784439,1.,0.866025403784439,
1.,0.866025403784439,1.,0.866025403784439,1.,0.866025403784439,1.,0.866025403784439,
1.,0.866025403784439,1.,0.866025403784439,1.,0.866025403784439,1.,0.866025403784439,
1.,0.866025403784439,1.,0.866025403784439,1.,0.866025403784439,1.,0.866025403784439,
1.,0.866025403784439,1.,0.866025403784439,1.,0.866025403784439,1.,0.866025403784439,
1.,0.866025403784439,1.,0.866025403784439,1.,0.866025403784439,1.,0.866025403784439,
1.,0.866025403784439,1.,0.866025403784439,1.,0.866025403784439,1.,0.866025403784439,
1.,0.866025403784439,1.,0.866025403784439,1.,0.866025403784439,1.,0.866025403784439,
1.,0.866025403784439,1.,0.866025403784439,1.,0.866025403784439,1.,0.866025403784439,
1.,0.866025403784439,1.,0.866025403784439,1.,0.866025403784439,1.,0.866025403784439,
1.,0.866025403784439,1.,0.866025403784439,1.,0.866025403784439,1.,0.866025403784439,
1.,0.866025403784439,1.,0.866025403784439,1.,0.866025403784439,1.,0.866025403784439,
1.,0.866025403784439,1.,0.866025403784439,1.,0.866025403784439,1.,0.866025403784439,
1.,0.866025403784439,1.,0.866025403784439,1.,0.866025403784439,1.,0.866025403784439,
1.,0.866025403784439,1.,0.866025403784439,1.,0.866025403784439,1.,0.866025403784439,
1.,0.866025403784439,1.,0.866025403784439,1.,0.866025403784439,1.,0.866025403784439,
1.,0.866025403784439,1.,0.866025403784439,1.,0.866025403784439,1.,0.866025403784439,
1.,0.866025403784439,1.,0.866025403784439,1.,0.866025403784439,1.,0.866025403784439,
1.,0.866025403784439,1.,0.866025403784439,1.,0.866025403784439,1.,0.866025403784439,
1.,0.866025403784439,1.,0.866025403784439,1.,0.866025403784439,1.,0.866025403784439,
1.,0.866025403784439,1.,0.866025403784439,1.,0.866025403784439,1.,0.866025403784439,
1.,0.866025403784439,1.,0.866025403784439,1.,0.866025403784439,1.,0.866025403784439,
1.,0.866025403784439,1.,0.866025403784439,1.,0.866025403784439,1.,0.866025403784439,
1.,0.866025403784439,1.,0.866025403784439,1.,0.866025403784439,1.,0.866025403784439,
1.,0.866025403784439,1.,0.866025403784439,1.,0.866025403784439,1.,0.866025403784439,
1.,0.866025403784439,1.,0.866025403784439,1.,0.866025403784439,1.,0.866025403784439,
1.,0.866025403784439,1.,0.866025403784439,1.,0.866025403784439,1.,0.866025403784439,
1.,0.866025403784439,1.,0.866025403784439,1.,0.866025403784439,1.,0.866025403784439,
1.,0.866025403784439,1.,0.866025403784439,1.,0.866025403784439,1.,0.866025403784439,
1.,0.866025403784439,1.,0.866025403784439,1.,0.866025403784439,1.,0.866025403784439,
1.,0.866025403784439,1.,0.866025403784439,1.,0.866025403784439,1.,0.866025403784439,
1.,0.946114646713198,0.93557529156132,0.93557529156132,0.93557529156132),
(1.,0.866025403784439,1.,0.866025403784439,1.,0.866025403784439,1.,0.866025403784439,
1.,0.866025403784439,1.,0.866025403784439,1.,0.866025403784439,1.,0.866025403784439,
1.,0.866025403784439,1.,0.866025403784439,1.,0.866025403784439,1.,0.866025403784439,
1.,0.866025403784439,1.,0.866025403784439,1.,0.866025403784439,1.,0.866025403784439,
1.,0.866025403784439,1.,0.866025403784439,1.,0.866025403784439,1.,0.866025403784439,
1.,0.866025403784439,1.,0.866025403784439,1.,0.866025403784439,1.,0.866025403784439,
1.,0.866025403784439,1.,0.866025403784439,1.,0.866025403784439,1.,0.866025403784439,
1.,0.866025403784439,1.,0.866025403784439,1.,0.866025403784439,1.,0.866025403784439,
1.,0.866025403784439,1.,0.866025403784439,1.,0.866025403784439,1.,0.866025403784439,
1.,0.866025403784439,1.,0.866025403784439,1.,0.866025403784439,1.,0.866025403784439,
1.,0.866025403784439,1.,0.866025403784439,1.,0.866025403784439,1.,0.866025403784439,
1.,0.866025403784439,1.,0.866025403784439,1.,0.866025403784439,1.,0.866025403784439,
1.,0.866025403784439,1.,0.866025403784439,1.,0.866025403784439,1.,0.866025403784439,
1.,0.866025403784439,1.,0.866025403784439,1.,0.866025403784439,1.,0.866025403784439,
1.,0.866025403784439,1.,0.866025403784439,1.,0.866025403784439,1.,0.866025403784439,
1.,0.866025403784439,1.,0.866025403784439,1.,0.866025403784439,1.,0.866025403784439,
1.,0.866025403784439,1.,0.866025403784439,1.,0.866025403784439,1.,0.866025403784439,
1.,0.866025403784439,1.,0.866025403784439,1.,0.866025403784439,1.,0.866025403784439,
1.,0.866025403784439,1.,0.866025403784439,1.,0.866025403784439,1.,0.866025403784439,
1.,0.866025403784439,1.,0.866025403784439,1.,0.866025403784439,1.,0.866025403784439,
1.,0.866025403784439,1.,0.866025403784439,1.,0.866025403784439,1.,0.866025403784439,
1.,0.866025403784439,1.,0.866025403784439,1.,0.866025403784439,1.,0.866025403784439,
1.,0.866025403784439,1.,0.866025403784439,1.,0.866025403784439,1.,0.866025403784439,
1.,0.866025403784439,1.,0.866025403784439,1.,0.866025403784439,1.,0.866025403784439,
1.,0.866025403784439,1.,0.866025403784439,1.,0.866025403784439,1.,0.866025403784439,
1.,0.866025403784439,1.,0.866025403784439,1.,0.866025403784439,1.,0.866025403784439,
1.,0.866025403784439,1.,0.866025403784439,1.,0.866025403784439,1.,0.866025403784439,
1.,0.866025403784439,1.,0.866025403784439,1.,0.866025403784439,1.,0.866025403784439,
1.,0.866025403784439,1.,0.866025403784439,1.,0.866025403784439,1.,0.866025403784439,
1.,0.866025403784439,1.,0.866025403784439,1.,0.866025403784439,1.,0.866025403784439,
1.,0.866025403784439,1.,0.866025403784439,1.,0.866025403784439,1.,0.866025403784439,
1.,0.866025403784439,1.,0.866025403784439,1.,0.866025403784439,1.,0.866025403784439,
1.,0.866025403784439,1.,0.866025403784439,1.,0.866025403784439,1.,0.866025403784439,
1.,0.866025403784439,1.,0.866025403784439,1.,0.866025403784439,1.,0.866025403784439,
1.,0.866025403784439,1.,0.866025403784439,1.,0.866025403784439,1.,0.866025403784439,
1.,0.866025403784439,1.,0.866025403784439,1.,0.866025403784439,1.,0.866025403784439,
1.,0.866025403784439,1.,0.866025403784439,1.,0.866025403784439,1.,0.866025403784439,
1.,0.866025403784439,1.,0.866025403784439,1.,0.866025403784439,1.,0.866025403784439,
1.,0.866025403784439,1.,0.866025403784439,1.,0.866025403784439,1.,0.866025403784439,
1.,0.866025403784439,1.,0.866025403784439,1.,0.946114646713198,0.93557529156132,
0.93557529156132,0.93557529156132)))
REPRESENTATION_ITEM('')
SURFACE()
);
#298=(
BOUNDED_SURFACE()
B_SPLINE_SURFACE(1,2,((#31705,#31706,#31707,#31708,#31709,#31710,#31711,
#31712,#31713,#31714,#31715,#31716,#31717,#31718,#31719,#31720,#31721,#31722,
#31723,#31724,#31725,#31726,#31727,#31728,#31729,#31730,#31731,#31732,#31733,
#31734,#31735,#31736,#31737,#31738,#31739,#31740,#31741,#31742,#31743,#31744,
#31745,#31746,#31747,#31748,#31749,#31750,#31751,#31752,#31753,#31754,#31755,
#31756,#31757,#31758,#31759,#31760,#31761,#31762,#31763,#31764,#31765,#31766,
#31767,#31768,#31769,#31770,#31771,#31772,#31773,#31774,#31775,#31776,#31777,
#31778,#31779,#31780,#31781,#31782,#31783,#31784,#31785,#31786,#31787,#31788,
#31789,#31790,#31791,#31792,#31793,#31794,#31795,#31796,#31797,#31798,#31799,
#31800,#31801,#31802,#31803,#31804,#31805,#31806,#31807,#31808,#31809,#31810,
#31811,#31812,#31813,#31814,#31815,#31816,#31817,#31818,#31819,#31820,#31821,
#31822,#31823,#31824,#31825,#31826,#31827,#31828,#31829,#31830,#31831,#31832,
#31833,#31834,#31835,#31836,#31837,#31838,#31839,#31840,#31841,#31842,#31843,
#31844,#31845,#31846,#31847,#31848,#31849,#31850,#31851,#31852,#31853,#31854,
#31855,#31856,#31857,#31858,#31859,#31860,#31861,#31862,#31863,#31864,#31865,
#31866,#31867,#31868,#31869,#31870,#31871,#31872,#31873,#31874,#31875,#31876,
#31877,#31878,#31879,#31880,#31881,#31882,#31883,#31884,#31885,#31886,#31887,
#31888,#31889,#31890,#31891,#31892,#31893,#31894,#31895,#31896,#31897,#31898,
#31899,#31900,#31901,#31902,#31903,#31904,#31905,#31906,#31907,#31908,#31909,
#31910,#31911,#31912,#31913,#31914,#31915,#31916,#31917,#31918,#31919,#31920,
#31921,#31922,#31923,#31924,#31925,#31926,#31927,#31928,#31929,#31930,#31931,
#31932,#31933,#31934,#31935,#31936,#31937,#31938,#31939,#31940,#31941,#31942,
#31943,#31944,#31945,#31946,#31947,#31948,#31949,#31950,#31951,#31952,#31953,
#31954,#31955,#31956,#31957,#31958,#31959,#31960,#31961,#31962,#31963,#31964,
#31965,#31966,#31967,#31968,#31969,#31970,#31971,#31972,#31973,#31974,#31975,
#31976,#31977,#31978,#31979,#31980,#31981,#31982,#31983,#31984,#31985,#31986,
#31987,#31988,#31989,#31990,#31991,#31992,#31993,#31994,#31995,#31996,#31997,
#31998,#31999,#32000,#32001,#32002,#32003,#32004,#32005,#32006,#32007,#32008,
#32009,#32010,#32011,#32012,#32013,#32014,#32015,#32016,#32017,#32018,#32019,
#32020,#32021,#32022,#32023),(#32024,#32025,#32026,#32027,#32028,#32029,
#32030,#32031,#32032,#32033,#32034,#32035,#32036,#32037,#32038,#32039,#32040,
#32041,#32042,#32043,#32044,#32045,#32046,#32047,#32048,#32049,#32050,#32051,
#32052,#32053,#32054,#32055,#32056,#32057,#32058,#32059,#32060,#32061,#32062,
#32063,#32064,#32065,#32066,#32067,#32068,#32069,#32070,#32071,#32072,#32073,
#32074,#32075,#32076,#32077,#32078,#32079,#32080,#32081,#32082,#32083,#32084,
#32085,#32086,#32087,#32088,#32089,#32090,#32091,#32092,#32093,#32094,#32095,
#32096,#32097,#32098,#32099,#32100,#32101,#32102,#32103,#32104,#32105,#32106,
#32107,#32108,#32109,#32110,#32111,#32112,#32113,#32114,#32115,#32116,#32117,
#32118,#32119,#32120,#32121,#32122,#32123,#32124,#32125,#32126,#32127,#32128,
#32129,#32130,#32131,#32132,#32133,#32134,#32135,#32136,#32137,#32138,#32139,
#32140,#32141,#32142,#32143,#32144,#32145,#32146,#32147,#32148,#32149,#32150,
#32151,#32152,#32153,#32154,#32155,#32156,#32157,#32158,#32159,#32160,#32161,
#32162,#32163,#32164,#32165,#32166,#32167,#32168,#32169,#32170,#32171,#32172,
#32173,#32174,#32175,#32176,#32177,#32178,#32179,#32180,#32181,#32182,#32183,
#32184,#32185,#32186,#32187,#32188,#32189,#32190,#32191,#32192,#32193,#32194,
#32195,#32196,#32197,#32198,#32199,#32200,#32201,#32202,#32203,#32204,#32205,
#32206,#32207,#32208,#32209,#32210,#32211,#32212,#32213,#32214,#32215,#32216,
#32217,#32218,#32219,#32220,#32221,#32222,#32223,#32224,#32225,#32226,#32227,
#32228,#32229,#32230,#32231,#32232,#32233,#32234,#32235,#32236,#32237,#32238,
#32239,#32240,#32241,#32242,#32243,#32244,#32245,#32246,#32247,#32248,#32249,
#32250,#32251,#32252,#32253,#32254,#32255,#32256,#32257,#32258,#32259,#32260,
#32261,#32262,#32263,#32264,#32265,#32266,#32267,#32268,#32269,#32270,#32271,
#32272,#32273,#32274,#32275,#32276,#32277,#32278,#32279,#32280,#32281,#32282,
#32283,#32284,#32285,#32286,#32287,#32288,#32289,#32290,#32291,#32292,#32293,
#32294,#32295,#32296,#32297,#32298,#32299,#32300,#32301,#32302,#32303,#32304,
#32305,#32306,#32307,#32308,#32309,#32310,#32311,#32312,#32313,#32314,#32315,
#32316,#32317,#32318,#32319,#32320,#32321,#32322,#32323,#32324,#32325,#32326,
#32327,#32328,#32329,#32330,#32331,#32332,#32333,#32334,#32335,#32336,#32337,
#32338,#32339,#32340,#32341,#32342)),.UNSPECIFIED.,.F.,.F.,.F.)
B_SPLINE_SURFACE_WITH_KNOTS((2,2),(3,2,2,2,2,2,2,2,2,2,2,2,2,2,2,2,2,2,
2,2,2,2,2,2,2,2,2,2,2,2,2,2,2,2,2,2,2,2,2,2,2,2,2,2,2,2,2,2,2,2,2,2,2,2,
2,2,2,2,2,2,2,2,2,2,2,2,2,2,2,2,2,2,2,2,2,2,2,2,2,2,2,2,2,2,2,2,2,2,2,2,
2,2,2,2,2,2,2,2,2,2,2,2,2,2,2,2,2,2,2,2,2,2,2,2,2,2,2,2,2,2,2,2,2,2,2,2,
2,2,2,2,2,2,2,2,2,2,2,2,2,2,2,2,2,2,2,2,2,2,2,2,2,2,2,2,2,2,2,2,2,3),(-2.473386913217E-5,
1.),(0.,0.00617283950617284,0.0123456790123457,0.0185185185185185,0.0246913580246914,
0.0308641975308642,0.037037037037037,0.0432098765432099,0.0493827160493827,
0.0555555555555556,0.0617283950617284,0.0679012345679012,0.0740740740740741,
0.0802469135802469,0.0864197530864197,0.0925925925925926,0.0987654320987654,
0.104938271604938,0.111111111111111,0.117283950617284,0.123456790123457,
0.12962962962963,0.135802469135802,0.141975308641975,0.148148148148148,
0.154320987654321,0.160493827160494,0.166666666666667,0.172839506172839,
0.179012345679012,0.185185185185185,0.191358024691358,0.197530864197531,
0.203703703703704,0.209876543209877,0.216049382716049,0.222222222222222,
0.228395061728395,0.234567901234568,0.240740740740741,0.246913580246914,
0.253086419753086,0.259259259259259,0.265432098765432,0.271604938271605,
0.277777777777778,0.283950617283951,0.290123456790123,0.296296296296296,
0.302469135802469,0.308641975308642,0.314814814814815,0.320987654320988,
0.327160493827161,0.333333333333333,0.339506172839506,0.345679012345679,
0.351851851851852,0.358024691358025,0.364197530864198,0.37037037037037,
0.376543209876543,0.382716049382716,0.388888888888889,0.395061728395062,
0.401234567901235,0.407407407407407,0.41358024691358,0.419753086419753,
0.425925925925926,0.432098765432099,0.438271604938272,0.444444444444444,
0.450617283950617,0.45679012345679,0.462962962962963,0.469135802469136,
0.475308641975309,0.481481481481481,0.487654320987654,0.493827160493827,
0.5,0.506172839506173,0.512345679012346,0.518518518518518,0.524691358024691,
0.530864197530864,0.537037037037037,0.54320987654321,0.549382716049383,
0.555555555555556,0.561728395061728,0.567901234567901,0.574074074074074,
0.580246913580247,0.58641975308642,0.592592592592593,0.598765432098765,
0.604938271604938,0.611111111111111,0.617283950617284,0.623456790123457,
0.62962962962963,0.635802469135803,0.641975308641975,0.648148148148148,
0.654320987654321,0.660493827160494,0.666666666666667,0.672839506172839,
0.679012345679012,0.685185185185185,0.691358024691358,0.697530864197531,
0.703703703703704,0.709876543209877,0.716049382716049,0.722222222222222,
0.728395061728395,0.734567901234568,0.740740740740741,0.746913580246914,
0.753086419753086,0.759259259259259,0.765432098765432,0.771604938271605,
0.777777777777778,0.783950617283951,0.790123456790123,0.796296296296296,
0.802469135802469,0.808641975308642,0.814814814814815,0.820987654320988,
0.827160493827161,0.833333333333333,0.839506172839506,0.845679012345679,
0.851851851851852,0.858024691358025,0.864197530864197,0.87037037037037,
0.876543209876543,0.882716049382716,0.888888888888889,0.895061728395062,
0.901234567901235,0.907407407407407,0.91358024691358,0.919753086419753,
0.925925925925926,0.932098765432099,0.938271604938272,0.944444444444444,
0.950617283950617,0.95679012345679,0.962962962962963,0.969135802469136,
0.975308641975309,0.977791447664447),.UNSPECIFIED.)
GEOMETRIC_REPRESENTATION_ITEM()
RATIONAL_B_SPLINE_SURFACE(((1.,0.866025403784439,1.,0.866025403784439,1.,
0.866025403784439,1.,0.866025403784439,1.,0.866025403784439,1.,0.866025403784439,
1.,0.866025403784439,1.,0.866025403784439,1.,0.866025403784439,1.,0.866025403784439,
1.,0.866025403784439,1.,0.866025403784439,1.,0.866025403784439,1.,0.866025403784439,
1.,0.866025403784439,1.,0.866025403784439,1.,0.866025403784439,1.,0.866025403784439,
1.,0.866025403784439,1.,0.866025403784439,1.,0.866025403784439,1.,0.866025403784439,
1.,0.866025403784439,1.,0.866025403784439,1.,0.866025403784439,1.,0.866025403784439,
1.,0.866025403784439,1.,0.866025403784439,1.,0.866025403784439,1.,0.866025403784439,
1.,0.866025403784439,1.,0.866025403784439,1.,0.866025403784439,1.,0.866025403784439,
1.,0.866025403784439,1.,0.866025403784439,1.,0.866025403784439,1.,0.866025403784439,
1.,0.866025403784439,1.,0.866025403784439,1.,0.866025403784439,1.,0.866025403784439,
1.,0.866025403784439,1.,0.866025403784439,1.,0.866025403784439,1.,0.866025403784439,
1.,0.866025403784439,1.,0.866025403784439,1.,0.866025403784439,1.,0.866025403784439,
1.,0.866025403784439,1.,0.866025403784439,1.,0.866025403784439,1.,0.866025403784439,
1.,0.866025403784439,1.,0.866025403784439,1.,0.866025403784439,1.,0.866025403784439,
1.,0.866025403784439,1.,0.866025403784439,1.,0.866025403784439,1.,0.866025403784439,
1.,0.866025403784439,1.,0.866025403784439,1.,0.866025403784439,1.,0.866025403784439,
1.,0.866025403784439,1.,0.866025403784439,1.,0.866025403784439,1.,0.866025403784439,
1.,0.866025403784439,1.,0.866025403784439,1.,0.866025403784439,1.,0.866025403784439,
1.,0.866025403784439,1.,0.866025403784439,1.,0.866025403784439,1.,0.866025403784439,
1.,0.866025403784439,1.,0.866025403784439,1.,0.866025403784439,1.,0.866025403784439,
1.,0.866025403784439,1.,0.866025403784439,1.,0.866025403784439,1.,0.866025403784439,
1.,0.866025403784439,1.,0.866025403784439,1.,0.866025403784439,1.,0.866025403784439,
1.,0.866025403784439,1.,0.866025403784439,1.,0.866025403784439,1.,0.866025403784439,
1.,0.866025403784439,1.,0.866025403784439,1.,0.866025403784439,1.,0.866025403784439,
1.,0.866025403784439,1.,0.866025403784439,1.,0.866025403784439,1.,0.866025403784439,
1.,0.866025403784439,1.,0.866025403784439,1.,0.866025403784439,1.,0.866025403784439,
1.,0.866025403784439,1.,0.866025403784439,1.,0.866025403784439,1.,0.866025403784439,
1.,0.866025403784439,1.,0.866025403784439,1.,0.866025403784439,1.,0.866025403784439,
1.,0.866025403784439,1.,0.866025403784439,1.,0.866025403784439,1.,0.866025403784439,
1.,0.866025403784439,1.,0.866025403784439,1.,0.866025403784439,1.,0.866025403784439,
1.,0.866025403784439,1.,0.866025403784439,1.,0.866025403784439,1.,0.866025403784439,
1.,0.866025403784439,1.,0.866025403784439,1.,0.866025403784439,1.,0.866025403784439,
1.,0.866025403784439,1.,0.866025403784439,1.,0.866025403784439,1.,0.866025403784439,
1.,0.866025403784439,1.,0.866025403784439,1.,0.866025403784439,1.,0.866025403784439,
1.,0.866025403784439,1.,0.866025403784439,1.,0.866025403784439,1.,0.866025403784439,
1.,0.866025403784439,1.,0.866025403784439,1.,0.866025403784439,1.,0.866025403784439,
1.,0.866025403784439,1.,0.866025403784439,1.,0.866025403784439,1.,0.866025403784439,
1.,0.866025403784439,1.,0.866025403784439,1.,0.866025403784439,1.,0.866025403784439,
1.,0.866025403784439,1.,0.866025403784439,1.,0.866025403784439,1.,0.866025403784439,
1.,0.9461134718712,0.935574832010768),(1.,0.866025403784439,1.,0.866025403784439,
1.,0.866025403784439,1.,0.866025403784439,1.,0.866025403784439,1.,0.866025403784439,
1.,0.866025403784439,1.,0.866025403784439,1.,0.866025403784439,1.,0.866025403784439,
1.,0.866025403784439,1.,0.866025403784439,1.,0.866025403784439,1.,0.866025403784439,
1.,0.866025403784439,1.,0.866025403784439,1.,0.866025403784439,1.,0.866025403784439,
1.,0.866025403784439,1.,0.866025403784439,1.,0.866025403784439,1.,0.866025403784439,
1.,0.866025403784439,1.,0.866025403784439,1.,0.866025403784439,1.,0.866025403784439,
1.,0.866025403784439,1.,0.866025403784439,1.,0.866025403784439,1.,0.866025403784439,
1.,0.866025403784439,1.,0.866025403784439,1.,0.866025403784439,1.,0.866025403784439,
1.,0.866025403784439,1.,0.866025403784439,1.,0.866025403784439,1.,0.866025403784439,
1.,0.866025403784439,1.,0.866025403784439,1.,0.866025403784439,1.,0.866025403784439,
1.,0.866025403784439,1.,0.866025403784439,1.,0.866025403784439,1.,0.866025403784439,
1.,0.866025403784439,1.,0.866025403784439,1.,0.866025403784439,1.,0.866025403784439,
1.,0.866025403784439,1.,0.866025403784439,1.,0.866025403784439,1.,0.866025403784439,
1.,0.866025403784439,1.,0.866025403784439,1.,0.866025403784439,1.,0.866025403784439,
1.,0.866025403784439,1.,0.866025403784439,1.,0.866025403784439,1.,0.866025403784439,
1.,0.866025403784439,1.,0.866025403784439,1.,0.866025403784439,1.,0.866025403784439,
1.,0.866025403784439,1.,0.866025403784439,1.,0.866025403784439,1.,0.866025403784439,
1.,0.866025403784439,1.,0.866025403784439,1.,0.866025403784439,1.,0.866025403784439,
1.,0.866025403784439,1.,0.866025403784439,1.,0.866025403784439,1.,0.866025403784439,
1.,0.866025403784439,1.,0.866025403784439,1.,0.866025403784439,1.,0.866025403784439,
1.,0.866025403784439,1.,0.866025403784439,1.,0.866025403784439,1.,0.866025403784439,
1.,0.866025403784439,1.,0.866025403784439,1.,0.866025403784439,1.,0.866025403784439,
1.,0.866025403784439,1.,0.866025403784439,1.,0.866025403784439,1.,0.866025403784439,
1.,0.866025403784439,1.,0.866025403784439,1.,0.866025403784439,1.,0.866025403784439,
1.,0.866025403784439,1.,0.866025403784439,1.,0.866025403784439,1.,0.866025403784439,
1.,0.866025403784439,1.,0.866025403784439,1.,0.866025403784439,1.,0.866025403784439,
1.,0.866025403784439,1.,0.866025403784439,1.,0.866025403784439,1.,0.866025403784439,
1.,0.866025403784439,1.,0.866025403784439,1.,0.866025403784439,1.,0.866025403784439,
1.,0.866025403784439,1.,0.866025403784439,1.,0.866025403784439,1.,0.866025403784439,
1.,0.866025403784439,1.,0.866025403784439,1.,0.866025403784439,1.,0.866025403784439,
1.,0.866025403784439,1.,0.866025403784439,1.,0.866025403784439,1.,0.866025403784439,
1.,0.866025403784439,1.,0.866025403784439,1.,0.866025403784439,1.,0.866025403784439,
1.,0.866025403784439,1.,0.866025403784439,1.,0.866025403784439,1.,0.866025403784439,
1.,0.866025403784439,1.,0.866025403784439,1.,0.866025403784439,1.,0.866025403784439,
1.,0.866025403784439,1.,0.866025403784439,1.,0.866025403784439,1.,0.866025403784439,
1.,0.866025403784439,1.,0.866025403784439,1.,0.866025403784439,1.,0.866025403784439,
1.,0.866025403784439,1.,0.866025403784439,1.,0.866025403784439,1.,0.866025403784439,
1.,0.866025403784439,1.,0.866025403784439,1.,0.866025403784439,1.,0.866025403784439,
1.,0.866025403784439,1.,0.866025403784439,1.,0.866025403784439,1.,0.866025403784439,
1.,0.9461134718712,0.935574832010768)))
REPRESENTATION_ITEM('')
SURFACE()
);
#299=(
BOUNDED_SURFACE()
B_SPLINE_SURFACE(1,2,((#32646,#32647,#32648,#32649,#32650,#32651,#32652,
#32653,#32654,#32655,#32656,#32657,#32658,#32659,#32660,#32661,#32662,#32663,
#32664,#32665,#32666,#32667,#32668,#32669,#32670,#32671,#32672,#32673,#32674,
#32675,#32676,#32677,#32678,#32679,#32680,#32681,#32682,#32683,#32684,#32685,
#32686,#32687,#32688,#32689,#32690,#32691,#32692,#32693,#32694,#32695,#32696,
#32697,#32698,#32699,#32700,#32701,#32702,#32703,#32704,#32705,#32706,#32707,
#32708,#32709,#32710,#32711,#32712,#32713,#32714,#32715,#32716,#32717,#32718,
#32719,#32720,#32721,#32722,#32723,#32724,#32725,#32726,#32727,#32728,#32729,
#32730,#32731,#32732,#32733,#32734,#32735,#32736,#32737,#32738,#32739,#32740,
#32741,#32742,#32743,#32744,#32745,#32746,#32747,#32748,#32749,#32750,#32751,
#32752,#32753,#32754,#32755,#32756,#32757,#32758,#32759,#32760,#32761,#32762,
#32763,#32764,#32765,#32766,#32767,#32768,#32769,#32770,#32771,#32772,#32773,
#32774,#32775,#32776,#32777,#32778,#32779,#32780,#32781,#32782,#32783,#32784,
#32785,#32786,#32787,#32788,#32789,#32790,#32791,#32792,#32793,#32794,#32795,
#32796,#32797,#32798,#32799,#32800,#32801,#32802,#32803,#32804,#32805,#32806,
#32807,#32808,#32809,#32810,#32811,#32812,#32813,#32814,#32815,#32816,#32817,
#32818,#32819,#32820,#32821,#32822,#32823,#32824,#32825,#32826,#32827,#32828,
#32829,#32830,#32831,#32832,#32833,#32834,#32835,#32836,#32837,#32838,#32839,
#32840,#32841,#32842,#32843,#32844,#32845,#32846,#32847,#32848,#32849,#32850,
#32851,#32852,#32853,#32854,#32855,#32856,#32857,#32858,#32859,#32860,#32861,
#32862,#32863,#32864,#32865,#32866,#32867,#32868,#32869,#32870,#32871,#32872,
#32873,#32874,#32875,#32876,#32877,#32878,#32879,#32880,#32881,#32882,#32883,
#32884,#32885,#32886,#32887,#32888,#32889,#32890,#32891,#32892,#32893,#32894,
#32895,#32896,#32897,#32898,#32899,#32900,#32901,#32902,#32903,#32904,#32905,
#32906,#32907,#32908,#32909,#32910,#32911,#32912,#32913,#32914,#32915,#32916,
#32917,#32918,#32919,#32920,#32921,#32922,#32923,#32924,#32925,#32926,#32927,
#32928,#32929,#32930,#32931,#32932,#32933,#32934,#32935,#32936,#32937,#32938,
#32939,#32940,#32941,#32942,#32943,#32944,#32945,#32946,#32947,#32948,#32949,
#32950,#32951,#32952,#32953,#32954,#32955,#32956,#32957,#32958,#32959,#32960,
#32961,#32962,#32963,#32964),(#32965,#32966,#32967,#32968,#32969,#32970,
#32971,#32972,#32973,#32974,#32975,#32976,#32977,#32978,#32979,#32980,#32981,
#32982,#32983,#32984,#32985,#32986,#32987,#32988,#32989,#32990,#32991,#32992,
#32993,#32994,#32995,#32996,#32997,#32998,#32999,#33000,#33001,#33002,#33003,
#33004,#33005,#33006,#33007,#33008,#33009,#33010,#33011,#33012,#33013,#33014,
#33015,#33016,#33017,#33018,#33019,#33020,#33021,#33022,#33023,#33024,#33025,
#33026,#33027,#33028,#33029,#33030,#33031,#33032,#33033,#33034,#33035,#33036,
#33037,#33038,#33039,#33040,#33041,#33042,#33043,#33044,#33045,#33046,#33047,
#33048,#33049,#33050,#33051,#33052,#33053,#33054,#33055,#33056,#33057,#33058,
#33059,#33060,#33061,#33062,#33063,#33064,#33065,#33066,#33067,#33068,#33069,
#33070,#33071,#33072,#33073,#33074,#33075,#33076,#33077,#33078,#33079,#33080,
#33081,#33082,#33083,#33084,#33085,#33086,#33087,#33088,#33089,#33090,#33091,
#33092,#33093,#33094,#33095,#33096,#33097,#33098,#33099,#33100,#33101,#33102,
#33103,#33104,#33105,#33106,#33107,#33108,#33109,#33110,#33111,#33112,#33113,
#33114,#33115,#33116,#33117,#33118,#33119,#33120,#33121,#33122,#33123,#33124,
#33125,#33126,#33127,#33128,#33129,#33130,#33131,#33132,#33133,#33134,#33135,
#33136,#33137,#33138,#33139,#33140,#33141,#33142,#33143,#33144,#33145,#33146,
#33147,#33148,#33149,#33150,#33151,#33152,#33153,#33154,#33155,#33156,#33157,
#33158,#33159,#33160,#33161,#33162,#33163,#33164,#33165,#33166,#33167,#33168,
#33169,#33170,#33171,#33172,#33173,#33174,#33175,#33176,#33177,#33178,#33179,
#33180,#33181,#33182,#33183,#33184,#33185,#33186,#33187,#33188,#33189,#33190,
#33191,#33192,#33193,#33194,#33195,#33196,#33197,#33198,#33199,#33200,#33201,
#33202,#33203,#33204,#33205,#33206,#33207,#33208,#33209,#33210,#33211,#33212,
#33213,#33214,#33215,#33216,#33217,#33218,#33219,#33220,#33221,#33222,#33223,
#33224,#33225,#33226,#33227,#33228,#33229,#33230,#33231,#33232,#33233,#33234,
#33235,#33236,#33237,#33238,#33239,#33240,#33241,#33242,#33243,#33244,#33245,
#33246,#33247,#33248,#33249,#33250,#33251,#33252,#33253,#33254,#33255,#33256,
#33257,#33258,#33259,#33260,#33261,#33262,#33263,#33264,#33265,#33266,#33267,
#33268,#33269,#33270,#33271,#33272,#33273,#33274,#33275,#33276,#33277,#33278,
#33279,#33280,#33281,#33282,#33283)),.UNSPECIFIED.,.F.,.F.,.F.)
B_SPLINE_SURFACE_WITH_KNOTS((2,2),(3,2,2,2,2,2,2,2,2,2,2,2,2,2,2,2,2,2,
2,2,2,2,2,2,2,2,2,2,2,2,2,2,2,2,2,2,2,2,2,2,2,2,2,2,2,2,2,2,2,2,2,2,2,2,
2,2,2,2,2,2,2,2,2,2,2,2,2,2,2,2,2,2,2,2,2,2,2,2,2,2,2,2,2,2,2,2,2,2,2,2,
2,2,2,2,2,2,2,2,2,2,2,2,2,2,2,2,2,2,2,2,2,2,2,2,2,2,2,2,2,2,2,2,2,2,2,2,
2,2,2,2,2,2,2,2,2,2,2,2,2,2,2,2,2,2,2,2,2,2,2,2,2,2,2,2,2,2,2,2,2,3),(0.,
1.00001332089252),(0.,0.00617283950617284,0.0123456790123457,0.0185185185185185,
0.0246913580246914,0.0308641975308642,0.037037037037037,0.0432098765432099,
0.0493827160493827,0.0555555555555556,0.0617283950617284,0.0679012345679012,
0.0740740740740741,0.0802469135802469,0.0864197530864197,0.0925925925925926,
0.0987654320987654,0.104938271604938,0.111111111111111,0.117283950617284,
0.123456790123457,0.12962962962963,0.135802469135802,0.141975308641975,
0.148148148148148,0.154320987654321,0.160493827160494,0.166666666666667,
0.172839506172839,0.179012345679012,0.185185185185185,0.191358024691358,
0.197530864197531,0.203703703703704,0.209876543209877,0.216049382716049,
0.222222222222222,0.228395061728395,0.234567901234568,0.240740740740741,
0.246913580246914,0.253086419753086,0.259259259259259,0.265432098765432,
0.271604938271605,0.277777777777778,0.283950617283951,0.290123456790123,
0.296296296296296,0.302469135802469,0.308641975308642,0.314814814814815,
0.320987654320988,0.327160493827161,0.333333333333333,0.339506172839506,
0.345679012345679,0.351851851851852,0.358024691358025,0.364197530864198,
0.37037037037037,0.376543209876543,0.382716049382716,0.388888888888889,
0.395061728395062,0.401234567901235,0.407407407407407,0.41358024691358,
0.419753086419753,0.425925925925926,0.432098765432099,0.438271604938272,
0.444444444444444,0.450617283950617,0.45679012345679,0.462962962962963,
0.469135802469136,0.475308641975309,0.481481481481481,0.487654320987654,
0.493827160493827,0.5,0.506172839506173,0.512345679012346,0.518518518518518,
0.524691358024691,0.530864197530864,0.537037037037037,0.54320987654321,
0.549382716049383,0.555555555555556,0.561728395061728,0.567901234567901,
0.574074074074074,0.580246913580247,0.58641975308642,0.592592592592593,
0.598765432098765,0.604938271604938,0.611111111111111,0.617283950617284,
0.623456790123457,0.62962962962963,0.635802469135803,0.641975308641975,
0.648148148148148,0.654320987654321,0.660493827160494,0.666666666666667,
0.672839506172839,0.679012345679012,0.685185185185185,0.691358024691358,
0.697530864197531,0.703703703703704,0.709876543209877,0.716049382716049,
0.722222222222222,0.728395061728395,0.734567901234568,0.740740740740741,
0.746913580246914,0.753086419753086,0.759259259259259,0.765432098765432,
0.771604938271605,0.777777777777778,0.783950617283951,0.790123456790123,
0.796296296296296,0.802469135802469,0.808641975308642,0.814814814814815,
0.820987654320988,0.827160493827161,0.833333333333333,0.839506172839506,
0.845679012345679,0.851851851851852,0.858024691358025,0.864197530864197,
0.87037037037037,0.876543209876543,0.882716049382716,0.888888888888889,
0.895061728395062,0.901234567901235,0.907407407407407,0.91358024691358,
0.919753086419753,0.925925925925926,0.932098765432099,0.938271604938272,
0.944444444444444,0.950617283950617,0.95679012345679,0.962962962962963,
0.969135802469136,0.975308641975309,0.977791440774828),.UNSPECIFIED.)
GEOMETRIC_REPRESENTATION_ITEM()
RATIONAL_B_SPLINE_SURFACE(((1.,0.866025403784439,1.,0.866025403784439,1.,
0.866025403784439,1.,0.866025403784439,1.,0.866025403784439,1.,0.866025403784439,
1.,0.866025403784439,1.,0.866025403784439,1.,0.866025403784439,1.,0.866025403784439,
1.,0.866025403784439,1.,0.866025403784439,1.,0.866025403784439,1.,0.866025403784439,
1.,0.866025403784439,1.,0.866025403784439,1.,0.866025403784439,1.,0.866025403784439,
1.,0.866025403784439,1.,0.866025403784439,1.,0.866025403784439,1.,0.866025403784439,
1.,0.866025403784439,1.,0.866025403784439,1.,0.866025403784439,1.,0.866025403784439,
1.,0.866025403784439,1.,0.866025403784439,1.,0.866025403784439,1.,0.866025403784439,
1.,0.866025403784439,1.,0.866025403784439,1.,0.866025403784439,1.,0.866025403784439,
1.,0.866025403784439,1.,0.866025403784439,1.,0.866025403784439,1.,0.866025403784439,
1.,0.866025403784439,1.,0.866025403784439,1.,0.866025403784439,1.,0.866025403784439,
1.,0.866025403784439,1.,0.866025403784439,1.,0.866025403784439,1.,0.866025403784439,
1.,0.866025403784439,1.,0.866025403784439,1.,0.866025403784439,1.,0.866025403784439,
1.,0.866025403784439,1.,0.866025403784439,1.,0.866025403784439,1.,0.866025403784439,
1.,0.866025403784439,1.,0.866025403784439,1.,0.866025403784439,1.,0.866025403784439,
1.,0.866025403784439,1.,0.866025403784439,1.,0.866025403784439,1.,0.866025403784439,
1.,0.866025403784439,1.,0.866025403784439,1.,0.866025403784439,1.,0.866025403784439,
1.,0.866025403784439,1.,0.866025403784439,1.,0.866025403784439,1.,0.866025403784439,
1.,0.866025403784439,1.,0.866025403784439,1.,0.866025403784439,1.,0.866025403784439,
1.,0.866025403784439,1.,0.866025403784439,1.,0.866025403784439,1.,0.866025403784439,
1.,0.866025403784439,1.,0.866025403784439,1.,0.866025403784439,1.,0.866025403784439,
1.,0.866025403784439,1.,0.866025403784439,1.,0.866025403784439,1.,0.866025403784439,
1.,0.866025403784439,1.,0.866025403784439,1.,0.866025403784439,1.,0.866025403784439,
1.,0.866025403784439,1.,0.866025403784439,1.,0.866025403784439,1.,0.866025403784439,
1.,0.866025403784439,1.,0.866025403784439,1.,0.866025403784439,1.,0.866025403784439,
1.,0.866025403784439,1.,0.866025403784439,1.,0.866025403784439,1.,0.866025403784439,
1.,0.866025403784439,1.,0.866025403784439,1.,0.866025403784439,1.,0.866025403784439,
1.,0.866025403784439,1.,0.866025403784439,1.,0.866025403784439,1.,0.866025403784439,
1.,0.866025403784439,1.,0.866025403784439,1.,0.866025403784439,1.,0.866025403784439,
1.,0.866025403784439,1.,0.866025403784439,1.,0.866025403784439,1.,0.866025403784439,
1.,0.866025403784439,1.,0.866025403784439,1.,0.866025403784439,1.,0.866025403784439,
1.,0.866025403784439,1.,0.866025403784439,1.,0.866025403784439,1.,0.866025403784439,
1.,0.866025403784439,1.,0.866025403784439,1.,0.866025403784439,1.,0.866025403784439,
1.,0.866025403784439,1.,0.866025403784439,1.,0.866025403784439,1.,0.866025403784439,
1.,0.866025403784439,1.,0.866025403784439,1.,0.866025403784439,1.,0.866025403784439,
1.,0.866025403784439,1.,0.866025403784439,1.,0.866025403784439,1.,0.866025403784439,
1.,0.866025403784439,1.,0.866025403784439,1.,0.866025403784439,1.,0.866025403784439,
1.,0.866025403784439,1.,0.866025403784439,1.,0.866025403784439,1.,0.866025403784439,
1.,0.866025403784439,1.,0.866025403784439,1.,0.866025403784439,1.,0.866025403784439,
1.,0.866025403784439,1.,0.866025403784439,1.,0.866025403784439,1.,0.866025403784439,
1.,0.946113621402695,0.935574890499137),(1.,0.866025403784439,1.,0.866025403784439,
1.,0.866025403784439,1.,0.866025403784439,1.,0.866025403784439,1.,0.866025403784439,
1.,0.866025403784439,1.,0.866025403784439,1.,0.866025403784439,1.,0.866025403784439,
1.,0.866025403784439,1.,0.866025403784439,1.,0.866025403784439,1.,0.866025403784439,
1.,0.866025403784439,1.,0.866025403784439,1.,0.866025403784439,1.,0.866025403784439,
1.,0.866025403784439,1.,0.866025403784439,1.,0.866025403784439,1.,0.866025403784439,
1.,0.866025403784439,1.,0.866025403784439,1.,0.866025403784439,1.,0.866025403784439,
1.,0.866025403784439,1.,0.866025403784439,1.,0.866025403784439,1.,0.866025403784439,
1.,0.866025403784439,1.,0.866025403784439,1.,0.866025403784439,1.,0.866025403784439,
1.,0.866025403784439,1.,0.866025403784439,1.,0.866025403784439,1.,0.866025403784439,
1.,0.866025403784439,1.,0.866025403784439,1.,0.866025403784439,1.,0.866025403784439,
1.,0.866025403784439,1.,0.866025403784439,1.,0.866025403784439,1.,0.866025403784439,
1.,0.866025403784439,1.,0.866025403784439,1.,0.866025403784439,1.,0.866025403784439,
1.,0.866025403784439,1.,0.866025403784439,1.,0.866025403784439,1.,0.866025403784439,
1.,0.866025403784439,1.,0.866025403784439,1.,0.866025403784439,1.,0.866025403784439,
1.,0.866025403784439,1.,0.866025403784439,1.,0.866025403784439,1.,0.866025403784439,
1.,0.866025403784439,1.,0.866025403784439,1.,0.866025403784439,1.,0.866025403784439,
1.,0.866025403784439,1.,0.866025403784439,1.,0.866025403784439,1.,0.866025403784439,
1.,0.866025403784439,1.,0.866025403784439,1.,0.866025403784439,1.,0.866025403784439,
1.,0.866025403784439,1.,0.866025403784439,1.,0.866025403784439,1.,0.866025403784439,
1.,0.866025403784439,1.,0.866025403784439,1.,0.866025403784439,1.,0.866025403784439,
1.,0.866025403784439,1.,0.866025403784439,1.,0.866025403784439,1.,0.866025403784439,
1.,0.866025403784439,1.,0.866025403784439,1.,0.866025403784439,1.,0.866025403784439,
1.,0.866025403784439,1.,0.866025403784439,1.,0.866025403784439,1.,0.866025403784439,
1.,0.866025403784439,1.,0.866025403784439,1.,0.866025403784439,1.,0.866025403784439,
1.,0.866025403784439,1.,0.866025403784439,1.,0.866025403784439,1.,0.866025403784439,
1.,0.866025403784439,1.,0.866025403784439,1.,0.866025403784439,1.,0.866025403784439,
1.,0.866025403784439,1.,0.866025403784439,1.,0.866025403784439,1.,0.866025403784439,
1.,0.866025403784439,1.,0.866025403784439,1.,0.866025403784439,1.,0.866025403784439,
1.,0.866025403784439,1.,0.866025403784439,1.,0.866025403784439,1.,0.866025403784439,
1.,0.866025403784439,1.,0.866025403784439,1.,0.866025403784439,1.,0.866025403784439,
1.,0.866025403784439,1.,0.866025403784439,1.,0.866025403784439,1.,0.866025403784439,
1.,0.866025403784439,1.,0.866025403784439,1.,0.866025403784439,1.,0.866025403784439,
1.,0.866025403784439,1.,0.866025403784439,1.,0.866025403784439,1.,0.866025403784439,
1.,0.866025403784439,1.,0.866025403784439,1.,0.866025403784439,1.,0.866025403784439,
1.,0.866025403784439,1.,0.866025403784439,1.,0.866025403784439,1.,0.866025403784439,
1.,0.866025403784439,1.,0.866025403784439,1.,0.866025403784439,1.,0.866025403784439,
1.,0.866025403784439,1.,0.866025403784439,1.,0.866025403784439,1.,0.866025403784439,
1.,0.866025403784439,1.,0.866025403784439,1.,0.866025403784439,1.,0.866025403784439,
1.,0.866025403784439,1.,0.866025403784439,1.,0.866025403784439,1.,0.866025403784439,
1.,0.946113621402695,0.935574890499137)))
REPRESENTATION_ITEM('')
SURFACE()
);
#300=(
BOUNDED_SURFACE()
B_SPLINE_SURFACE(1,2,((#33589,#33590,#33591,#33592,#33593,#33594,#33595,
#33596,#33597,#33598,#33599,#33600,#33601,#33602,#33603,#33604,#33605,#33606,
#33607,#33608,#33609,#33610,#33611,#33612,#33613,#33614,#33615,#33616,#33617,
#33618,#33619,#33620,#33621,#33622,#33623,#33624,#33625,#33626,#33627,#33628,
#33629,#33630,#33631,#33632,#33633,#33634,#33635,#33636,#33637,#33638,#33639,
#33640,#33641,#33642,#33643,#33644,#33645,#33646,#33647,#33648,#33649,#33650,
#33651,#33652,#33653,#33654,#33655,#33656,#33657,#33658,#33659,#33660,#33661,
#33662,#33663,#33664,#33665,#33666,#33667,#33668,#33669,#33670,#33671,#33672,
#33673,#33674,#33675,#33676,#33677,#33678,#33679,#33680,#33681,#33682,#33683,
#33684,#33685,#33686,#33687,#33688,#33689,#33690,#33691,#33692,#33693,#33694,
#33695,#33696,#33697,#33698,#33699,#33700,#33701,#33702,#33703,#33704,#33705,
#33706,#33707,#33708,#33709,#33710,#33711,#33712,#33713,#33714,#33715,#33716,
#33717,#33718,#33719,#33720,#33721,#33722,#33723,#33724,#33725,#33726,#33727,
#33728,#33729,#33730,#33731,#33732,#33733,#33734,#33735,#33736,#33737,#33738,
#33739,#33740,#33741,#33742,#33743,#33744,#33745,#33746,#33747,#33748,#33749,
#33750,#33751,#33752,#33753,#33754,#33755,#33756,#33757,#33758,#33759,#33760,
#33761,#33762,#33763,#33764,#33765,#33766,#33767,#33768,#33769,#33770,#33771,
#33772,#33773,#33774,#33775,#33776,#33777,#33778,#33779,#33780,#33781,#33782,
#33783,#33784,#33785,#33786,#33787,#33788,#33789,#33790,#33791,#33792,#33793,
#33794,#33795,#33796,#33797,#33798,#33799,#33800,#33801,#33802,#33803,#33804,
#33805,#33806,#33807,#33808,#33809,#33810,#33811,#33812,#33813,#33814,#33815,
#33816,#33817,#33818,#33819,#33820,#33821,#33822,#33823,#33824,#33825,#33826,
#33827,#33828,#33829,#33830,#33831,#33832,#33833,#33834,#33835,#33836,#33837,
#33838,#33839,#33840,#33841,#33842,#33843,#33844,#33845,#33846,#33847,#33848,
#33849,#33850,#33851,#33852,#33853,#33854,#33855,#33856,#33857,#33858,#33859,
#33860,#33861,#33862,#33863,#33864,#33865,#33866,#33867,#33868,#33869,#33870,
#33871,#33872,#33873,#33874,#33875,#33876,#33877,#33878,#33879,#33880,#33881,
#33882,#33883,#33884,#33885,#33886,#33887,#33888,#33889,#33890,#33891,#33892,
#33893,#33894,#33895,#33896,#33897,#33898,#33899,#33900,#33901,#33902,#33903,
#33904,#33905,#33906,#33907,#33908,#33909),(#33910,#33911,#33912,#33913,
#33914,#33915,#33916,#33917,#33918,#33919,#33920,#33921,#33922,#33923,#33924,
#33925,#33926,#33927,#33928,#33929,#33930,#33931,#33932,#33933,#33934,#33935,
#33936,#33937,#33938,#33939,#33940,#33941,#33942,#33943,#33944,#33945,#33946,
#33947,#33948,#33949,#33950,#33951,#33952,#33953,#33954,#33955,#33956,#33957,
#33958,#33959,#33960,#33961,#33962,#33963,#33964,#33965,#33966,#33967,#33968,
#33969,#33970,#33971,#33972,#33973,#33974,#33975,#33976,#33977,#33978,#33979,
#33980,#33981,#33982,#33983,#33984,#33985,#33986,#33987,#33988,#33989,#33990,
#33991,#33992,#33993,#33994,#33995,#33996,#33997,#33998,#33999,#34000,#34001,
#34002,#34003,#34004,#34005,#34006,#34007,#34008,#34009,#34010,#34011,#34012,
#34013,#34014,#34015,#34016,#34017,#34018,#34019,#34020,#34021,#34022,#34023,
#34024,#34025,#34026,#34027,#34028,#34029,#34030,#34031,#34032,#34033,#34034,
#34035,#34036,#34037,#34038,#34039,#34040,#34041,#34042,#34043,#34044,#34045,
#34046,#34047,#34048,#34049,#34050,#34051,#34052,#34053,#34054,#34055,#34056,
#34057,#34058,#34059,#34060,#34061,#34062,#34063,#34064,#34065,#34066,#34067,
#34068,#34069,#34070,#34071,#34072,#34073,#34074,#34075,#34076,#34077,#34078,
#34079,#34080,#34081,#34082,#34083,#34084,#34085,#34086,#34087,#34088,#34089,
#34090,#34091,#34092,#34093,#34094,#34095,#34096,#34097,#34098,#34099,#34100,
#34101,#34102,#34103,#34104,#34105,#34106,#34107,#34108,#34109,#34110,#34111,
#34112,#34113,#34114,#34115,#34116,#34117,#34118,#34119,#34120,#34121,#34122,
#34123,#34124,#34125,#34126,#34127,#34128,#34129,#34130,#34131,#34132,#34133,
#34134,#34135,#34136,#34137,#34138,#34139,#34140,#34141,#34142,#34143,#34144,
#34145,#34146,#34147,#34148,#34149,#34150,#34151,#34152,#34153,#34154,#34155,
#34156,#34157,#34158,#34159,#34160,#34161,#34162,#34163,#34164,#34165,#34166,
#34167,#34168,#34169,#34170,#34171,#34172,#34173,#34174,#34175,#34176,#34177,
#34178,#34179,#34180,#34181,#34182,#34183,#34184,#34185,#34186,#34187,#34188,
#34189,#34190,#34191,#34192,#34193,#34194,#34195,#34196,#34197,#34198,#34199,
#34200,#34201,#34202,#34203,#34204,#34205,#34206,#34207,#34208,#34209,#34210,
#34211,#34212,#34213,#34214,#34215,#34216,#34217,#34218,#34219,#34220,#34221,
#34222,#34223,#34224,#34225,#34226,#34227,#34228,#34229,#34230)),
 .UNSPECIFIED.,.F.,.F.,.F.)
B_SPLINE_SURFACE_WITH_KNOTS((2,2),(3,2,2,2,2,2,2,2,2,2,2,2,2,2,2,2,2,2,
2,2,2,2,2,2,2,2,2,2,2,2,2,2,2,2,2,2,2,2,2,2,2,2,2,2,2,2,2,2,2,2,2,2,2,2,
2,2,2,2,2,2,2,2,2,2,2,2,2,2,2,2,2,2,2,2,2,2,2,2,2,2,2,2,2,2,2,2,2,2,2,2,
2,2,2,2,2,2,2,2,2,2,2,2,2,2,2,2,2,2,2,2,2,2,2,2,2,2,2,2,2,2,2,2,2,2,2,2,
2,2,2,2,2,2,2,2,2,2,2,2,2,2,2,2,2,2,2,2,2,2,2,2,2,2,2,2,2,2,2,2,2,2,3),
(-0.000321975171240205,1.),(0.,0.00617283950617284,0.0123456790123457,0.0185185185185185,
0.0246913580246914,0.0308641975308642,0.037037037037037,0.0432098765432099,
0.0493827160493827,0.0555555555555556,0.0617283950617284,0.0679012345679012,
0.0740740740740741,0.0802469135802469,0.0864197530864197,0.0925925925925926,
0.0987654320987654,0.104938271604938,0.111111111111111,0.117283950617284,
0.123456790123457,0.12962962962963,0.135802469135802,0.141975308641975,
0.148148148148148,0.154320987654321,0.160493827160494,0.166666666666667,
0.172839506172839,0.179012345679012,0.185185185185185,0.191358024691358,
0.197530864197531,0.203703703703704,0.209876543209877,0.216049382716049,
0.222222222222222,0.228395061728395,0.234567901234568,0.240740740740741,
0.246913580246914,0.253086419753086,0.259259259259259,0.265432098765432,
0.271604938271605,0.277777777777778,0.283950617283951,0.290123456790123,
0.296296296296296,0.302469135802469,0.308641975308642,0.314814814814815,
0.320987654320988,0.327160493827161,0.333333333333333,0.339506172839506,
0.345679012345679,0.351851851851852,0.358024691358025,0.364197530864198,
0.37037037037037,0.376543209876543,0.382716049382716,0.388888888888889,
0.395061728395062,0.401234567901235,0.407407407407407,0.41358024691358,
0.419753086419753,0.425925925925926,0.432098765432099,0.438271604938272,
0.444444444444444,0.450617283950617,0.45679012345679,0.462962962962963,
0.469135802469136,0.475308641975309,0.481481481481481,0.487654320987654,
0.493827160493827,0.5,0.506172839506173,0.512345679012346,0.518518518518518,
0.524691358024691,0.530864197530864,0.537037037037037,0.54320987654321,
0.549382716049383,0.555555555555556,0.561728395061728,0.567901234567901,
0.574074074074074,0.580246913580247,0.58641975308642,0.592592592592593,
0.598765432098765,0.604938271604938,0.611111111111111,0.617283950617284,
0.623456790123457,0.62962962962963,0.635802469135803,0.641975308641975,
0.648148148148148,0.654320987654321,0.660493827160494,0.666666666666667,
0.672839506172839,0.679012345679012,0.685185185185185,0.691358024691358,
0.697530864197531,0.703703703703704,0.709876543209877,0.716049382716049,
0.722222222222222,0.728395061728395,0.734567901234568,0.740740740740741,
0.746913580246914,0.753086419753086,0.759259259259259,0.765432098765432,
0.771604938271605,0.777777777777778,0.783950617283951,0.790123456790123,
0.796296296296296,0.802469135802469,0.808641975308642,0.814814814814815,
0.820987654320988,0.827160493827161,0.833333333333333,0.839506172839506,
0.845679012345679,0.851851851851852,0.858024691358025,0.864197530864197,
0.87037037037037,0.876543209876543,0.882716049382716,0.888888888888889,
0.895061728395062,0.901234567901235,0.907407407407407,0.91358024691358,
0.919753086419753,0.925925925925926,0.932098765432099,0.938271604938272,
0.944444444444444,0.950617283950617,0.95679012345679,0.962962962962963,
0.969135802469136,0.975308641975309,0.977791393533952,0.987569307469292),
 .UNSPECIFIED.)
GEOMETRIC_REPRESENTATION_ITEM()
RATIONAL_B_SPLINE_SURFACE(((1.,0.866025403784439,1.,0.866025403784439,1.,
0.866025403784439,1.,0.866025403784439,1.,0.866025403784439,1.,0.866025403784439,
1.,0.866025403784439,1.,0.866025403784439,1.,0.866025403784439,1.,0.866025403784439,
1.,0.866025403784439,1.,0.866025403784439,1.,0.866025403784439,1.,0.866025403784439,
1.,0.866025403784439,1.,0.866025403784439,1.,0.866025403784439,1.,0.866025403784439,
1.,0.866025403784439,1.,0.866025403784439,1.,0.866025403784439,1.,0.866025403784439,
1.,0.866025403784439,1.,0.866025403784439,1.,0.866025403784439,1.,0.866025403784439,
1.,0.866025403784439,1.,0.866025403784439,1.,0.866025403784439,1.,0.866025403784439,
1.,0.866025403784439,1.,0.866025403784439,1.,0.866025403784439,1.,0.866025403784439,
1.,0.866025403784439,1.,0.866025403784439,1.,0.866025403784439,1.,0.866025403784439,
1.,0.866025403784439,1.,0.866025403784439,1.,0.866025403784439,1.,0.866025403784439,
1.,0.866025403784439,1.,0.866025403784439,1.,0.866025403784439,1.,0.866025403784439,
1.,0.866025403784439,1.,0.866025403784439,1.,0.866025403784439,1.,0.866025403784439,
1.,0.866025403784439,1.,0.866025403784439,1.,0.866025403784439,1.,0.866025403784439,
1.,0.866025403784439,1.,0.866025403784439,1.,0.866025403784439,1.,0.866025403784439,
1.,0.866025403784439,1.,0.866025403784439,1.,0.866025403784439,1.,0.866025403784439,
1.,0.866025403784439,1.,0.866025403784439,1.,0.866025403784439,1.,0.866025403784439,
1.,0.866025403784439,1.,0.866025403784439,1.,0.866025403784439,1.,0.866025403784439,
1.,0.866025403784439,1.,0.866025403784439,1.,0.866025403784439,1.,0.866025403784439,
1.,0.866025403784439,1.,0.866025403784439,1.,0.866025403784439,1.,0.866025403784439,
1.,0.866025403784439,1.,0.866025403784439,1.,0.866025403784439,1.,0.866025403784439,
1.,0.866025403784439,1.,0.866025403784439,1.,0.866025403784439,1.,0.866025403784439,
1.,0.866025403784439,1.,0.866025403784439,1.,0.866025403784439,1.,0.866025403784439,
1.,0.866025403784439,1.,0.866025403784439,1.,0.866025403784439,1.,0.866025403784439,
1.,0.866025403784439,1.,0.866025403784439,1.,0.866025403784439,1.,0.866025403784439,
1.,0.866025403784439,1.,0.866025403784439,1.,0.866025403784439,1.,0.866025403784439,
1.,0.866025403784439,1.,0.866025403784439,1.,0.866025403784439,1.,0.866025403784439,
1.,0.866025403784439,1.,0.866025403784439,1.,0.866025403784439,1.,0.866025403784439,
1.,0.866025403784439,1.,0.866025403784439,1.,0.866025403784439,1.,0.866025403784439,
1.,0.866025403784439,1.,0.866025403784439,1.,0.866025403784439,1.,0.866025403784439,
1.,0.866025403784439,1.,0.866025403784439,1.,0.866025403784439,1.,0.866025403784439,
1.,0.866025403784439,1.,0.866025403784439,1.,0.866025403784439,1.,0.866025403784439,
1.,0.866025403784439,1.,0.866025403784439,1.,0.866025403784439,1.,0.866025403784439,
1.,0.866025403784439,1.,0.866025403784439,1.,0.866025403784439,1.,0.866025403784439,
1.,0.866025403784439,1.,0.866025403784439,1.,0.866025403784439,1.,0.866025403784439,
1.,0.866025403784439,1.,0.866025403784439,1.,0.866025403784439,1.,0.866025403784439,
1.,0.866025403784439,1.,0.866025403784439,1.,0.866025403784439,1.,0.866025403784439,
1.,0.866025403784439,1.,0.866025403784439,1.,0.866025403784439,1.,0.866025403784439,
1.,0.866025403784439,1.,0.866025403784439,1.,0.866025403784439,1.,0.866025403784439,
1.,0.866025403784439,1.,0.866025403784439,1.,0.866025403784439,1.,0.866025403784439,
1.,0.946114646713198,0.93557529156132,0.93557529156132,0.93557529156132),
(1.,0.866025403784439,1.,0.866025403784439,1.,0.866025403784439,1.,0.866025403784439,
1.,0.866025403784439,1.,0.866025403784439,1.,0.866025403784439,1.,0.866025403784439,
1.,0.866025403784439,1.,0.866025403784439,1.,0.866025403784439,1.,0.866025403784439,
1.,0.866025403784439,1.,0.866025403784439,1.,0.866025403784439,1.,0.866025403784439,
1.,0.866025403784439,1.,0.866025403784439,1.,0.866025403784439,1.,0.866025403784439,
1.,0.866025403784439,1.,0.866025403784439,1.,0.866025403784439,1.,0.866025403784439,
1.,0.866025403784439,1.,0.866025403784439,1.,0.866025403784439,1.,0.866025403784439,
1.,0.866025403784439,1.,0.866025403784439,1.,0.866025403784439,1.,0.866025403784439,
1.,0.866025403784439,1.,0.866025403784439,1.,0.866025403784439,1.,0.866025403784439,
1.,0.866025403784439,1.,0.866025403784439,1.,0.866025403784439,1.,0.866025403784439,
1.,0.866025403784439,1.,0.866025403784439,1.,0.866025403784439,1.,0.866025403784439,
1.,0.866025403784439,1.,0.866025403784439,1.,0.866025403784439,1.,0.866025403784439,
1.,0.866025403784439,1.,0.866025403784439,1.,0.866025403784439,1.,0.866025403784439,
1.,0.866025403784439,1.,0.866025403784439,1.,0.866025403784439,1.,0.866025403784439,
1.,0.866025403784439,1.,0.866025403784439,1.,0.866025403784439,1.,0.866025403784439,
1.,0.866025403784439,1.,0.866025403784439,1.,0.866025403784439,1.,0.866025403784439,
1.,0.866025403784439,1.,0.866025403784439,1.,0.866025403784439,1.,0.866025403784439,
1.,0.866025403784439,1.,0.866025403784439,1.,0.866025403784439,1.,0.866025403784439,
1.,0.866025403784439,1.,0.866025403784439,1.,0.866025403784439,1.,0.866025403784439,
1.,0.866025403784439,1.,0.866025403784439,1.,0.866025403784439,1.,0.866025403784439,
1.,0.866025403784439,1.,0.866025403784439,1.,0.866025403784439,1.,0.866025403784439,
1.,0.866025403784439,1.,0.866025403784439,1.,0.866025403784439,1.,0.866025403784439,
1.,0.866025403784439,1.,0.866025403784439,1.,0.866025403784439,1.,0.866025403784439,
1.,0.866025403784439,1.,0.866025403784439,1.,0.866025403784439,1.,0.866025403784439,
1.,0.866025403784439,1.,0.866025403784439,1.,0.866025403784439,1.,0.866025403784439,
1.,0.866025403784439,1.,0.866025403784439,1.,0.866025403784439,1.,0.866025403784439,
1.,0.866025403784439,1.,0.866025403784439,1.,0.866025403784439,1.,0.866025403784439,
1.,0.866025403784439,1.,0.866025403784439,1.,0.866025403784439,1.,0.866025403784439,
1.,0.866025403784439,1.,0.866025403784439,1.,0.866025403784439,1.,0.866025403784439,
1.,0.866025403784439,1.,0.866025403784439,1.,0.866025403784439,1.,0.866025403784439,
1.,0.866025403784439,1.,0.866025403784439,1.,0.866025403784439,1.,0.866025403784439,
1.,0.866025403784439,1.,0.866025403784439,1.,0.866025403784439,1.,0.866025403784439,
1.,0.866025403784439,1.,0.866025403784439,1.,0.866025403784439,1.,0.866025403784439,
1.,0.866025403784439,1.,0.866025403784439,1.,0.866025403784439,1.,0.866025403784439,
1.,0.866025403784439,1.,0.866025403784439,1.,0.866025403784439,1.,0.866025403784439,
1.,0.866025403784439,1.,0.866025403784439,1.,0.866025403784439,1.,0.866025403784439,
1.,0.866025403784439,1.,0.866025403784439,1.,0.866025403784439,1.,0.866025403784439,
1.,0.866025403784439,1.,0.866025403784439,1.,0.866025403784439,1.,0.866025403784439,
1.,0.866025403784439,1.,0.866025403784439,1.,0.866025403784439,1.,0.866025403784439,
1.,0.866025403784439,1.,0.866025403784439,1.,0.946114646713198,0.93557529156132,
0.93557529156132,0.93557529156132)))
REPRESENTATION_ITEM('')
SURFACE()
);
#301=CONICAL_SURFACE('',#11717,10.985,0.785398163397459);
#302=CONICAL_SURFACE('',#11722,2.155,0.78539816339745);
#303=CONICAL_SURFACE('',#11725,2.155,0.78539816339745);
#304=CONICAL_SURFACE('',#11728,2.155,0.78539816339745);
#305=CONICAL_SURFACE('',#11731,2.155,0.78539816339745);
#306=CONICAL_SURFACE('',#11774,1.99200000000004,0.785398163397448);
#307=CONICAL_SURFACE('',#11777,1.99200000000004,0.785398163397448);
#308=CONICAL_SURFACE('',#11780,0.975999999999995,0.78539816339745);
#309=CONICAL_SURFACE('',#11792,3.175,0.785398163397427);
#310=CONICAL_SURFACE('',#11795,3.175,0.785398163397427);
#311=CONICAL_SURFACE('',#11798,3.175,0.785398163397427);
#312=CONICAL_SURFACE('',#11801,3.175,0.785398163397427);
#313=CONICAL_SURFACE('',#11889,10.9505,0.785398163397447);
#314=CONICAL_SURFACE('',#11896,10.9505,0.785398163397447);
#315=CONICAL_SURFACE('',#11911,2.110288568297,0.5235987755983);
#316=CONICAL_SURFACE('',#11914,2.110288568297,0.5235987755983);
#317=CONICAL_SURFACE('',#11919,4.27,1.0471975511966);
#318=CONICAL_SURFACE('',#11927,4.27,1.0471975511966);
#319=CONICAL_SURFACE('',#11939,7.75,0.785398163397447);
#320=CONICAL_SURFACE('',#11945,8.,0.785398163397448);
#321=CONICAL_SURFACE('',#11958,4.01780239848197,0.78539816339745);
#322=CONICAL_SURFACE('',#11962,3.26912128048043,0.78539816339745);
#323=CONICAL_SURFACE('',#11968,2.5,0.785398163397447);
#324=CONICAL_SURFACE('',#11979,3.26912128048043,0.78539816339745);
#325=CONICAL_SURFACE('',#12394,2.27961999999998,0.833832411830472);
#326=STYLED_ITEM('',(#36596),#358);
#327=STYLED_ITEM('',(#36596),#359);
#328=STYLED_ITEM('',(#36596),#360);
#329=STYLED_ITEM('',(#36596),#361);
#330=STYLED_ITEM('',(#36596),#362);
#331=STYLED_ITEM('',(#36596),#363);
#332=STYLED_ITEM('',(#36596),#364);
#333=STYLED_ITEM('',(#36596),#365);
#334=STYLED_ITEM('',(#36597),#366);
#335=STYLED_ITEM('',(#36598),#367);
#336=STYLED_ITEM('',(#36599),#368);
#337=STYLED_ITEM('',(#36596),#369);
#338=STYLED_ITEM('',(#36596),#370);
#339=STYLED_ITEM('',(#36596),#371);
#340=STYLED_ITEM('',(#36596),#372);
#341=STYLED_ITEM('',(#36596),#373);
#342=STYLED_ITEM('',(#36596),#374);
#343=STYLED_ITEM('',(#36596),#375);
#344=STYLED_ITEM('',(#36596),#376);
#345=STYLED_ITEM('',(#36596),#377);
#346=STYLED_ITEM('',(#36596),#378);
#347=STYLED_ITEM('',(#36596),#379);
#348=STYLED_ITEM('',(#36596),#380);
#349=STYLED_ITEM('',(#36596),#381);
#350=STYLED_ITEM('',(#36598),#382);
#351=STYLED_ITEM('',(#36598),#383);
#352=STYLED_ITEM('',(#36596),#384);
#353=STYLED_ITEM('',(#36598),#385);
#354=STYLED_ITEM('',(#36597),#386);
#355=STYLED_ITEM('',(#36596),#387);
#356=STYLED_ITEM('',(#36596),#388);
#357=STYLED_ITEM('',(#36596),#389);
#358=MANIFOLD_SOLID_BREP('Body1',#11262);
#359=MANIFOLD_SOLID_BREP('Body2',#11263);
#360=MANIFOLD_SOLID_BREP('Body3',#11264);
#361=MANIFOLD_SOLID_BREP('Body4',#11265);
#362=MANIFOLD_SOLID_BREP('Body5',#11266);
#363=MANIFOLD_SOLID_BREP('Body6',#11267);
#364=MANIFOLD_SOLID_BREP('Body7',#11268);
#365=MANIFOLD_SOLID_BREP('Body8',#11269);
#366=MANIFOLD_SOLID_BREP('Body1',#11270);
#367=MANIFOLD_SOLID_BREP('Body1',#11271);
#368=MANIFOLD_SOLID_BREP('Body1',#11272);
#369=MANIFOLD_SOLID_BREP('Body1',#11273);
#370=MANIFOLD_SOLID_BREP('Body2',#11274);
#371=MANIFOLD_SOLID_BREP('Body3',#11275);
#372=MANIFOLD_SOLID_BREP('Body4',#11276);
#373=MANIFOLD_SOLID_BREP('Body5',#11277);
#374=MANIFOLD_SOLID_BREP('Body6',#11278);
#375=MANIFOLD_SOLID_BREP('Body7',#11279);
#376=MANIFOLD_SOLID_BREP('Body8',#11280);
#377=MANIFOLD_SOLID_BREP('Body9',#11281);
#378=MANIFOLD_SOLID_BREP('Body10',#11282);
#379=MANIFOLD_SOLID_BREP('Body11',#11283);
#380=MANIFOLD_SOLID_BREP('Body12',#11284);
#381=MANIFOLD_SOLID_BREP('Body13',#11285);
#382=MANIFOLD_SOLID_BREP('Body1',#11286);
#383=MANIFOLD_SOLID_BREP('Body1',#11287);
#384=MANIFOLD_SOLID_BREP('Body1',#11288);
#385=MANIFOLD_SOLID_BREP('Body1',#11289);
#386=MANIFOLD_SOLID_BREP('Body1',#11290);
#387=MANIFOLD_SOLID_BREP('Body1',#11291);
#388=MANIFOLD_SOLID_BREP('Body1',#11292);
#389=MANIFOLD_SOLID_BREP('Body1',#11293);
#390=PLANE('',#11458);
#391=PLANE('',#11459);
#392=PLANE('',#11460);
#393=PLANE('',#11461);
#394=PLANE('',#11462);
#395=PLANE('',#11463);
#396=PLANE('',#11464);
#397=PLANE('',#11465);
#398=PLANE('',#11466);
#399=PLANE('',#11467);
#400=PLANE('',#11468);
#401=PLANE('',#11469);
#402=PLANE('',#11470);
#403=PLANE('',#11471);
#404=PLANE('',#11472);
#405=PLANE('',#11473);
#406=PLANE('',#11474);
#407=PLANE('',#11475);
#408=PLANE('',#11494);
#409=PLANE('',#11495);
#410=PLANE('',#11496);
#411=PLANE('',#11497);
#412=PLANE('',#11498);
#413=PLANE('',#11499);
#414=PLANE('',#11500);
#415=PLANE('',#11501);
#416=PLANE('',#11502);
#417=PLANE('',#11503);
#418=PLANE('',#11504);
#419=PLANE('',#11505);
#420=PLANE('',#11506);
#421=PLANE('',#11507);
#422=PLANE('',#11508);
#423=PLANE('',#11509);
#424=PLANE('',#11510);
#425=PLANE('',#11511);
#426=PLANE('',#11530);
#427=PLANE('',#11531);
#428=PLANE('',#11532);
#429=PLANE('',#11533);
#430=PLANE('',#11534);
#431=PLANE('',#11535);
#432=PLANE('',#11536);
#433=PLANE('',#11537);
#434=PLANE('',#11538);
#435=PLANE('',#11539);
#436=PLANE('',#11540);
#437=PLANE('',#11541);
#438=PLANE('',#11542);
#439=PLANE('',#11543);
#440=PLANE('',#11544);
#441=PLANE('',#11545);
#442=PLANE('',#11546);
#443=PLANE('',#11547);
#444=PLANE('',#11566);
#445=PLANE('',#11567);
#446=PLANE('',#11568);
#447=PLANE('',#11569);
#448=PLANE('',#11570);
#449=PLANE('',#11571);
#450=PLANE('',#11572);
#451=PLANE('',#11573);
#452=PLANE('',#11574);
#453=PLANE('',#11575);
#454=PLANE('',#11576);
#455=PLANE('',#11577);
#456=PLANE('',#11578);
#457=PLANE('',#11579);
#458=PLANE('',#11580);
#459=PLANE('',#11581);
#460=PLANE('',#11582);
#461=PLANE('',#11583);
#462=PLANE('',#11736);
#463=PLANE('',#11737);
#464=PLANE('',#11744);
#465=PLANE('',#11745);
#466=PLANE('',#11746);
#467=PLANE('',#11747);
#468=PLANE('',#11748);
#469=PLANE('',#11749);
#470=PLANE('',#11750);
#471=PLANE('',#11754);
#472=PLANE('',#11755);
#473=PLANE('',#11758);
#474=PLANE('',#11761);
#475=PLANE('',#11764);
#476=PLANE('',#11767);
#477=PLANE('',#11773);
#478=PLANE('',#11785);
#479=PLANE('',#11786);
#480=PLANE('',#11787);
#481=PLANE('',#11788);
#482=PLANE('',#11815);
#483=PLANE('',#11816);
#484=PLANE('',#11817);
#485=PLANE('',#11818);
#486=PLANE('',#11819);
#487=PLANE('',#11820);
#488=PLANE('',#11821);
#489=PLANE('',#11822);
#490=PLANE('',#11823);
#491=PLANE('',#11824);
#492=PLANE('',#11825);
#493=PLANE('',#11826);
#494=PLANE('',#11834);
#495=PLANE('',#11837);
#496=PLANE('',#11840);
#497=PLANE('',#11843);
#498=PLANE('',#11846);
#499=PLANE('',#11847);
#500=PLANE('',#11848);
#501=PLANE('',#11850);
#502=PLANE('',#11851);
#503=PLANE('',#11854);
#504=PLANE('',#11855);
#505=PLANE('',#11856);
#506=PLANE('',#11857);
#507=PLANE('',#11873);
#508=PLANE('',#11874);
#509=PLANE('',#11875);
#510=PLANE('',#11876);
#511=PLANE('',#11877);
#512=PLANE('',#11878);
#513=PLANE('',#11879);
#514=PLANE('',#11880);
#515=PLANE('',#11881);
#516=PLANE('',#11882);
#517=PLANE('',#11883);
#518=PLANE('',#11884);
#519=PLANE('',#11885);
#520=PLANE('',#11886);
#521=PLANE('',#11894);
#522=PLANE('',#11898);
#523=PLANE('',#11908);
#524=PLANE('',#11909);
#525=PLANE('',#11917);
#526=PLANE('',#11918);
#527=PLANE('',#11921);
#528=PLANE('',#11922);
#529=PLANE('',#11923);
#530=PLANE('',#11924);
#531=PLANE('',#11925);
#532=PLANE('',#11928);
#533=PLANE('',#11947);
#534=PLANE('',#11948);
#535=PLANE('',#11960);
#536=PLANE('',#11961);
#537=PLANE('',#11981);
#538=PLANE('',#11982);
#539=PLANE('',#11983);
#540=PLANE('',#12010);
#541=PLANE('',#12011);
#542=PLANE('',#12012);
#543=PLANE('',#12013);
#544=PLANE('',#12014);
#545=PLANE('',#12018);
#546=PLANE('',#12019);
#547=PLANE('',#12020);
#548=PLANE('',#12021);
#549=PLANE('',#12022);
#550=PLANE('',#12023);
#551=PLANE('',#12024);
#552=PLANE('',#12025);
#553=PLANE('',#12026);
#554=PLANE('',#12030);
#555=PLANE('',#12031);
#556=PLANE('',#12032);
#557=PLANE('',#12033);
#558=PLANE('',#12034);
#559=PLANE('',#12035);
#560=PLANE('',#12036);
#561=PLANE('',#12037);
#562=PLANE('',#12038);
#563=PLANE('',#12039);
#564=PLANE('',#12040);
#565=PLANE('',#12041);
#566=PLANE('',#12042);
#567=PLANE('',#12043);
#568=PLANE('',#12044);
#569=PLANE('',#12045);
#570=PLANE('',#12046);
#571=PLANE('',#12047);
#572=PLANE('',#12051);
#573=PLANE('',#12052);
#574=PLANE('',#12053);
#575=PLANE('',#12054);
#576=PLANE('',#12055);
#577=PLANE('',#12056);
#578=PLANE('',#12057);
#579=PLANE('',#12058);
#580=PLANE('',#12059);
#581=PLANE('',#12060);
#582=PLANE('',#12061);
#583=PLANE('',#12062);
#584=PLANE('',#12063);
#585=PLANE('',#12067);
#586=PLANE('',#12068);
#587=PLANE('',#12069);
#588=PLANE('',#12070);
#589=PLANE('',#12071);
#590=PLANE('',#12074);
#591=PLANE('',#12075);
#592=PLANE('',#12076);
#593=PLANE('',#12077);
#594=PLANE('',#12078);
#595=PLANE('',#12079);
#596=PLANE('',#12080);
#597=PLANE('',#12081);
#598=PLANE('',#12082);
#599=PLANE('',#12085);
#600=PLANE('',#12086);
#601=PLANE('',#12087);
#602=PLANE('',#12088);
#603=PLANE('',#12089);
#604=PLANE('',#12090);
#605=PLANE('',#12091);
#606=PLANE('',#12092);
#607=PLANE('',#12093);
#608=PLANE('',#12094);
#609=PLANE('',#12095);
#610=PLANE('',#12096);
#611=PLANE('',#12097);
#612=PLANE('',#12098);
#613=PLANE('',#12099);
#614=PLANE('',#12100);
#615=PLANE('',#12101);
#616=PLANE('',#12102);
#617=PLANE('',#12103);
#618=PLANE('',#12106);
#619=PLANE('',#12107);
#620=PLANE('',#12108);
#621=PLANE('',#12109);
#622=PLANE('',#12110);
#623=PLANE('',#12111);
#624=PLANE('',#12112);
#625=PLANE('',#12113);
#626=PLANE('',#12114);
#627=PLANE('',#12115);
#628=PLANE('',#12116);
#629=PLANE('',#12117);
#630=PLANE('',#12119);
#631=PLANE('',#12125);
#632=PLANE('',#12127);
#633=PLANE('',#12132);
#634=PLANE('',#12139);
#635=PLANE('',#12140);
#636=PLANE('',#12141);
#637=PLANE('',#12142);
#638=PLANE('',#12143);
#639=PLANE('',#12144);
#640=PLANE('',#12145);
#641=PLANE('',#12146);
#642=PLANE('',#12153);
#643=PLANE('',#12154);
#644=PLANE('',#12155);
#645=PLANE('',#12156);
#646=PLANE('',#12163);
#647=PLANE('',#12164);
#648=PLANE('',#12165);
#649=PLANE('',#12166);
#650=PLANE('',#12167);
#651=PLANE('',#12168);
#652=PLANE('',#12169);
#653=PLANE('',#12170);
#654=PLANE('',#12171);
#655=PLANE('',#12175);
#656=PLANE('',#12179);
#657=PLANE('',#12183);
#658=PLANE('',#12187);
#659=PLANE('',#12188);
#660=PLANE('',#12195);
#661=PLANE('',#12197);
#662=PLANE('',#12202);
#663=PLANE('',#12210);
#664=PLANE('',#12211);
#665=PLANE('',#12213);
#666=PLANE('',#12218);
#667=PLANE('',#12221);
#668=PLANE('',#12224);
#669=PLANE('',#12227);
#670=PLANE('',#12230);
#671=PLANE('',#12235);
#672=PLANE('',#12239);
#673=PLANE('',#12258);
#674=PLANE('',#12262);
#675=PLANE('',#12266);
#676=PLANE('',#12270);
#677=PLANE('',#12289);
#678=PLANE('',#12293);
#679=PLANE('',#12303);
#680=PLANE('',#12307);
#681=PLANE('',#12311);
#682=PLANE('',#12315);
#683=PLANE('',#12319);
#684=PLANE('',#12323);
#685=PLANE('',#12327);
#686=PLANE('',#12331);
#687=PLANE('',#12341);
#688=PLANE('',#12345);
#689=PLANE('',#12349);
#690=PLANE('',#12353);
#691=PLANE('',#12357);
#692=PLANE('',#12358);
#693=PLANE('',#12378);
#694=PLANE('',#12382);
#695=PLANE('',#12386);
#696=PLANE('',#12390);
#697=PLANE('',#12391);
#698=PLANE('',#12392);
#699=PLANE('',#12401);
#700=PLANE('',#12404);
#701=PLANE('',#12405);
#702=PLANE('',#12406);
#703=PLANE('',#12407);
#704=PLANE('',#12408);
#705=PLANE('',#12409);
#706=PLANE('',#12410);
#707=PLANE('',#12411);
#708=PLANE('',#12412);
#709=PLANE('',#12413);
#710=PLANE('',#12414);
#711=PLANE('',#12415);
#712=PLANE('',#12416);
#713=PLANE('',#12417);
#714=ELLIPSE('',#11446,1.32158737874913,1.29894133639841);
#715=ELLIPSE('',#11448,1.32158737875847,1.29894133640388);
#716=ELLIPSE('',#11449,1.32158737877034,1.2989413364124);
#717=ELLIPSE('',#11451,1.32594775747344,1.30189938329286);
#718=ELLIPSE('',#11452,1.32594775747545,1.30189938329438);
#719=ELLIPSE('',#11454,1.32594775748252,1.30189938329882);
#720=ELLIPSE('',#11455,1.3259477575257,1.30189938332617);
#721=ELLIPSE('',#11457,1.32158737873925,1.29894133639057);
#722=ELLIPSE('',#11482,1.32158737875113,1.29894133639988);
#723=ELLIPSE('',#11484,1.32158737869327,1.29894133635907);
#724=ELLIPSE('',#11485,1.32158737875922,1.29894133640477);
#725=ELLIPSE('',#11487,1.32594775746793,1.3018993832892);
#726=ELLIPSE('',#11488,1.32594775746135,1.3018993832848);
#727=ELLIPSE('',#11490,1.32594775747089,1.30189938329139);
#728=ELLIPSE('',#11491,1.32594775751682,1.30189938332048);
#729=ELLIPSE('',#11493,1.32158737872551,1.29894133638101);
#730=ELLIPSE('',#11518,1.32158737874913,1.29894133639841);
#731=ELLIPSE('',#11520,1.32158737875847,1.29894133640388);
#732=ELLIPSE('',#11521,1.32158737877034,1.2989413364124);
#733=ELLIPSE('',#11523,1.32594775747344,1.30189938329286);
#734=ELLIPSE('',#11524,1.32594775747545,1.30189938329438);
#735=ELLIPSE('',#11526,1.32594775748252,1.30189938329882);
#736=ELLIPSE('',#11527,1.3259477575257,1.30189938332617);
#737=ELLIPSE('',#11529,1.32158737873925,1.29894133639057);
#738=ELLIPSE('',#11554,1.32158737871208,1.29894133637222);
#739=ELLIPSE('',#11556,1.32158737876063,1.29894133640545);
#740=ELLIPSE('',#11557,1.3215873787679,1.29894133641094);
#741=ELLIPSE('',#11559,1.32594775747229,1.30189938329206);
#742=ELLIPSE('',#11560,1.32594775746355,1.30189938328618);
#743=ELLIPSE('',#11562,1.3259477575216,1.30189938332397);
#744=ELLIPSE('',#11563,1.32594775751662,1.30189938332021);
#745=ELLIPSE('',#11565,1.32158737874161,1.29894133639227);
#746=ELLIPSE('',#11752,0.824782856622966,0.762000000000211);
#747=ELLIPSE('',#11753,0.824782856622431,0.761999999999637);
#748=ELLIPSE('',#11757,0.824782856622448,0.761999999999701);
#749=ELLIPSE('',#11760,0.824782856623037,0.762000000000206);
#750=ELLIPSE('',#11763,0.82478285662272,0.761999999999946);
#751=ELLIPSE('',#11766,0.824782856622662,0.761999999999831);
#752=ELLIPSE('',#11769,0.824782856622382,0.761999999999617);
#753=ELLIPSE('',#11771,0.824782856622497,0.761999999999736);
#754=ELLIPSE('',#11828,0.8247828566222,0.761999999999463);
#755=ELLIPSE('',#11829,0.824782856621912,0.761999999999204);
#756=ELLIPSE('',#11831,0.824782856622183,0.761999999999485);
#757=ELLIPSE('',#11833,0.824782856621664,0.761999999998966);
#758=ELLIPSE('',#11836,0.824782856622583,0.761999999999779);
#759=ELLIPSE('',#11839,0.824782856622534,0.761999999999738);
#760=ELLIPSE('',#11842,0.824782856623014,0.762000000000189);
#761=ELLIPSE('',#11845,0.824782856623095,0.762000000000223);
#762=B_SPLINE_CURVE_WITH_KNOTS('',3,(#15394,#15395,#15396,#15397),
 .UNSPECIFIED.,.F.,.F.,(4,4),(-0.496042203551295,-0.465357569002963),
 .UNSPECIFIED.);
#763=B_SPLINE_CURVE_WITH_KNOTS('',3,(#15400,#15401,#15402,#15403),
 .UNSPECIFIED.,.F.,.F.,(4,4),(-0.526726838099626,-0.496042203551295),
 .UNSPECIFIED.);
#764=B_SPLINE_CURVE_WITH_KNOTS('',3,(#15411,#15412,#15413,#15414,#15415,
#15416),.UNSPECIFIED.,.F.,.F.,(4,2,4),(0.465357569002967,0.496042203551295,
0.526726838099618),.UNSPECIFIED.);
#765=B_SPLINE_CURVE_WITH_KNOTS('',3,(#15424,#15425,#15426,#15427,#15428,
#15429),.UNSPECIFIED.,.F.,.F.,(4,2,4),(-0.526726838099624,-0.496042203551295,
-0.465357569002967),.UNSPECIFIED.);
#766=B_SPLINE_CURVE_WITH_KNOTS('',3,(#15437,#15438,#15439,#15440,#15441,
#15442),.UNSPECIFIED.,.F.,.F.,(4,2,4),(0.465357569002967,0.496042203551295,
0.526726838099618),.UNSPECIFIED.);
#767=B_SPLINE_CURVE_WITH_KNOTS('',3,(#15525,#15526,#15527,#15528),
 .UNSPECIFIED.,.F.,.F.,(4,4),(-0.496042203551295,-0.465357569002962),
 .UNSPECIFIED.);
#768=B_SPLINE_CURVE_WITH_KNOTS('',3,(#15531,#15532,#15533,#15534),
 .UNSPECIFIED.,.F.,.F.,(4,4),(-0.526726838099626,-0.496042203551295),
 .UNSPECIFIED.);
#769=B_SPLINE_CURVE_WITH_KNOTS('',3,(#15542,#15543,#15544,#15545,#15546,
#15547),.UNSPECIFIED.,.F.,.F.,(4,2,4),(0.465357569002975,0.496042203551295,
0.526726838099626),.UNSPECIFIED.);
#770=B_SPLINE_CURVE_WITH_KNOTS('',3,(#15555,#15556,#15557,#15558,#15559,
#15560),.UNSPECIFIED.,.F.,.F.,(4,2,4),(-0.526726838099632,-0.496042203551295,
-0.465357569002975),.UNSPECIFIED.);
#771=B_SPLINE_CURVE_WITH_KNOTS('',3,(#15568,#15569,#15570,#15571,#15572,
#15573),.UNSPECIFIED.,.F.,.F.,(4,2,4),(0.465357569002966,0.496042203551295,
0.526726838099617),.UNSPECIFIED.);
#772=B_SPLINE_CURVE_WITH_KNOTS('',3,(#15656,#15657,#15658,#15659),
 .UNSPECIFIED.,.F.,.F.,(4,4),(-0.496042203551295,-0.465357569002963),
 .UNSPECIFIED.);
#773=B_SPLINE_CURVE_WITH_KNOTS('',3,(#15662,#15663,#15664,#15665),
 .UNSPECIFIED.,.F.,.F.,(4,4),(-0.526726838099626,-0.496042203551295),
 .UNSPECIFIED.);
#774=B_SPLINE_CURVE_WITH_KNOTS('',3,(#15673,#15674,#15675,#15676,#15677,
#15678),.UNSPECIFIED.,.F.,.F.,(4,2,4),(0.465357569002967,0.496042203551295,
0.526726838099618),.UNSPECIFIED.);
#775=B_SPLINE_CURVE_WITH_KNOTS('',3,(#15686,#15687,#15688,#15689,#15690,
#15691),.UNSPECIFIED.,.F.,.F.,(4,2,4),(-0.526726838099624,-0.496042203551295,
-0.465357569002967),.UNSPECIFIED.);
#776=B_SPLINE_CURVE_WITH_KNOTS('',3,(#15699,#15700,#15701,#15702,#15703,
#15704),.UNSPECIFIED.,.F.,.F.,(4,2,4),(0.465357569002967,0.496042203551295,
0.526726838099618),.UNSPECIFIED.);
#777=B_SPLINE_CURVE_WITH_KNOTS('',3,(#15787,#15788,#15789,#15790),
 .UNSPECIFIED.,.F.,.F.,(4,4),(-0.496042203551296,-0.465357569002961),
 .UNSPECIFIED.);
#778=B_SPLINE_CURVE_WITH_KNOTS('',3,(#15793,#15794,#15795,#15796),
 .UNSPECIFIED.,.F.,.F.,(4,4),(-0.526726838099625,-0.496042203551296),
 .UNSPECIFIED.);
#779=B_SPLINE_CURVE_WITH_KNOTS('',3,(#15804,#15805,#15806,#15807,#15808,
#15809),.UNSPECIFIED.,.F.,.F.,(4,2,4),(0.465357569002966,0.496042203551297,
0.526726838099617),.UNSPECIFIED.);
#780=B_SPLINE_CURVE_WITH_KNOTS('',3,(#15817,#15818,#15819,#15820,#15821,
#15822),.UNSPECIFIED.,.F.,.F.,(4,2,4),(-0.526726838099632,-0.496042203551297,
-0.465357569002976),.UNSPECIFIED.);
#781=B_SPLINE_CURVE_WITH_KNOTS('',3,(#15830,#15831,#15832,#15833,#15834,
#15835),.UNSPECIFIED.,.F.,.F.,(4,2,4),(0.465357569002975,0.496042203551296,
0.526726838099625),.UNSPECIFIED.);
#782=B_SPLINE_CURVE_WITH_KNOTS('',3,(#15912,#15913,#15914,#15915,#15916,
#15917,#15918,#15919,#15920,#15921,#15922,#15923,#15924,#15925,#15926,#15927,
#15928,#15929,#15930,#15931,#15932,#15933,#15934,#15935),.UNSPECIFIED.,
 .F.,.F.,(4,2,2,2,2,2,2,2,2,2,2,4),(21.735148043229,21.8036569750145,21.87839314446,
21.9507157433963,22.0264533977592,22.1003572095216,22.1735114412091,22.2494464904211,
22.3225068859442,22.3979222493655,22.4408998473177,22.4837420617588),
 .UNSPECIFIED.);
#783=B_SPLINE_CURVE_WITH_KNOTS('',3,(#15938,#15939,#15940,#15941,#15942,
#15943,#15944,#15945,#15946,#15947,#15948,#15949,#15950,#15951,#15952,#15953,
#15954,#15955,#15956,#15957),.UNSPECIFIED.,.F.,.F.,(4,2,2,2,2,2,2,2,2,4),
(9.99999992566316E-7,0.073261775877382,0.148517640224947,0.222784465371623,
0.296220695153182,0.372581441669242,0.445206623942385,0.519494682665066,
0.595216703454685,0.600517325493893),.UNSPECIFIED.);
#784=B_SPLINE_CURVE_WITH_KNOTS('',3,(#15962,#15963,#15964,#15965,#15966,
#15967,#15968,#15969,#15970,#15971,#15972,#15973,#15974,#15975,#15976,#15977,
#15978,#15979,#15980,#15981,#15982,#15983,#15984,#15985,#15986,#15987,#15988,
#15989,#15990,#15991,#15992,#15993,#15994,#15995,#15996,#15997,#15998,#15999),
 .UNSPECIFIED.,.F.,.F.,(4,2,2,2,2,2,2,2,2,2,2,2,2,2,2,2,2,2,4),(20.5336633202875,
20.5379028397142,20.6136758540443,20.6880566488837,20.7606931637132,20.8371521629564,
20.9106790831678,20.9848948112315,21.0603960074604,21.133073065851,21.2088134892057,
21.2833596437299,21.3557824762703,21.4315489590993,21.5052648239699,21.578854096748,
21.654575937,21.7274478848722,21.735148043229),.UNSPECIFIED.);
#785=B_SPLINE_CURVE_WITH_KNOTS('',3,(#16000,#16001,#16002,#16003,#16004,
#16005,#16006,#16007,#16008,#16009,#16010,#16011,#16012,#16013,#16014,#16015,
#16016,#16017,#16018,#16019,#16020,#16021,#16022,#16023,#16024,#16025,#16026,
#16027,#16028,#16029,#16030,#16031,#16032,#16033,#16034,#16035),
 .UNSPECIFIED.,.F.,.F.,(4,2,2,2,2,2,2,2,2,2,2,2,2,2,2,2,2,4),(0.600517325493893,
0.667612278651497,0.742740731622242,0.817626982135437,0.890823747292109,
0.966914372473297,1.03979849673016,1.11384065879918,1.18955318544221,1.26185304627361,
1.33673011198806,1.41235250817445,1.48533685995812,1.56118752270884,1.63444336293204,
1.70827064836793,1.78399660279134,1.8010716495484),.UNSPECIFIED.);
#786=B_SPLINE_CURVE_WITH_KNOTS('',3,(#16040,#16041,#16042,#16043,#16044,
#16045,#16046,#16047,#16048,#16049,#16050,#16051,#16052,#16053,#16054,#16055,
#16056,#16057,#16058,#16059,#16060,#16061,#16062,#16063,#16064,#16065,#16066,
#16067,#16068,#16069,#16070,#16071,#16072,#16073,#16074,#16075),
 .UNSPECIFIED.,.F.,.F.,(4,2,2,2,2,2,2,2,2,2,2,2,2,2,2,2,2,4),(19.3323573209819,
19.3484147961251,19.4241832189873,19.4980919040389,19.5713184805846,19.647256341792,
19.7203214434773,19.7958507281764,19.8708169249353,19.9431693074854,20.0189283058273,
20.0930582366082,20.1659315565263,20.2421156550342,20.3153987855463,20.3902097385234,
20.4654324286821,20.5336633202875),.UNSPECIFIED.);
#787=B_SPLINE_CURVE_WITH_KNOTS('',3,(#16076,#16077,#16078,#16079,#16080,
#16081,#16082,#16083,#16084,#16085,#16086,#16087,#16088,#16089,#16090,#16091,
#16092,#16093,#16094,#16095,#16096,#16097,#16098,#16099,#16100,#16101,#16102,
#16103,#16104,#16105,#16106,#16107,#16108,#16109,#16110,#16111),
 .UNSPECIFIED.,.F.,.F.,(4,2,2,2,2,2,2,2,2,2,2,2,2,2,2,2,2,4),(1.8010716495484,
1.85632097173359,1.93097958702412,2.00669544898473,2.07947671745479,2.15509765889709,
2.22887534865907,2.30250174281485,2.37826575306116,2.45073970736901,2.52519594000083,
2.60090396558053,2.6734198270398,2.7487208613376,2.82307768483266,2.89642023960164,
2.97267867831249,3.00178463538),.UNSPECIFIED.);
#788=B_SPLINE_CURVE_WITH_KNOTS('',3,(#16116,#16117,#16118,#16119,#16120,
#16121,#16122,#16123,#16124,#16125,#16126,#16127,#16128,#16129,#16130,#16131,
#16132,#16133,#16134,#16135,#16136,#16137,#16138,#16139,#16140,#16141,#16142,
#16143,#16144,#16145,#16146,#16147,#16148,#16149,#16150,#16151),
 .UNSPECIFIED.,.F.,.F.,(4,2,2,2,2,2,2,2,2,2,2,2,2,2,2,2,2,4),(18.1305008749428,
18.1578726481782,18.2343411588787,18.3078795059063,18.3821918466053,18.4577019685292,
18.5303892204231,18.6061604943215,18.6807161398418,18.7531832580321,18.8289827839731,
18.9027079219705,18.9763779108492,19.0521069660884,19.1249875630571,19.201317714322,
19.2760587308964,19.3323573209819),.UNSPECIFIED.);
#789=B_SPLINE_CURVE_WITH_KNOTS('',3,(#16152,#16153,#16154,#16155,#16156,
#16157,#16158,#16159,#16160,#16161,#16162,#16163,#16164,#16165,#16166,#16167,
#16168,#16169,#16170,#16171,#16172,#16173,#16174,#16175,#16176,#16177,#16178,
#16179,#16180,#16181,#16182,#16183,#16184,#16185,#16186,#16187),
 .UNSPECIFIED.,.F.,.F.,(4,2,2,2,2,2,2,2,2,2,2,2,2,2,2,2,2,4),(3.00178463538,
3.04531437320501,3.11950655772365,3.19518552285788,3.26751148643464,3.34254217247711,
3.41754738871303,3.49065592253175,3.56665029446013,3.63957183128242,3.71352440520342,
3.78919914579688,3.86145728333581,3.9362433503504,4.01200521216688,4.08490867151133,
4.16067128180272,4.20177247101643),.UNSPECIFIED.);
#790=B_SPLINE_CURVE_WITH_KNOTS('',3,(#16192,#16193,#16194,#16195,#16196,
#16197,#16198,#16199,#16200,#16201,#16202,#16203,#16204,#16205,#16206,#16207,
#16208,#16209,#16210,#16211,#16212,#16213,#16214,#16215,#16216,#16217,#16218,
#16219,#16220,#16221,#16222,#16223,#16224,#16225,#16226,#16227),
 .UNSPECIFIED.,.F.,.F.,(4,2,2,2,2,2,2,2,2,2,2,2,2,2,2,2,2,4),(16.9284782926901,
16.9678976750472,17.0438510669624,17.1169330115821,17.1925854820866,17.2675652039096,
17.3399503832518,17.4157492456997,17.4898927769109,17.5628373804741,17.6390334998648,
17.7123303300565,17.7872529716401,17.8624863899118,17.9349763255315,18.0107865695245,
18.0851783175673,18.1305008749428),.UNSPECIFIED.);
#791=B_SPLINE_CURVE_WITH_KNOTS('',3,(#16228,#16229,#16230,#16231,#16232,
#16233,#16234,#16235,#16236,#16237,#16238,#16239,#16240,#16241,#16242,#16243,
#16244,#16245,#16246,#16247,#16248,#16249,#16250,#16251,#16252,#16253,#16254,
#16255,#16256,#16257,#16258,#16259,#16260,#16261,#16262,#16263),
 .UNSPECIFIED.,.F.,.F.,(4,2,2,2,2,2,2,2,2,2,2,2,2,2,2,2,2,4),(4.20177247101643,
4.23398639776024,4.30773238538011,4.38342550182221,4.45573344091213,4.53030981628678,
4.60598738978255,4.67869011646994,4.75422560786203,4.82809657464004,4.90164519382672,
4.97813761619202,5.05060070132551,5.12500656732537,5.20068772705914,5.27315693915424,
5.34840666656873,5.40206337156151),.UNSPECIFIED.);
#792=B_SPLINE_CURVE_WITH_KNOTS('',3,(#16268,#16269,#16270,#16271,#16272,
#16273,#16274,#16275,#16276,#16277,#16278,#16279,#16280,#16281,#16282,#16283,
#16284,#16285,#16286,#16287,#16288,#16289,#16290,#16291,#16292,#16293,#16294,
#16295,#16296,#16297,#16298,#16299,#16300,#16301,#16302,#16303),
 .UNSPECIFIED.,.F.,.F.,(4,2,2,2,2,2,2,2,2,2,2,2,2,2,2,2,2,4),(15.726117824467,
15.7780750192724,15.853606763511,15.9263163363047,16.0021301582733,16.0767077486258,
16.1492304547217,16.2250745456645,16.2988212561443,16.3725818347547,16.448330814818,
16.5212321990517,16.5976919639176,16.6724503083522,16.7448517316063,16.8206624353022,
16.8945883123486,16.9284782926901),.UNSPECIFIED.);
#793=B_SPLINE_CURVE_WITH_KNOTS('',3,(#16304,#16305,#16306,#16307,#16308,
#16309,#16310,#16311,#16312,#16313,#16314,#16315,#16316,#16317,#16318,#16319,
#16320,#16321,#16322,#16323,#16324,#16325,#16326,#16327,#16328,#16329,#16330,
#16331,#16332,#16333,#16334,#16335,#16336,#16337,#16338,#16339),
 .UNSPECIFIED.,.F.,.F.,(4,2,2,2,2,2,2,2,2,2,2,2,2,2,2,2,2,4),(5.40206337156151,
5.42280202682982,5.49609741893041,5.57230460411098,5.64494245529769,5.71908647523217,
5.79474126674104,5.86703289445559,5.94201457649685,6.01707103049025,6.09013508828157,
6.16608119732253,6.23901689966539,6.31292439432828,6.38857738200078,6.46081383727264,
6.5355541601915,6.60170135024484),.UNSPECIFIED.);
#794=B_SPLINE_CURVE_WITH_KNOTS('',3,(#16344,#16345,#16346,#16347,#16348,
#16349,#16350,#16351,#16352,#16353,#16354,#16355,#16356,#16357,#16358,#16359,
#16360,#16361,#16362,#16363,#16364,#16365,#16366,#16367,#16368,#16369,#16370,
#16371,#16372,#16373,#16374,#16375,#16376,#16377,#16378,#16379),
 .UNSPECIFIED.,.F.,.F.,(4,2,2,2,2,2,2,2,2,2,2,2,2,2,2,2,2,4),(14.5232480602204,
14.587720826004,14.6627266216289,14.7351566206077,14.8110065122084,14.8851760254236,
14.9582018706076,15.0344228221103,15.1077455393524,15.1827880426445,15.2580448317048,
15.330567041737,15.4064258517686,15.4808410268554,15.5536039491834,15.6300948676244,
15.7036569101188,15.726117824467),.UNSPECIFIED.);
#795=B_SPLINE_CURVE_WITH_KNOTS('',3,(#16380,#16381,#16382,#16383,#16384,
#16385,#16386,#16387,#16388,#16389,#16390,#16391,#16392,#16393,#16394,#16395,
#16396,#16397,#16398,#16399,#16400,#16401,#16402,#16403,#16404,#16405,#16406,
#16407,#16408,#16409,#16410,#16411,#16412,#16413,#16414,#16415,#16416,#16417),
 .UNSPECIFIED.,.F.,.F.,(4,2,2,2,2,2,2,2,2,2,2,2,2,2,2,2,2,2,4),(6.60170135024484,
6.61137577552695,6.68423824543049,6.75995648832746,6.83329516983099,6.90699999888082,
6.98267359184862,7.05497103331607,7.12950580421754,7.20516147352223,7.27782441678246,
7.35331687836184,7.42722660556652,7.50073581542755,7.57718483813595,7.64964990352041,
7.72401516242666,7.79968082938935,7.80168454737663),.UNSPECIFIED.);
#796=B_SPLINE_CURVE_WITH_KNOTS('',3,(#16422,#16423,#16424,#16425,#16426,
#16427,#16428,#16429,#16430,#16431,#16432,#16433,#16434,#16435,#16436,#16437,
#16438,#16439,#16440,#16441,#16442,#16443,#16444,#16445,#16446,#16447,#16448,
#16449,#16450,#16451,#16452,#16453,#16454,#16455,#16456,#16457,#16458,#16459),
 .UNSPECIFIED.,.F.,.F.,(4,2,2,2,2,2,2,2,2,2,2,2,2,2,2,2,2,2,4),(13.3202804103381,
13.3204858332824,13.396327946239,13.4709396564183,13.5435282910564,13.6194278366413,
13.6932081483868,13.7670676615046,13.842849038861,13.9157830966167,13.992378939387,
14.0671670071756,14.139624957434,14.2154889603696,14.2894442653871,14.3628455045441,
14.4388271007212,14.5119379522483,14.5232480602204),.UNSPECIFIED.);
#797=B_SPLINE_CURVE_WITH_KNOTS('',3,(#16460,#16461,#16462,#16463,#16464,
#16465,#16466,#16467,#16468,#16469,#16470,#16471,#16472,#16473,#16474,#16475,
#16476,#16477,#16478,#16479,#16480,#16481,#16482,#16483,#16484,#16485,#16486,
#16487,#16488,#16489,#16490,#16491,#16492,#16493,#16494,#16495),
 .UNSPECIFIED.,.F.,.F.,(4,2,2,2,2,2,2,2,2,2,2,2,2,2,2,2,2,4),(7.80168454737663,
7.87211413102601,7.94732240677868,8.02177231494539,8.09503035135967,8.17119637492625,
8.24384995772828,8.31795574584409,8.39359784723522,8.46586665716587,8.54080937647058,
8.61593349998142,8.68896308906026,8.76487125310207,8.83783517633463,8.91170775389988,
8.98735057902809,9.00117105879399),.UNSPECIFIED.);
#798=B_SPLINE_CURVE_WITH_KNOTS('',3,(#16500,#16501,#16502,#16503,#16504,
#16505,#16506,#16507,#16508,#16509,#16510,#16511,#16512,#16513,#16514,#16515,
#16516,#16517,#16518,#16519,#16520,#16521,#16522,#16523,#16524,#16525,#16526,
#16527,#16528,#16529,#16530,#16531,#16532,#16533,#16534,#16535),
 .UNSPECIFIED.,.F.,.F.,(4,2,2,2,2,2,2,2,2,2,2,2,2,2,2,2,2,4),(12.1180952064906,
12.1300964327481,12.2059000950361,12.2800023729485,12.3530142433209,12.429164356048,
12.5024207579045,12.577482546649,12.6526682733113,12.7251319418283,12.8009422564708,
12.8752874494255,12.9480251561944,13.0244425760833,13.0979359086261,13.1723612965324,
13.2478199418432,13.3202804103381),.UNSPECIFIED.);
#799=B_SPLINE_CURVE_WITH_KNOTS('',3,(#16536,#16537,#16538,#16539,#16540,
#16541,#16542,#16543,#16544,#16545,#16546,#16547,#16548,#16549,#16550,#16551,
#16552,#16553,#16554,#16555,#16556,#16557,#16558,#16559,#16560,#16561,#16562,
#16563,#16564,#16565,#16566,#16567,#16568,#16569,#16570,#16571),
 .UNSPECIFIED.,.F.,.F.,(4,2,2,2,2,2,2,2,2,2,2,2,2,2,2,2,2,4),(9.00117105879399,
9.05957747650006,9.13428234170321,9.21018018815867,9.28301191789558,9.35869638013789,
9.43207287871308,9.50574697566939,9.58141274520128,9.65371218182695,9.72821591324838,
9.80386132341097,9.87649484644817,9.95195499133692,10.0259184544355,10.0993988305648,
10.1758153751141,10.2009145729997),.UNSPECIFIED.);
#800=B_SPLINE_CURVE_WITH_KNOTS('',3,(#16576,#16577,#16578,#16579,#16580,
#16581,#16582,#16583,#16584,#16585,#16586,#16587,#16588,#16589,#16590,#16591,
#16592,#16593,#16594,#16595,#16596,#16597,#16598,#16599,#16600,#16601,#16602,
#16603,#16604,#16605,#16606,#16607,#16608,#16609,#16610,#16611),
 .UNSPECIFIED.,.F.,.F.,(4,2,2,2,2,2,2,2,2,2,2,2,2,2,2,2,2,4),(10.9159048894311,
10.9417285685803,11.0153840118466,11.0919857331349,11.1645843892562,11.2390977710806,
11.3119432957782,11.3877499955148,11.4624736172065,11.5348953545546,11.6107151951244,
11.6846067885645,11.7580031449498,11.8339173959719,11.9069650575345,11.9827756411443,
12.0577132709042,12.1180952064906),.UNSPECIFIED.);
#801=B_SPLINE_CURVE_WITH_KNOTS('',3,(#16612,#16613,#16614,#16615,#16616,
#16617,#16618,#16619,#16620,#16621,#16622,#16623,#16624,#16625,#16626,#16627,
#16628,#16629,#16630,#16631,#16632,#16633,#16634,#16635,#16636,#16637,#16638,
#16639,#16640,#16641,#16642,#16643,#16644,#16645,#16646,#16647),
 .UNSPECIFIED.,.F.,.F.,(4,2,2,2,2,2,2,2,2,2,2,2,2,2,2,2,2,4),(10.2009145729997,
10.2482956163185,10.322630969213,10.3982930177132,10.4707021613456,10.5458798011778,
10.6203996650247,10.6936310413183,10.7697669637686,10.8424499299129,10.9165283318329,
10.9921696743595,11.0644279598046,11.1393426885537,11.2145500048589,11.2901931117698,
11.3640626377355,11.4005300405451),.UNSPECIFIED.);
#802=B_SPLINE_CURVE_WITH_KNOTS('',3,(#16652,#16653,#16654,#16655,#16656,
#16657,#16658,#16659,#16660,#16661,#16662,#16663,#16664,#16665,#16666,#16667,
#16668,#16669,#16670,#16671,#16672,#16673,#16674,#16675,#16676,#16677,#16678,
#16679,#16680,#16681,#16682,#16683,#16684,#16685,#16686,#16687),
 .UNSPECIFIED.,.F.,.F.,(4,2,2,2,2,2,2,2,2,2,2,2,2,2,2,2,2,4),(9.71384447846264,
9.75123807372611,9.82529401484089,9.90109268520411,9.97346838049563,10.0483588614417,
10.1243054415182,10.1973133659223,10.2731832176365,10.3466515722912,10.4205034552055,
10.4963221962313,10.5687561318069,10.6434396061474,10.7192409968005,10.7920487072417,
10.8676920069456,10.9159048894311),.UNSPECIFIED.);
#803=B_SPLINE_CURVE_WITH_KNOTS('',3,(#16688,#16689,#16690,#16691,#16692,
#16693,#16694,#16695,#16696,#16697,#16698,#16699,#16700,#16701,#16702,#16703,
#16704,#16705,#16706,#16707,#16708,#16709,#16710,#16711,#16712,#16713,#16714,
#16715,#16716,#16717,#16718,#16719,#16720,#16721,#16722,#16723),
 .UNSPECIFIED.,.F.,.F.,(4,2,2,2,2,2,2,2,2,2,2,2,2,2,2,2,2,4),(11.4005300405451,
11.4370319883629,11.512936739381,11.5859633149398,11.66109817641,11.7360373201757,
11.8083047404636,11.8839467877415,11.9580490787634,12.0307064288464,12.1068686070501,
12.1801232420663,12.2545821520692,12.3297865173144,12.4022166746571,12.4778819161449,
12.5522433586879,12.6001780638435),.UNSPECIFIED.);
#804=B_SPLINE_CURVE_WITH_KNOTS('',3,(#16728,#16729,#16730,#16731,#16732,
#16733,#16734,#16735,#16736,#16737,#16738,#16739,#16740,#16741,#16742,#16743,
#16744,#16745,#16746,#16747,#16748,#16749,#16750,#16751,#16752,#16753,#16754,
#16755,#16756,#16757,#16758,#16759,#16760,#16761,#16762,#16763),
 .UNSPECIFIED.,.F.,.F.,(4,2,2,2,2,2,2,2,2,2,2,2,2,2,2,2,2,4),(8.51163684764714,
8.56051488014775,8.63507149460952,8.71089970093124,8.78351502133584,8.85891730151577,
8.93344036889881,9.00688362281223,9.08324511353396,9.15601680140874,9.2303105092999,
9.30611160804312,9.37854583103873,9.45367896715513,9.52886111434057,9.60207190548669,
9.67817105698719,9.71384447846264),.UNSPECIFIED.);
#805=B_SPLINE_CURVE_WITH_KNOTS('',3,(#16764,#16765,#16766,#16767,#16768,
#16769,#16770,#16771,#16772,#16773,#16774,#16775,#16776,#16777,#16778,#16779,
#16780,#16781,#16782,#16783,#16784,#16785,#16786,#16787,#16788,#16789,#16790,
#16791,#16792,#16793,#16794,#16795,#16796,#16797,#16798,#16799),
 .UNSPECIFIED.,.F.,.F.,(4,2,2,2,2,2,2,2,2,2,2,2,2,2,2,2,2,4),(12.6001780638435,
12.6247103529074,12.7011552296179,12.7746607626844,12.8485773844421,12.9240657240679,
12.9967249178213,13.0723793041668,13.1469101199023,13.2192078014959,13.2948804280115,
13.3685813421806,13.4419248676146,13.5176388064005,13.5904973625241,13.6663287520978,
13.7410645591005,13.8000330191523),.UNSPECIFIED.);
#806=B_SPLINE_CURVE_WITH_KNOTS('',3,(#16804,#16805,#16806,#16807,#16808,
#16809,#16810,#16811,#16812,#16813,#16814,#16815,#16816,#16817,#16818,#16819,
#16820,#16821,#16822,#16823,#16824,#16825,#16826,#16827,#16828,#16829,#16830,
#16831,#16832,#16833,#16834,#16835,#16836,#16837,#16838,#16839),
 .UNSPECIFIED.,.F.,.F.,(4,2,2,2,2,2,2,2,2,2,2,2,2,2,2,2,2,4),(7.30910491909639,
7.36904466691905,7.44398341398191,7.51987439067294,7.59292582087003,7.66884263680248,
7.74229098745011,7.81618658837825,7.89202775292298,7.96447527526033,8.03920294715864,
8.11502912392363,8.18787916176048,8.26356811876647,8.33756968006074,8.41126712892377,
8.48791492770604,8.51163684764714),.UNSPECIFIED.);
#807=B_SPLINE_CURVE_WITH_KNOTS('',3,(#16840,#16841,#16842,#16843,#16844,
#16845,#16846,#16847,#16848,#16849,#16850,#16851,#16852,#16853,#16854,#16855,
#16856,#16857,#16858,#16859,#16860,#16861,#16862,#16863,#16864,#16865,#16866,
#16867,#16868,#16869,#16870,#16871,#16872,#16873,#16874,#16875),
 .UNSPECIFIED.,.F.,.F.,(4,2,2,2,2,2,2,2,2,2,2,2,2,2,2,2,2,4),(13.8000330191523,
13.8132997602596,13.8889514810619,13.9628545298081,14.0357938247276,14.1117351018702,
14.1847947733853,14.2598598732388,14.3348365968016,14.4071252676432,14.4827784672019,
14.5569176226292,14.6295574535427,14.7057594011558,14.7790500427128,14.8534523457235,
14.928696802142,14.9997046922138),.UNSPECIFIED.);
#808=B_SPLINE_CURVE_WITH_KNOTS('',3,(#16880,#16881,#16882,#16883,#16884,
#16885,#16886,#16887,#16888,#16889,#16890,#16891,#16892,#16893,#16894,#16895,
#16896,#16897,#16898,#16899,#16900,#16901,#16902,#16903,#16904,#16905,#16906,
#16907,#16908,#16909,#16910,#16911,#16912,#16913,#16914,#16915),
 .UNSPECIFIED.,.F.,.F.,(4,2,2,2,2,2,2,2,2,2,2,2,2,2,2,2,2,4),(6.10664536118632,
6.17866461342232,6.25412061574428,6.32860913795001,6.40210195980943,6.47851717655568,
6.55129006619227,6.62563437348072,6.70146248771766,6.77393386191794,6.84911846281497,
6.9242534903129,6.99751121258825,7.07366115565623,7.1467175018577,7.2208210143513,
7.29664430841493,7.30910491909639),.UNSPECIFIED.);
#809=B_SPLINE_CURVE_WITH_KNOTS('',3,(#16916,#16917,#16918,#16919,#16920,
#16921,#16922,#16923,#16924,#16925,#16926,#16927,#16928,#16929,#16930,#16931,
#16932,#16933,#16934,#16935,#16936,#16937,#16938,#16939,#16940,#16941,#16942,
#16943,#16944,#16945,#16946,#16947,#16948,#16949,#16950,#16951,#16952,#16953),
 .UNSPECIFIED.,.F.,.F.,(4,2,2,2,2,2,2,2,2,2,2,2,2,2,2,2,2,2,4),(14.9997046922138,
15.0011613882487,15.0768405953163,15.1512412983625,15.2237046008859,15.3001915049673,
15.3737351155337,15.4476109939679,15.5231410173751,15.5958386903706,15.6715134909765,
15.7460845825,15.8183911548274,15.8940818044762,15.9678225658965,16.0411406541614,
16.1168976313948,16.1897958881647,16.1999526159265),.UNSPECIFIED.);
#810=B_SPLINE_CURVE_WITH_KNOTS('',3,(#16958,#16959,#16960,#16961,#16962,
#16963,#16964,#16965,#16966,#16967,#16968,#16969,#16970,#16971,#16972,#16973,
#16974,#16975,#16976,#16977,#16978,#16979,#16980,#16981,#16982,#16983,#16984,
#16985,#16986,#16987,#16988,#16989,#16990,#16991,#16992,#16993,#16994,#16995),
 .UNSPECIFIED.,.F.,.F.,(4,2,2,2,2,2,2,2,2,2,2,2,2,2,2,2,2,2,4),(4.90346669291888,
4.91506870236462,4.98820357266399,5.0642110881259,5.13760351086168,5.21158300924342,
5.28745976927761,5.35992685538553,5.43473940551762,5.51060663707254,5.58353780541342,
5.65931490562363,5.73322660979942,5.80700448229846,5.88291878918759,5.95553277454454,
6.03014214800553,6.10600003177494,6.10664536118632),.UNSPECIFIED.);
#811=B_SPLINE_CURVE_WITH_KNOTS('',3,(#16996,#16997,#16998,#16999,#17000,
#17001,#17002,#17003,#17004,#17005,#17006,#17007,#17008,#17009,#17010,#17011,
#17012,#17013,#17014,#17015,#17016,#17017,#17018,#17019,#17020,#17021,#17022,
#17023,#17024,#17025,#17026,#17027,#17028,#17029,#17030,#17031),
 .UNSPECIFIED.,.F.,.F.,(4,2,2,2,2,2,2,2,2,2,2,2,2,2,2,2,2,4),(16.1999526159265,
16.2655653257236,16.3403455878608,16.4126009260191,16.4882729159108,16.5622197702428,
16.6351430664402,16.7111313156308,16.7842342086322,16.8592458915388,16.9342703643616,
17.006591918744,17.0822678244985,17.1564539028843,17.2290898213618,17.305341763104,
17.3786783406879,17.3999243091323),.UNSPECIFIED.);
#812=B_SPLINE_CURVE_WITH_KNOTS('',3,(#17036,#17037,#17038,#17039,#17040,
#17041,#17042,#17043,#17044,#17045,#17046,#17047,#17048,#17049,#17050,#17051,
#17052,#17053,#17054,#17055,#17056,#17057,#17058,#17059,#17060,#17061,#17062,
#17063,#17064,#17065,#17066,#17067,#17068,#17069,#17070,#17071),
 .UNSPECIFIED.,.F.,.F.,(4,2,2,2,2,2,2,2,2,2,2,2,2,2,2,2,2,4),(3.70035601869793,
3.72311624650954,3.79670529484639,3.87322545967511,3.94599134340126,4.02043411786514,
4.09630815185354,4.16885219107272,4.24413705849594,4.31915694699897,4.39250538571124,
4.46875415936413,4.54177650959524,4.61597214318868,4.6918359692238,4.76428118831078,
4.83931350214248,4.90346669291888),.UNSPECIFIED.);
#813=B_SPLINE_CURVE_WITH_KNOTS('',3,(#17072,#17073,#17074,#17075,#17076,
#17077,#17078,#17079,#17080,#17081,#17082,#17083,#17084,#17085,#17086,#17087,
#17088,#17089,#17090,#17091,#17092,#17093,#17094,#17095,#17096,#17097,#17098,
#17099,#17100,#17101,#17102,#17103,#17104,#17105,#17106,#17107),
 .UNSPECIFIED.,.F.,.F.,(4,2,2,2,2,2,2,2,2,2,2,2,2,2,2,2,2,4),(17.3999243091323,
17.4530399991148,17.5283345331806,17.6008444296539,17.6765490523624,17.7509989042253,
17.823471428145,17.9000104222439,17.9736018979823,18.0474522767511,18.1230338545409,
18.1957795858358,18.2714859169376,18.3461070373767,18.4184345339858,18.4941544247165,
18.5679446597149,18.6006226277154),.UNSPECIFIED.);
#814=B_SPLINE_CURVE_WITH_KNOTS('',3,(#17112,#17113,#17114,#17115,#17116,
#17117,#17118,#17119,#17120,#17121,#17122,#17123,#17124,#17125,#17126,#17127,
#17128,#17129,#17130,#17131,#17132,#17133,#17134,#17135,#17136,#17137,#17138,
#17139,#17140,#17141,#17142,#17143,#17144,#17145,#17146,#17147),
 .UNSPECIFIED.,.F.,.F.,(4,2,2,2,2,2,2,2,2,2,2,2,2,2,2,2,2,4),(2.49771244823052,
2.53192367017835,2.60588018236931,2.6817093794774,2.75412572335012,2.82891507571771,
2.90534779569656,2.97827737294551,3.05405652257629,3.12780907401846,3.20158401386577,
3.27744541782065,3.34997777562528,3.42458384305547,3.500416008436,3.57315285646769,
3.64871375186048,3.70035601869793),.UNSPECIFIED.);
#815=B_SPLINE_CURVE_WITH_KNOTS('',3,(#17148,#17149,#17150,#17151,#17152,
#17153,#17154,#17155,#17156,#17157,#17158,#17159,#17160,#17161,#17162,#17163,
#17164,#17165,#17166,#17167,#17168,#17169,#17170,#17171,#17172,#17173,#17174,
#17175,#17176,#17177,#17178,#17179,#17180,#17181,#17182,#17183),
 .UNSPECIFIED.,.F.,.F.,(4,2,2,2,2,2,2,2,2,2,2,2,2,2,2,2,2,4),(18.6006226277154,
18.6412515943291,18.7170613483601,18.7900087657457,18.8657332626392,18.9405674102812,
19.0128543569302,19.088557693505,19.162557674121,19.2354788720627,19.3115235235351,
19.3846788212928,19.4596538548932,19.5347352341894,19.6071003449551,19.6828098930783,
19.7570519591634,19.8010822666473),.UNSPECIFIED.);
#816=B_SPLINE_CURVE_WITH_KNOTS('',3,(#17188,#17189,#17190,#17191,#17192,
#17193,#17194,#17195,#17196,#17197,#17198,#17199,#17200,#17201,#17202,#17203,
#17204,#17205,#17206,#17207,#17208,#17209,#17210,#17211,#17212,#17213,#17214,
#17215,#17216,#17217,#17218,#17219,#17220,#17221,#17222,#17223),
 .UNSPECIFIED.,.F.,.F.,(4,2,2,2,2,2,2,2,2,2,2,2,2,2,2,2,2,4),(1.29536360785537,
1.3410237414506,1.41544967668057,1.49128106098848,1.56379951471133,1.6390676891521,
1.71397174076513,1.78730072016975,1.86353142409529,1.93647760847481,2.01065379022671,
2.08647240671551,2.15887907340395,2.233891932145,2.30952022673612,2.38263254256176,
2.45861853204788,2.49771244823052),.UNSPECIFIED.);
#817=B_SPLINE_CURVE_WITH_KNOTS('',3,(#17224,#17225,#17226,#17227,#17228,
#17229,#17230,#17231,#17232,#17233,#17234,#17235,#17236,#17237,#17238,#17239,
#17240,#17241,#17242,#17243,#17244,#17245,#17246,#17247,#17248,#17249,#17250,
#17251,#17252,#17253,#17254,#17255,#17256,#17257,#17258,#17259),
 .UNSPECIFIED.,.F.,.F.,(4,2,2,2,2,2,2,2,2,2,2,2,2,2,2,2,2,4),(19.8010822666473,
19.8296971813633,19.906008297278,19.9793997719053,20.0537368961349,20.1290904646827,
20.2016554087686,20.2773962331364,20.3519041110699,20.4243981590469,20.500196098935,
20.5738737064591,20.6476431596998,20.7233186338297,20.7961510557135,20.8726600109033,
20.9473431199328,21.0023403829801),.UNSPECIFIED.);
#818=B_SPLINE_CURVE_WITH_KNOTS('',3,(#17264,#17265,#17266,#17267,#17268,
#17269,#17270,#17271,#17272,#17273,#17274,#17275,#17276,#17277,#17278,#17279,
#17280,#17281,#17282,#17283,#17284,#17285,#17286,#17287,#17288,#17289,#17290,
#17291,#17292,#17293,#17294,#17295,#17296,#17297,#17298,#17299),
 .UNSPECIFIED.,.F.,.F.,(4,2,2,2,2,2,2,2,2,2,2,2,2,2,2,2,2,4),(0.0931362008875077,
0.149790300478668,0.22456899063002,0.300876335984474,0.373791545212683,
0.449557496276257,0.523224461713842,0.596984331376484,0.67280719625716,
0.745289827435934,0.819880533368118,0.895676274953773,0.968397209774783,
1.04394319560093,1.11824450231286,1.19181633349106,1.26832090648479,1.29536360785537),
 .UNSPECIFIED.);
#819=B_SPLINE_CURVE_WITH_KNOTS('',3,(#17300,#17301,#17302,#17303,#17304,
#17305,#17306,#17307,#17308,#17309,#17310,#17311,#17312,#17313,#17314,#17315,
#17316,#17317,#17318,#17319,#17320,#17321,#17322,#17323,#17324,#17325,#17326,
#17327,#17328,#17329,#17330,#17331,#17332,#17333,#17334,#17335),
 .UNSPECIFIED.,.F.,.F.,(4,2,2,2,2,2,2,2,2,2,2,2,2,2,2,2,2,4),(21.0023403829801,
21.0197048750824,21.0954669052174,21.1693184250428,21.2426289506514,21.3185035201107,
21.3915117307964,21.4672078751245,21.5421076664978,21.6144392466584,21.6901867449512,
21.7642514729239,21.8371851198342,21.9132980208032,21.9865171840574,22.0614720493734,
22.1366219228939,22.2034453162522),.UNSPECIFIED.);
#820=B_SPLINE_CURVE_WITH_KNOTS('',3,(#17341,#17342,#17343,#17344,#17345,
#17346,#17347,#17348,#17349,#17350,#17351,#17352,#17353,#17354,#17355,#17356),
 .UNSPECIFIED.,.F.,.F.,(4,2,2,2,2,2,2,4),(22.05254318977,22.1180882873261,
22.1913966771312,22.2674423144429,22.3406104852454,22.4162117292643,22.4590238164125,
22.5016957284502),.UNSPECIFIED.);
#821=B_SPLINE_CURVE_WITH_KNOTS('',3,(#17359,#17360,#17361,#17362,#17363,
#17364,#17365,#17366,#17367,#17368,#17369,#17370),.UNSPECIFIED.,.F.,.F.,
(4,2,2,2,2,4),(9.9999999344546E-7,0.0733434466267004,0.148679158126967,
0.222930175188716,0.296371686733512,0.300253786431838),.UNSPECIFIED.);
#822=B_SPLINE_CURVE_WITH_KNOTS('',3,(#17375,#17376,#17377,#17378,#17379,
#17380,#17381,#17382,#17383,#17384,#17385,#17386,#17387,#17388,#17389,#17390,
#17391,#17392,#17393,#17394,#17395,#17396,#17397,#17398,#17399,#17400,#17401,
#17402,#17403,#17404,#17405,#17406,#17407,#17408,#17409,#17410,#17411,#17412),
 .UNSPECIFIED.,.F.,.F.,(4,2,2,2,2,2,2,2,2,2,2,2,2,2,2,2,2,2,4),(20.8492626875425,
20.8526997788034,20.92633985541,21.000728096518,21.0763435643888,21.1491317214545,
21.2250018067689,21.2996612587163,21.3722181264907,21.4481158219413,21.5219436477844,
21.5956936182336,21.6715288843462,21.7445111612003,21.82091239387,21.8957589923512,
21.968208067014,22.0440753652377,22.05254318977),.UNSPECIFIED.);
#823=B_SPLINE_CURVE_WITH_KNOTS('',3,(#17413,#17414,#17415,#17416,#17417,
#17418,#17419,#17420,#17421,#17422,#17423,#17424,#17425,#17426,#17427,#17428,
#17429,#17430,#17431,#17432,#17433,#17434,#17435,#17436,#17437,#17438,#17439,
#17440,#17441,#17442,#17443,#17444,#17445,#17446,#17447,#17448),
 .UNSPECIFIED.,.F.,.F.,(4,2,2,2,2,2,2,2,2,2,2,2,2,2,2,2,2,4),(0.300253786431838,
0.372738742718709,0.445357707142144,0.519651496018735,0.595372982506417,
0.667771570411935,0.742905776016391,0.817772805632994,0.890974369726359,
0.967070519807669,1.03994508219452,1.11399215053163,1.18970337979295,1.26200299001726,
1.33688506897023,1.4124856469306,1.48547398290461,1.50088857683023),
 .UNSPECIFIED.);
#824=B_SPLINE_CURVE_WITH_KNOTS('',3,(#17453,#17454,#17455,#17456,#17457,
#17458,#17459,#17460,#17461,#17462,#17463,#17464,#17465,#17466,#17467,#17468,
#17469,#17470,#17471,#17472,#17473,#17474,#17475,#17476,#17477,#17478,#17479,
#17480,#17481,#17482,#17483,#17484,#17485,#17486,#17487,#17488),
 .UNSPECIFIED.,.F.,.F.,(4,2,2,2,2,2,2,2,2,2,2,2,2,2,2,2,2,4),(19.645692524193,
19.6606922925129,19.7338735908416,19.8095956125189,19.8846784522713,19.9571568609594,
20.0330517465526,20.1072971763248,20.180323721384,20.2566251773908,20.3300226670146,
20.405017375142,20.4803551658045,20.5529426548938,20.6288497632478,20.703344608527,
20.7761247410544,20.8492626875425),.UNSPECIFIED.);
#825=B_SPLINE_CURVE_WITH_KNOTS('',3,(#17489,#17490,#17491,#17492,#17493,
#17494,#17495,#17496,#17497,#17498,#17499,#17500,#17501,#17502,#17503,#17504,
#17505,#17506,#17507,#17508,#17509,#17510,#17511,#17512,#17513,#17514,#17515,
#17516,#17517,#17518,#17519,#17520,#17521,#17522,#17523,#17524),
 .UNSPECIFIED.,.F.,.F.,(4,2,2,2,2,2,2,2,2,2,2,2,2,2,2,2,2,4),(1.50088857683023,
1.56132926031601,1.63457285707235,1.70840412356841,1.78412819690882,1.85644929963145,
1.93111194973725,2.00752125551993,2.08033097553257,2.15598401092867,2.22968137937417,
2.30333560484894,2.37909398462287,2.45154044534442,2.526024569367,2.60175189775299,
2.67437074343493,2.70178082223175),.UNSPECIFIED.);
#826=B_SPLINE_CURVE_WITH_KNOTS('',3,(#17529,#17530,#17531,#17532,#17533,
#17534,#17535,#17536,#17537,#17538,#17539,#17540,#17541,#17542,#17543,#17544,
#17545,#17546,#17547,#17548,#17549,#17550,#17551,#17552,#17553,#17554,#17555,
#17556,#17557,#17558,#17559,#17560,#17561,#17562,#17563,#17564),
 .UNSPECIFIED.,.F.,.F.,(4,2,2,2,2,2,2,2,2,2,2,2,2,2,2,2,2,4),(18.4419253882545,
18.4689607777214,18.5417674330568,18.6176764482914,18.692353915849,18.7649629384551,
18.8409016431339,18.9147471603291,18.9885848629576,19.064436034922,19.1374352663987,
19.21396378216,19.2888237212987,19.361314468639,19.437220454931,19.511246779585,
19.5846350260553,19.645692524193),.UNSPECIFIED.);
#827=B_SPLINE_CURVE_WITH_KNOTS('',3,(#17565,#17566,#17567,#17568,#17569,
#17570,#17571,#17572,#17573,#17574,#17575,#17576,#17577,#17578,#17579,#17580,
#17581,#17582,#17583,#17584,#17585,#17586,#17587,#17588,#17589,#17590,#17591,
#17592,#17593,#17594,#17595,#17596,#17597,#17598,#17599,#17600),
 .UNSPECIFIED.,.F.,.F.,(4,2,2,2,2,2,2,2,2,2,2,2,2,2,2,2,2,4),(2.70178082223175,
2.7498075868511,2.82416793687965,2.89763867153337,2.97403371648344,3.0467255487614,
3.12104813871485,3.19682290300267,3.26925914401864,3.34442216914417,3.41941186677616,
3.49264454688915,3.56877103926687,3.64173068239134,3.71580904480027,3.79157592600334,
3.86392532985084,3.90337860449495),.UNSPECIFIED.);
#828=B_SPLINE_CURVE_WITH_KNOTS('',3,(#17605,#17606,#17607,#17608,#17609,
#17610,#17611,#17612,#17613,#17614,#17615,#17616,#17617,#17618,#17619,#17620,
#17621,#17622,#17623,#17624,#17625,#17626,#17627,#17628,#17629,#17630,#17631,
#17632,#17633,#17634,#17635,#17636,#17637,#17638,#17639,#17640),
 .UNSPECIFIED.,.F.,.F.,(4,2,2,2,2,2,2,2,2,2,2,2,2,2,2,2,2,4),(17.2375105283243,
17.2766093876775,17.3491289223455,17.4250714160394,17.499338938451,17.5724438079126,
17.6487660648582,17.7221856134517,17.7972979623461,17.8726551407408,17.9452709356035,
18.0212231268876,18.0957374704035,18.1685829757813,18.2451763533381,18.3188362628287,
18.393327694986,18.4419253882545),.UNSPECIFIED.);
#829=B_SPLINE_CURVE_WITH_KNOTS('',3,(#17641,#17642,#17643,#17644,#17645,
#17646,#17647,#17648,#17649,#17650,#17651,#17652,#17653,#17654,#17655,#17656,
#17657,#17658,#17659,#17660,#17661,#17662,#17663,#17664,#17665,#17666,#17667,
#17668,#17669,#17670,#17671,#17672,#17673,#17674,#17675,#17676),
 .UNSPECIFIED.,.F.,.F.,(4,2,2,2,2,2,2,2,2,2,2,2,2,2,2,2,2,4),(3.90337860449495,
3.93883886724166,4.01457219092803,4.08759458450174,4.16348348884845,4.23682236672617,
4.31068828214277,4.38647020014597,4.45885236050979,4.53355002247132,4.61009741287901,
4.68294485075255,4.75863558635613,4.83243494391621,4.90612786986772,4.98194618038897,
5.05446269206163,5.10503562671789),.UNSPECIFIED.);
#830=B_SPLINE_CURVE_WITH_KNOTS('',3,(#17681,#17682,#17683,#17684,#17685,
#17686,#17687,#17688,#17689,#17690,#17691,#17692,#17693,#17694,#17695,#17696,
#17697,#17698,#17699,#17700,#17701,#17702,#17703,#17704,#17705,#17706,#17707,
#17708,#17709,#17710,#17711,#17712,#17713,#17714,#17715,#17716),
 .UNSPECIFIED.,.F.,.F.,(4,2,2,2,2,2,2,2,2,2,2,2,2,2,2,2,2,4),(16.0330840204075,
16.0841125680968,16.1568062445162,16.2328002845215,16.3066506773229,16.3806513190249,
16.4565023761763,16.529505085786,16.6054509302403,16.6803367129194,16.752880602522,
16.8288365206925,16.9028884433636,16.9763659562233,17.0524474525173,17.1256538804743,
17.2015044165735,17.2375105283243),.UNSPECIFIED.);
#831=B_SPLINE_CURVE_WITH_KNOTS('',3,(#17717,#17718,#17719,#17720,#17721,
#17722,#17723,#17724,#17725,#17726,#17727,#17728,#17729,#17730,#17731,#17732,
#17733,#17734,#17735,#17736,#17737,#17738,#17739,#17740,#17741,#17742,#17743,
#17744,#17745,#17746,#17747,#17748,#17749,#17750,#17751,#17752),
 .UNSPECIFIED.,.F.,.F.,(4,2,2,2,2,2,2,2,2,2,2,2,2,2,2,2,2,4),(5.10503562671789,
5.128986095298,5.20474754783383,5.27732785095318,5.35269704620258,5.4270671253138,
5.50047437008582,5.57680143647526,5.64947178183473,5.72372970158786,5.79946041374855,
5.87184324601293,5.94694059652358,6.02195142938892,6.09512293367728,6.17118401925371,
6.24413288664852,6.30606327815735),.UNSPECIFIED.);
#832=B_SPLINE_CURVE_WITH_KNOTS('',3,(#17757,#17758,#17759,#17760,#17761,
#17762,#17763,#17764,#17765,#17766,#17767,#17768,#17769,#17770,#17771,#17772,
#17773,#17774,#17775,#17776,#17777,#17778,#17779,#17780,#17781,#17782,#17783,
#17784,#17785,#17786,#17787,#17788,#17789,#17790,#17791,#17792),
 .UNSPECIFIED.,.F.,.F.,(4,2,2,2,2,2,2,2,2,2,2,2,2,2,2,2,2,4),(14.8292463189387,
14.8916714870627,14.9648135885411,15.0410390970424,15.1143699500454,15.1896012848457,
15.2648602033373,15.3374059196021,15.4133145735808,15.4877324338808,15.5605880748831,
15.6370785099079,15.7106441465414,15.7852253876934,15.8607555191899,15.9334919583014,
16.009429815992,16.0330840204075),.UNSPECIFIED.);
#833=B_SPLINE_CURVE_WITH_KNOTS('',3,(#17793,#17794,#17795,#17796,#17797,
#17798,#17799,#17800,#17801,#17802,#17803,#17804,#17805,#17806,#17807,#17808,
#17809,#17810,#17811,#17812,#17813,#17814,#17815,#17816,#17817,#17818,#17819,
#17820,#17821,#17822,#17823,#17824,#17825,#17826,#17827,#17828),
 .UNSPECIFIED.,.F.,.F.,(4,2,2,2,2,2,2,2,2,2,2,2,2,2,2,2,2,4),(6.30606327815735,
6.3181492331229,6.39387422239827,6.4661814102393,6.54103207285242,6.61679445258831,
6.68975868398347,6.76558555007303,6.83892225320291,6.91272954788185,6.98847154733521,
7.06082159277665,7.13545996398158,7.2111879061331,7.28395060515172,7.35954946368319,
7.43343288378257,7.50694329613649),.UNSPECIFIED.);
#834=B_SPLINE_CURVE_WITH_KNOTS('',3,(#17833,#17834,#17835,#17836,#17837,
#17838,#17839,#17840,#17841,#17842,#17843,#17844,#17845,#17846,#17847,#17848,
#17849,#17850,#17851,#17852,#17853,#17854,#17855,#17856,#17857,#17858,#17859,
#17860,#17861,#17862,#17863,#17864,#17865,#17866,#17867,#17868,#17869,#17870),
 .UNSPECIFIED.,.F.,.F.,(4,2,2,2,2,2,2,2,2,2,2,2,2,2,2,2,2,2,4),(13.6255081123504,
13.6257686237007,13.69954079358,13.7736346929468,13.8493998261943,13.9223235489263,
13.9982307610449,14.0730338438641,14.1455609916275,14.2214837444646,14.2954539153653,
14.3689905924738,14.444983558864,14.5181086459962,14.5940987389015,14.6691122320421,
14.7415896580288,14.8174940250215,14.8292463189387),.UNSPECIFIED.);
#835=B_SPLINE_CURVE_WITH_KNOTS('',3,(#17871,#17872,#17873,#17874,#17875,
#17876,#17877,#17878,#17879,#17880,#17881,#17882,#17883,#17884,#17885,#17886,
#17887,#17888,#17889,#17890,#17891,#17892,#17893,#17894,#17895,#17896,#17897,
#17898,#17899,#17900,#17901,#17902,#17903,#17904,#17905,#17906,#17907,#17908),
 .UNSPECIFIED.,.F.,.F.,(4,2,2,2,2,2,2,2,2,2,2,2,2,2,2,2,2,2,4),(7.50694329613649,
7.50704168142511,7.58359819570377,7.65609581512641,7.73056303342993,7.80629057752357,
7.87881785040344,7.95412986788821,8.02852802101149,8.10188223252519,8.17815202887751,
8.25081592351181,8.32501973957617,8.40071914005803,8.47306065592921,8.54810300239926,
8.62315419471727,8.69627520937395,8.7076043136218),.UNSPECIFIED.);
#836=B_SPLINE_CURVE_WITH_KNOTS('',3,(#17913,#17914,#17915,#17916,#17917,
#17918,#17919,#17920,#17921,#17922,#17923,#17924,#17925,#17926,#17927,#17928,
#17929,#17930,#17931,#17932,#17933,#17934,#17935,#17936,#17937,#17938,#17939,
#17940,#17941,#17942,#17943,#17944,#17945,#17946,#17947,#17948),
 .UNSPECIFIED.,.F.,.F.,(4,2,2,2,2,2,2,2,2,2,2,2,2,2,2,2,2,4),(12.4219370484953,
12.4336739434024,12.5069599844754,12.582242359428,12.6574519243816,12.7299629676721,
12.8058471386926,12.8802164895036,12.9530740102056,13.0295128346491,13.1030309691241,
13.1776505229453,13.2531289951954,13.3258184291418,13.4017291063575,13.4763611441305,
13.5490436531927,13.6255081123504),.UNSPECIFIED.);
#837=B_SPLINE_CURVE_WITH_KNOTS('',3,(#17949,#17950,#17951,#17952,#17953,
#17954,#17955,#17956,#17957,#17958,#17959,#17960,#17961,#17962,#17963,#17964,
#17965,#17966,#17967,#17968,#17969,#17970,#17971,#17972,#17973,#17974,#17975,
#17976,#17977,#17978,#17979,#17980,#17981,#17982,#17983,#17984),
 .UNSPECIFIED.,.F.,.F.,(4,2,2,2,2,2,2,2,2,2,2,2,2,2,2,2,2,4),(8.7076043136218,
8.77228185453319,8.84523584591332,8.91920100935851,8.99489701762563,9.06717503350083,
9.14197377622361,9.21778488216681,9.2907019327574,9.36647805600043,9.43982904332821,
9.51358887943921,9.58930403779362,9.66163574037612,9.73622612410351,9.81192490828735,
9.88464155555956,9.90796673370336),.UNSPECIFIED.);
#838=B_SPLINE_CURVE_WITH_KNOTS('',3,(#17989,#17990,#17991,#17992,#17993,
#17994,#17995,#17996,#17997,#17998,#17999,#18000,#18001,#18002,#18003,#18004,
#18005,#18006,#18007,#18008,#18009,#18010,#18011,#18012,#18013,#18014,#18015,
#18016,#18017,#18018,#18019,#18020,#18021,#18022,#18023,#18024),
 .UNSPECIFIED.,.F.,.F.,(4,2,2,2,2,2,2,2,2,2,2,2,2,2,2,2,2,4),(11.2186140020348,
11.2423844354747,11.3152680450516,11.3911530468487,11.4659141859847,11.5384305455132,
11.6143334741864,11.6882621514422,11.7618221629515,11.8377704143951,11.9108541811434,
11.9869038522642,12.0618712560632,12.1343266856154,12.2102089949707,12.2843410369651,
12.3574970509075,12.4219370484953),.UNSPECIFIED.);
#839=B_SPLINE_CURVE_WITH_KNOTS('',3,(#18025,#18026,#18027,#18028,#18029,
#18030,#18031,#18032,#18033,#18034,#18035,#18036,#18037,#18038,#18039,#18040,
#18041,#18042,#18043,#18044,#18045,#18046,#18047,#18048,#18049,#18050,#18051,
#18052,#18053,#18054,#18055,#18056,#18057,#18058,#18059,#18060),
 .UNSPECIFIED.,.F.,.F.,(4,2,2,2,2,2,2,2,2,2,2,2,2,2,2,2,2,4),(9.90796673370336,
9.96019092336532,10.0341032107759,10.1076661950525,10.1841727231514,10.2566639152439,
10.3310840557284,10.4067886417102,10.479272885833,10.5545369162698,10.6289792715137,
10.7022896323962,10.7785115766127,10.8511823564967,10.9253413608401,11.0010205408586,
11.0733316430189,11.1084872386129),.UNSPECIFIED.);
#840=B_SPLINE_CURVE_WITH_KNOTS('',3,(#18065,#18066,#18067,#18068,#18069,
#18070,#18071,#18072,#18073,#18074,#18075,#18076,#18077,#18078,#18079,#18080,
#18081,#18082,#18083,#18084,#18085,#18086,#18087,#18088,#18089,#18090,#18091,
#18092,#18093,#18094,#18095,#18096,#18097,#18098,#18099,#18100),
 .UNSPECIFIED.,.F.,.F.,(4,2,2,2,2,2,2,2,2,2,2,2,2,2,2,2,2,4),(10.0149003245173,
10.0510187671742,10.1268082021235,10.1999760315649,10.2760177990289,10.3494433562341,
10.4234561945758,10.499367171396,10.5718669419739,10.6467132074588,10.7226146491072,
10.7955786855985,10.8713899348627,10.9453350224554,11.0191461453506,11.0950946883506,
11.1677414366375,11.2186140020348),.UNSPECIFIED.);
#841=B_SPLINE_CURVE_WITH_KNOTS('',3,(#18101,#18102,#18103,#18104,#18105,
#18106,#18107,#18108,#18109,#18110,#18111,#18112,#18113,#18114,#18115,#18116,
#18117,#18118,#18119,#18120,#18121,#18122,#18123,#18124,#18125,#18126,#18127,
#18128,#18129,#18130,#18131,#18132,#18133,#18134,#18135,#18136),
 .UNSPECIFIED.,.F.,.F.,(4,2,2,2,2,2,2,2,2,2,2,2,2,2,2,2,2,4),(11.1084872386129,
11.1483283739535,11.2234366551377,11.2991180761832,11.3729850850114,11.4460551399792,
11.5219539304636,11.5949779932755,11.6702784418692,11.7452091132129,11.8174948284876,
11.8931711695511,11.9672655283304,12.0400035862207,12.1161545493962,12.1894019596549,
12.2640057912728,12.3085142855165),.UNSPECIFIED.);
#842=B_SPLINE_CURVE_WITH_KNOTS('',3,(#18141,#18142,#18143,#18144,#18145,
#18146,#18147,#18148,#18149,#18150,#18151,#18152,#18153,#18154,#18155,#18156,
#18157,#18158,#18159,#18160,#18161,#18162,#18163,#18164,#18165,#18166,#18167,
#18168,#18169,#18170,#18171,#18172,#18173,#18174,#18175,#18176),
 .UNSPECIFIED.,.F.,.F.,(4,2,2,2,2,2,2,2,2,2,2,2,2,2,2,2,2,4),(8.81118131706356,
8.85988219698284,8.93431829400909,9.00794050109038,9.08449514330149,9.15729385741128,
9.23177017479016,9.30767841987432,9.38025515534607,9.45557394481698,9.53062772699601,
9.60400921817289,9.6802923492869,9.75334765731488,9.82757672494492,9.90347475980174,
9.97595264247102,10.0149003245173),.UNSPECIFIED.);
#843=B_SPLINE_CURVE_WITH_KNOTS('',3,(#18177,#18178,#18179,#18180,#18181,
#18182,#18183,#18184,#18185,#18186,#18187,#18188,#18189,#18190,#18191,#18192,
#18193,#18194,#18195,#18196,#18197,#18198,#18199,#18200,#18201,#18202,#18203,
#18204,#18205,#18206,#18207,#18208,#18209,#18210,#18211,#18212),
 .UNSPECIFIED.,.F.,.F.,(4,2,2,2,2,2,2,2,2,2,2,2,2,2,2,2,2,4),(12.3085142855165,
12.339197606822,12.4116248037092,12.4873199113833,12.5616695432387,12.6341950359927,
12.7106250508666,12.7841200263037,12.8581561559303,12.9336293939092,13.0062766775809,
13.0819505646389,13.1564677944215,13.2288031792112,13.3044990905332,13.3781864966043,
13.4516243658145,13.5089129023366),.UNSPECIFIED.);
#844=B_SPLINE_CURVE_WITH_KNOTS('',3,(#18217,#18218,#18219,#18220,#18221,
#18222,#18223,#18224,#18225,#18226,#18227,#18228,#18229,#18230,#18231,#18232,
#18233,#18234,#18235,#18236,#18237,#18238,#18239,#18240,#18241,#18242,#18243,
#18244,#18245,#18246,#18247,#18248,#18249,#18250,#18251,#18252),
 .UNSPECIFIED.,.F.,.F.,(4,2,2,2,2,2,2,2,2,2,2,2,2,2,2,2,2,4),(7.60809265701202,
7.66925043325465,7.74258865796053,7.81657848823611,7.89244187032674,7.96489086528524,
8.03971391088468,8.11618116990066,8.18914360620284,8.26495689720756,8.33874274405452,
8.41255092435251,8.488446529945,8.56101160072265,8.63565128320245,8.71151763515169,
8.78428725689606,8.81118131706356),.UNSPECIFIED.);
#845=B_SPLINE_CURVE_WITH_KNOTS('',3,(#18253,#18254,#18255,#18256,#18257,
#18258,#18259,#18260,#18261,#18262,#18263,#18264,#18265,#18266,#18267,#18268,
#18269,#18270,#18271,#18272,#18273,#18274,#18275,#18276,#18277,#18278,#18279,
#18280,#18281,#18282,#18283,#18284,#18285,#18286,#18287,#18288),
 .UNSPECIFIED.,.F.,.F.,(4,2,2,2,2,2,2,2,2,2,2,2,2,2,2,2,2,4),(13.5089129023366,
13.5273209464022,13.6001655562817,13.6761527551668,13.7508680671827,13.8231229487502,
13.8987942754795,13.9726772741613,14.0456959794494,14.1216133937442,14.1946532931299,
14.2698607489188,14.3448115065662,14.4170990904062,14.4927679373319,14.5668818733047,
14.6395814079699,14.70876682955),.UNSPECIFIED.);
#846=B_SPLINE_CURVE_WITH_KNOTS('',3,(#18293,#18294,#18295,#18296,#18297,
#18298,#18299,#18300,#18301,#18302,#18303,#18304,#18305,#18306,#18307,#18308,
#18309,#18310,#18311,#18312,#18313,#18314,#18315,#18316,#18317,#18318,#18319,
#18320,#18321,#18322,#18323,#18324,#18325,#18326,#18327,#18328),
 .UNSPECIFIED.,.F.,.F.,(4,2,2,2,2,2,2,2,2,2,2,2,2,2,2,2,2,4),(6.40518341674792,
6.4784162628992,6.5511518896874,6.62561134850426,6.70147691401884,6.77402804045823,
6.84933011752558,6.9242680029148,6.99763001454459,7.07389505573071,7.14687415420526,
7.22108374957461,7.29693654400393,7.36937584557916,7.44442249461365,7.52008495994635,
7.59323021339548,7.60809265701202),.UNSPECIFIED.);
#847=B_SPLINE_CURVE_WITH_KNOTS('',3,(#18329,#18330,#18331,#18332,#18333,
#18334,#18335,#18336,#18337,#18338,#18339,#18340,#18341,#18342,#18343,#18344,
#18345,#18346,#18347,#18348,#18349,#18350,#18351,#18352,#18353,#18354,#18355,
#18356,#18357,#18358,#18359,#18360,#18361,#18362,#18363,#18364,#18365,#18366),
 .UNSPECIFIED.,.F.,.F.,(4,2,2,2,2,2,2,2,2,2,2,2,2,2,2,2,2,2,4),(14.70876682955,
14.7157544850024,14.7890208603349,14.8635448396388,14.9387594701541,15.0112023807248,
15.0868928606138,15.1612646656571,15.2337659834846,15.3102205634935,15.383736740473,
15.4577093324676,15.5332071233297,15.6058763383245,15.6815523186699,15.7560929436209,
15.8284176747741,15.9041132391376,15.9090867771917),.UNSPECIFIED.);
#848=B_SPLINE_CURVE_WITH_KNOTS('',3,(#18371,#18372,#18373,#18374,#18375,
#18376,#18377,#18378,#18379,#18380,#18381,#18382,#18383,#18384,#18385,#18386,
#18387,#18388,#18389,#18390,#18391,#18392,#18393,#18394,#18395,#18396,#18397,
#18398,#18399,#18400,#18401,#18402,#18403,#18404,#18405,#18406,#18407,#18408),
 .UNSPECIFIED.,.F.,.F.,(4,2,2,2,2,2,2,2,2,2,2,2,2,2,2,2,2,2,4),(5.20254529202766,
5.21114452011972,5.28697167508392,5.35938153580539,5.43419390254545,5.51053572229188,
5.58348377267585,5.65928384720493,5.73298406017818,5.80677715192569,5.88263419023285,
5.95514950133274,6.02977380367191,6.1056037044028,6.17835739435224,6.25393740620464,
6.32827226106894,6.40187723168649,6.40518341674792),.UNSPECIFIED.);
#849=B_SPLINE_CURVE_WITH_KNOTS('',3,(#18409,#18410,#18411,#18412,#18413,
#18414,#18415,#18416,#18417,#18418,#18419,#18420,#18421,#18422,#18423,#18424,
#18425,#18426,#18427,#18428,#18429,#18430,#18431,#18432,#18433,#18434,#18435,
#18436,#18437,#18438,#18439,#18440,#18441,#18442,#18443,#18444),
 .UNSPECIFIED.,.F.,.F.,(4,2,2,2,2,2,2,2,2,2,2,2,2,2,2,2,2,4),(15.9090867771917,
15.9778238334733,16.0512144010312,16.1269370761519,16.1998050074649,16.2757053629313,
16.3504486400594,16.4227045323351,16.4983779027584,16.572288419036,16.6452693381883,
16.7212171599794,16.7942842435471,16.8694133182641,16.9443956867004,17.0166978074018,
17.0923712727689,17.1089856849962),.UNSPECIFIED.);
#850=B_SPLINE_CURVE_WITH_KNOTS('',3,(#18449,#18450,#18451,#18452,#18453,
#18454,#18455,#18456,#18457,#18458,#18459,#18460,#18461,#18462,#18463,#18464,
#18465,#18466,#18467,#18468,#18469,#18470,#18471,#18472,#18473,#18474,#18475,
#18476,#18477,#18478,#18479,#18480,#18481,#18482,#18483,#18484),
 .UNSPECIFIED.,.F.,.F.,(4,2,2,2,2,2,2,2,2,2,2,2,2,2,2,2,2,4),(4.00022881423318,
4.02070918614415,4.09654371873197,4.16908222613698,4.24438030317169,4.31921153434457,
4.39256635461615,4.46882620393768,4.54173975558394,4.61594236312608,4.69176141251603,
4.76417452467247,4.83921434981631,4.9147582004447,4.98789307802441,5.06390455041936,
5.13716531906636,5.20254529202766),.UNSPECIFIED.);
#851=B_SPLINE_CURVE_WITH_KNOTS('',3,(#18485,#18486,#18487,#18488,#18489,
#18490,#18491,#18492,#18493,#18494,#18495,#18496,#18497,#18498,#18499,#18500,
#18501,#18502,#18503,#18504,#18505,#18506,#18507,#18508,#18509,#18510,#18511,
#18512,#18513,#18514,#18515,#18516,#18517,#18518,#18519,#18520),
 .UNSPECIFIED.,.F.,.F.,(4,2,2,2,2,2,2,2,2,2,2,2,2,2,2,2,2,4),(17.1089856849962,
17.1665161724971,17.2391906728527,17.315397504744,17.3886940669098,17.4631529044837,
17.5384017461112,17.6108726881494,17.6865706351,17.7609758822802,17.8334662647143,
17.909956936562,17.9835054396964,18.0574290155657,18.1329626682353,18.2056647279776,
18.2813547593944,18.3094927861098),.UNSPECIFIED.);
#852=B_SPLINE_CURVE_WITH_KNOTS('',3,(#18525,#18526,#18527,#18528,#18529,
#18530,#18531,#18532,#18533,#18534,#18535,#18536,#18537,#18538,#18539,#18540,
#18541,#18542,#18543,#18544,#18545,#18546,#18547,#18548,#18549,#18550,#18551,
#18552,#18553,#18554,#18555,#18556,#18557,#18558,#18559,#18560),
 .UNSPECIFIED.,.F.,.F.,(4,2,2,2,2,2,2,2,2,2,2,2,2,2,2,2,2,4),(2.79777820474308,
2.82974055501476,2.90596677502876,2.97891261559774,3.05471220698905,3.12833745896342,
3.20212780791041,3.27795807200847,3.35043537338853,3.42505679873134,3.50086219836848,
3.57361214287228,3.64918997002519,3.72343368786902,3.79703376475382,3.87357013783338,
3.94625404048576,4.00022881423318),.UNSPECIFIED.);
#853=B_SPLINE_CURVE_WITH_KNOTS('',3,(#18561,#18562,#18563,#18564,#18565,
#18566,#18567,#18568,#18569,#18570,#18571,#18572,#18573,#18574,#18575,#18576,
#18577,#18578,#18579,#18580,#18581,#18582,#18583,#18584,#18585,#18586,#18587,
#18588,#18589,#18590,#18591,#18592,#18593,#18594,#18595,#18596),
 .UNSPECIFIED.,.F.,.F.,(4,2,2,2,2,2,2,2,2,2,2,2,2,2,2,2,2,4),(18.3094927861098,
18.3559299172002,18.4282566986793,18.5039638888353,18.5777086627907,18.6510659398855,
18.7268259021107,18.7997279632351,18.8755572416397,18.950339388976,19.0226087972395,
19.0982961026059,19.1722449066968,19.245202097094,19.3211912918155,19.3942961629852,
19.4693627363339,19.5096597635899),.UNSPECIFIED.);
#854=B_SPLINE_CURVE_WITH_KNOTS('',3,(#18601,#18602,#18603,#18604,#18605,
#18606,#18607,#18608,#18609,#18610,#18611,#18612,#18613,#18614,#18615,#18616,
#18617,#18618,#18619,#18620,#18621,#18622,#18623,#18624,#18625,#18626,#18627,
#18628,#18629,#18630,#18631,#18632,#18633,#18634,#18635,#18636),
 .UNSPECIFIED.,.F.,.F.,(4,2,2,2,2,2,2,2,2,2,2,2,2,2,2,2,2,4),(1.59584813976879,
1.64030318449184,1.71503898288323,1.78839885504719,1.8646663227141,1.93752618397062,
2.01173424115385,2.08753149252248,2.1599312617715,2.23497686627159,2.31041262209493,
2.3835493496218,2.45956486633182,2.53275945264887,2.60674043699168,2.68254322671225,
2.75492629137578,2.79777820474308),.UNSPECIFIED.);
#855=B_SPLINE_CURVE_WITH_KNOTS('',3,(#18637,#18638,#18639,#18640,#18641,
#18642,#18643,#18644,#18645,#18646,#18647,#18648,#18649,#18650,#18651,#18652,
#18653,#18654,#18655,#18656,#18657,#18658,#18659,#18660,#18661,#18662,#18663,
#18664,#18665,#18666,#18667,#18668,#18669,#18670,#18671,#18672),
 .UNSPECIFIED.,.F.,.F.,(4,2,2,2,2,2,2,2,2,2,2,2,2,2,2,2,2,4),(19.5096597635899,
19.5443874072969,19.6167161417866,19.6924060411691,19.7665924754453,19.8392556153294,
19.9155069695267,19.988844146723,20.0632535067116,20.1385470836438,20.2110575105348,
20.2867746653084,20.361223770174,20.4337163429507,20.5102537253887,20.5838448538204,
20.6577345355442,20.7103833929792),.UNSPECIFIED.);
#856=B_SPLINE_CURVE_WITH_KNOTS('',3,(#18677,#18678,#18679,#18680,#18681,
#18682,#18683,#18684,#18685,#18686,#18687,#18688,#18689,#18690,#18691,#18692,
#18693,#18694,#18695,#18696,#18697,#18698,#18699,#18700,#18701,#18702,#18703,
#18704,#18705,#18706,#18707,#18708,#18709,#18710,#18711,#18712),
 .UNSPECIFIED.,.F.,.F.,(4,2,2,2,2,2,2,2,2,2,2,2,2,2,2,2,2,4),(0.393548424805639,
0.4508158900413,0.524378226173459,0.598178030137416,0.673993636458548,0.746445315016936,
0.821076220256436,0.896869346725983,0.969627610190531,1.04521583748751,
1.11938021843885,1.19298764736334,1.26953416876338,1.34217863689082,1.41664190675191,
1.49245745846437,1.56499651097925,1.59584813976879),.UNSPECIFIED.);
#857=B_SPLINE_CURVE_WITH_KNOTS('',3,(#18713,#18714,#18715,#18716,#18717,
#18718,#18719,#18720,#18721,#18722,#18723,#18724,#18725,#18726,#18727,#18728,
#18729,#18730,#18731,#18732,#18733,#18734,#18735,#18736,#18737,#18738,#18739,
#18740,#18741,#18742,#18743,#18744,#18745,#18746,#18747,#18748),
 .UNSPECIFIED.,.F.,.F.,(4,2,2,2,2,2,2,2,2,2,2,2,2,2,2,2,2,4),(20.7103833929792,
20.7333144658301,20.8060594577103,20.8817750110343,20.9563949805616,21.0287361646161,
21.1044665243677,21.1782556223629,21.2515939142169,21.3274014498813,21.4003476115493,
21.4761225443347,21.550953543773,21.6232483768027,21.6989610391312,21.7729579939401,
21.8459054932902,21.9110024905134),.UNSPECIFIED.);
#858=B_SPLINE_CURVE_WITH_KNOTS('',3,(#18754,#18755,#18756,#18757,#18758,
#18759,#18760,#18761),.UNSPECIFIED.,.F.,.F.,(4,2,2,4),(22.3024920269109,
22.3688483291561,22.4097534378368,22.450488682359),.UNSPECIFIED.);
#859=B_SPLINE_CURVE_WITH_KNOTS('',3,(#18767,#18768,#18769,#18770,#18771,
#18772,#18773,#18774,#18775,#18776,#18777,#18778,#18779,#18780,#18781,#18782,
#18783,#18784,#18785,#18786,#18787,#18788,#18789,#18790,#18791,#18792,#18793,
#18794,#18795,#18796,#18797,#18798,#18799,#18800,#18801,#18802,#18803,#18804),
 .UNSPECIFIED.,.F.,.F.,(4,2,2,2,2,2,2,2,2,2,2,2,2,2,2,2,2,2,4),(21.1027737430364,
21.1049994597819,21.1806496975336,21.2549908073923,21.327447317095,21.4038709246568,
21.477356515211,21.5512705483181,21.6267378367605,21.6993771262732,21.7750151016799,
21.8495253198282,21.9218097649896,21.9974664960608,22.0711470350727,22.1444847067024,
22.2201772479808,22.2930155883394,22.3024920269109),.UNSPECIFIED.);
#860=B_SPLINE_CURVE_WITH_KNOTS('',3,(#18805,#18806,#18807,#18808,#18809,
#18810,#18811,#18812,#18813,#18814,#18815,#18816,#18817,#18818,#18819,#18820,
#18821,#18822,#18823,#18824,#18825,#18826,#18827,#18828,#18829,#18830,#18831,
#18832,#18833,#18834,#18835,#18836,#18837,#18838,#18839,#18840),
 .UNSPECIFIED.,.F.,.F.,(4,2,2,2,2,2,2,2,2,2,2,2,2,2,2,2,2,4),(9.99999992579797E-7,
0.071600740188014,0.145227781903171,0.219826582094929,0.293153757552435,
0.369389729999796,0.442157073718064,0.516332458908302,0.592067666639851,
0.664417382066663,0.739430243920045,0.814714869378155,0.887815779298927,
0.963796320979993,1.03688481767441,1.11082953216144,1.18656756573286,1.2009375425295),
 .UNSPECIFIED.);
#861=B_SPLINE_CURVE_WITH_KNOTS('',3,(#18845,#18846,#18847,#18848,#18849,
#18850,#18851,#18852,#18853,#18854,#18855,#18856,#18857,#18858,#18859,#18860,
#18861,#18862,#18863,#18864,#18865,#18866,#18867,#18868,#18869,#18870,#18871,
#18872,#18873,#18874,#18875,#18876,#18877,#18878,#18879,#18880),
 .UNSPECIFIED.,.F.,.F.,(4,2,2,2,2,2,2,2,2,2,2,2,2,2,2,2,2,4),(19.9035199005169,
19.9175621070154,19.9931913738258,20.0670419245932,20.1400064577233,20.2158912543276,
20.2888990748213,20.3640374087997,20.4389565108213,20.5112080306681,20.586835687514,
20.6609182233636,20.7335680720135,20.8097095325252,20.8829447283432,20.9574044024021,
21.0325881211151,21.1027737430364),.UNSPECIFIED.);
#862=B_SPLINE_CURVE_WITH_KNOTS('',3,(#18881,#18882,#18883,#18884,#18885,
#18886,#18887,#18888,#18889,#18890,#18891,#18892,#18893,#18894,#18895,#18896,
#18897,#18898,#18899,#18900,#18901,#18902,#18903,#18904,#18905,#18906,#18907,
#18908,#18909,#18910,#18911,#18912,#18913,#18914,#18915,#18916),
 .UNSPECIFIED.,.F.,.F.,(4,2,2,2,2,2,2,2,2,2,2,2,2,2,2,2,2,4),(1.2009375425295,
1.25888640597054,1.33366417438652,1.40973038664347,1.48263642047109,1.5583965827547,
1.63190591222369,1.70565551039325,1.78141853327558,1.85381950408462,1.92839963526476,
2.00414029370891,2.07684901974681,2.1523858558826,2.22649613810886,2.30005340880839,
2.37654787318782,2.40222076469358),.UNSPECIFIED.);
#863=B_SPLINE_CURVE_WITH_KNOTS('',3,(#18921,#18922,#18923,#18924,#18925,
#18926,#18927,#18928,#18929,#18930,#18931,#18932,#18933,#18934,#18935,#18936,
#18937,#18938,#18939,#18940,#18941,#18942,#18943,#18944,#18945,#18946,#18947,
#18948,#18949,#18950,#18951,#18952,#18953,#18954,#18955,#18956),
 .UNSPECIFIED.,.F.,.F.,(4,2,2,2,2,2,2,2,2,2,2,2,2,2,2,2,2,4),(18.7039793906749,
18.7293029617149,18.8056980625727,18.8791586520591,18.953131415963,19.0285702841427,
19.101183913415,19.1768157473824,19.2512987633797,19.3235895776797,19.3992426079428,
19.4728962017746,19.5462765111672,19.621939128249,19.6947504523395,19.7706652930376,
19.8453478358706,19.9035199005169),.UNSPECIFIED.);
#864=B_SPLINE_CURVE_WITH_KNOTS('',3,(#18957,#18958,#18959,#18960,#18961,
#18962,#18963,#18964,#18965,#18966,#18967,#18968,#18969,#18970,#18971,#18972,
#18973,#18974,#18975,#18976,#18977,#18978,#18979,#18980,#18981,#18982,#18983,
#18984,#18985,#18986,#18987,#18988,#18989,#18990,#18991,#18992),
 .UNSPECIFIED.,.F.,.F.,(4,2,2,2,2,2,2,2,2,2,2,2,2,2,2,2,2,4),(2.40222076469358,
2.44914093359071,2.52355349120749,2.59931628116421,2.67180565378717,2.74706105662188,
2.82174169130443,2.89505148167998,2.97126698121376,3.04407469365999,3.11823210506219,
3.1939764896512,3.26632610002547,3.34132049862734,3.41670007479089,3.48978674293741,
3.56575031853941,3.60344585613563),.UNSPECIFIED.);
#865=B_SPLINE_CURVE_WITH_KNOTS('',3,(#18997,#18998,#18999,#19000,#19001,
#19002,#19003,#19004,#19005,#19006,#19007,#19008,#19009,#19010,#19011,#19012,
#19013,#19014,#19015,#19016,#19017,#19018,#19019,#19020,#19021,#19022,#19023,
#19024,#19025,#19026,#19027,#19028,#19029,#19030,#19031,#19032),
 .UNSPECIFIED.,.F.,.F.,(4,2,2,2,2,2,2,2,2,2,2,2,2,2,2,2,2,4),(17.5045386553045,
17.5418586812021,17.6177208347371,17.6907089519883,17.7659355012861,17.8408305830793,
17.9130759416574,17.9887070096763,18.0627660821069,18.1354499558134,18.2115653258401,
18.2847777274801,18.3593124155404,18.4344694246712,18.506860849091,18.5825116326314,
18.6568267189528,18.7039793906749),.UNSPECIFIED.);
#866=B_SPLINE_CURVE_WITH_KNOTS('',3,(#19033,#19034,#19035,#19036,#19037,
#19038,#19039,#19040,#19041,#19042,#19043,#19044,#19045,#19046,#19047,#19048,
#19049,#19050,#19051,#19052,#19053,#19054,#19055,#19056,#19057,#19058,#19059,
#19060,#19061,#19062,#19063,#19064,#19065,#19066,#19067,#19068),
 .UNSPECIFIED.,.F.,.F.,(4,2,2,2,2,2,2,2,2,2,2,2,2,2,2,2,2,4),(3.60344585613563,
3.63889200144254,3.71282234596637,3.78857215811946,3.86090451389972,3.93566757169027,
4.01183674496613,4.08473249054017,4.16048010314507,4.23405178231718,4.30779143621035,
4.38356860368306,4.45599465938229,4.53056481489909,4.606317231512,4.67901715347343,
4.75454308534004,4.80478993825526),.UNSPECIFIED.);
#867=B_SPLINE_CURVE_WITH_KNOTS('',3,(#19073,#19074,#19075,#19076,#19077,
#19078,#19079,#19080,#19081,#19082,#19083,#19084,#19085,#19086,#19087,#19088,
#19089,#19090,#19091,#19092,#19093,#19094,#19095,#19096,#19097,#19098,#19099,
#19100,#19101,#19102,#19103,#19104,#19105,#19106,#19107,#19108),
 .UNSPECIFIED.,.F.,.F.,(4,2,2,2,2,2,2,2,2,2,2,2,2,2,2,2,2,4),(16.3050203760452,
16.3548731718868,16.4302954221762,16.5028947557627,16.5785325996716,16.6530000240717,
16.7253099644208,16.800971419953,16.8746095269004,16.9480460530331,17.0236904467053,
17.0964860271612,17.1724973404452,17.2471596152608,17.319381368035,17.3950166419569,
17.4688472747823,17.5045386553045),.UNSPECIFIED.);
#868=B_SPLINE_CURVE_WITH_KNOTS('',3,(#19109,#19110,#19111,#19112,#19113,
#19114,#19115,#19116,#19117,#19118,#19119,#19120,#19121,#19122,#19123,#19124,
#19125,#19126,#19127,#19128,#19129,#19130,#19131,#19132,#19133,#19134,#19135,
#19136,#19137,#19138,#19139,#19140,#19141,#19142,#19143,#19144),
 .UNSPECIFIED.,.F.,.F.,(4,2,2,2,2,2,2,2,2,2,2,2,2,2,2,2,2,4),(4.80478993825526,
4.82873212967197,4.90228155462143,4.97876535710322,5.05139730211433,5.12580123479856,
5.20158249025959,5.2740707767987,5.34931707642891,5.42409257488621,5.49739681707695,
5.57360418155691,5.64646503610294,5.72061649399095,5.79638216249746,5.86874457180556,
5.94373268071591,6.00642764136115),.UNSPECIFIED.);
#869=B_SPLINE_CURVE_WITH_KNOTS('',3,(#19149,#19150,#19151,#19152,#19153,
#19154,#19155,#19156,#19157,#19158,#19159,#19160,#19161,#19162,#19163,#19164,
#19165,#19166,#19167,#19168,#19169,#19170,#19171,#19172,#19173,#19174,#19175,
#19176,#19177,#19178,#19179,#19180,#19181,#19182,#19183,#19184),
 .UNSPECIFIED.,.F.,.F.,(4,2,2,2,2,2,2,2,2,2,2,2,2,2,2,2,2,4),(15.1052499210504,
15.1675158452439,15.2423988721291,15.3146509504745,15.3902976012197,15.4643450279264,
15.5370760734893,15.6131774634138,15.6863787117015,15.761002222048,15.8361443918783,
15.9085286335628,15.9841921557106,16.0584929502958,16.1310020353728,16.2073806551034,
16.2808278140705,16.3050203760452),.UNSPECIFIED.);
#870=B_SPLINE_CURVE_WITH_KNOTS('',3,(#19185,#19186,#19187,#19188,#19189,
#19190,#19191,#19192,#19193,#19194,#19195,#19196,#19197,#19198,#19199,#19200,
#19201,#19202,#19203,#19204,#19205,#19206,#19207,#19208,#19209,#19210,#19211,
#19212,#19213,#19214,#19215,#19216,#19217,#19218,#19219,#19220),
 .UNSPECIFIED.,.F.,.F.,(4,2,2,2,2,2,2,2,2,2,2,2,2,2,2,2,2,4),(6.00642764136115,
6.01921979787647,6.09230411676459,6.16826312791688,6.24147045508006,6.31539850918389,
6.39117217319509,6.46353078683716,6.5382914339967,6.61457567378796,6.6874731272014,
6.76322069995753,6.83686681762636,6.91060870469478,6.98641213318798,7.05887567245481,
7.13344818869197,7.20797850375824),.UNSPECIFIED.);
#871=B_SPLINE_CURVE_WITH_KNOTS('',3,(#19225,#19226,#19227,#19228,#19229,
#19230,#19231,#19232,#19233,#19234,#19235,#19236,#19237,#19238,#19239,#19240,
#19241,#19242,#19243,#19244,#19245,#19246,#19247,#19248,#19249,#19250,#19251,
#19252,#19253,#19254,#19255,#19256,#19257,#19258,#19259,#19260),
 .UNSPECIFIED.,.F.,.F.,(4,2,2,2,2,2,2,2,2,2,2,2,2,2,2,2,2,4),(13.9056073328072,
13.979733684865,14.0541976690322,14.1265393105317,14.2022213563442,14.2758559700236,
14.3493613399648,14.4249998082098,14.4977914544797,14.573912278901,14.6485663529743,
14.7208084008114,14.7964618439306,14.8702844710759,14.9433557153578,15.0192074340945,
15.0921875748939,15.1052499210504),.UNSPECIFIED.);
#872=B_SPLINE_CURVE_WITH_KNOTS('',3,(#19261,#19262,#19263,#19264,#19265,
#19266,#19267,#19268,#19269,#19270,#19271,#19272,#19273,#19274,#19275,#19276,
#19277,#19278,#19279,#19280,#19281,#19282,#19283,#19284,#19285,#19286,#19287,
#19288,#19289,#19290,#19291,#19292,#19293,#19294,#19295,#19296,#19297,#19298),
 .UNSPECIFIED.,.F.,.F.,(4,2,2,2,2,2,2,2,2,2,2,2,2,2,2,2,2,2,4),(7.20797850375824,
7.20922458919542,7.28192775231267,7.3574553433693,7.43173500783957,7.50528881442058,
7.58177474025056,7.65445788369708,7.72886560966757,7.80467738626606,7.87717774144433,
7.95242751469966,8.02730916972658,8.10062009072416,8.17683211153858,8.24975800118347,
8.32391592638887,8.39971483158691,8.41018693810434),.UNSPECIFIED.);
#873=B_SPLINE_CURVE_WITH_KNOTS('',3,(#19303,#19304,#19305,#19306,#19307,
#19308,#19309,#19310,#19311,#19312,#19313,#19314,#19315,#19316,#19317,#19318,
#19319,#19320,#19321,#19322,#19323,#19324,#19325,#19326,#19327,#19328,#19329,
#19330,#19331,#19332,#19333,#19334,#19335,#19336,#19337,#19338,#19339,#19340),
 .UNSPECIFIED.,.F.,.F.,(4,2,2,2,2,2,2,2,2,2,2,2,2,2,2,2,2,2,4),(12.7053500380718,
12.715500408312,12.7911747085665,12.8652227682113,12.9380133372392,13.0141133728098,
13.0873155564923,13.1620400374673,13.2371797690825,13.3095699175679,13.3852583231407,
13.4595570740892,13.5321116326848,13.6084863643335,13.6819321581728,13.7560626688118,
13.8314806701097,13.9040775820415,13.9056073328072),.UNSPECIFIED.);
#874=B_SPLINE_CURVE_WITH_KNOTS('',3,(#19341,#19342,#19343,#19344,#19345,
#19346,#19347,#19348,#19349,#19350,#19351,#19352,#19353,#19354,#19355,#19356,
#19357,#19358,#19359,#19360,#19361,#19362,#19363,#19364,#19365,#19366,#19367,
#19368,#19369,#19370,#19371,#19372,#19373,#19374,#19375,#19376),
 .UNSPECIFIED.,.F.,.F.,(4,2,2,2,2,2,2,2,2,2,2,2,2,2,2,2,2,4),(8.41018693810434,
8.47210288948872,8.54709729504254,8.62270255411287,8.69579673625766,8.77176395924554,
8.84504825099315,8.91898641394924,8.99479579943711,9.06719302368103,9.14196382255198,
9.21837305385914,9.29128438161236,9.36704463649688,9.44077591825568,9.51453237511723,
9.59037386733617,9.61221885207275),.UNSPECIFIED.);
#875=B_SPLINE_CURVE_WITH_KNOTS('',3,(#19381,#19382,#19383,#19384,#19385,
#19386,#19387,#19388,#19389,#19390,#19391,#19392,#19393,#19394,#19395,#19396,
#19397,#19398,#19399,#19400,#19401,#19402,#19403,#19404,#19405,#19406,#19407,
#19408,#19409,#19410,#19411,#19412,#19413,#19414,#19415,#19416),
 .UNSPECIFIED.,.F.,.F.,(4,2,2,2,2,2,2,2,2,2,2,2,2,2,2,2,2,4),(11.5053094523182,
11.5268488992701,11.6025634962346,11.6762068956174,11.7497924810252,11.8254376640932,
11.8982374792771,11.9744787611083,12.0491370912012,12.1214119953902,12.1970956139134,
12.2709225306323,12.3440655074962,12.4199194393904,12.4929037111634,12.5683452713175,
12.6432286827158,12.7053500380718),.UNSPECIFIED.);
#876=B_SPLINE_CURVE_WITH_KNOTS('',3,(#19417,#19418,#19419,#19420,#19421,
#19422,#19423,#19424,#19425,#19426,#19427,#19428,#19429,#19430,#19431,#19432,
#19433,#19434,#19435,#19436,#19437,#19438,#19439,#19440,#19441,#19442,#19443,
#19444,#19445,#19446,#19447,#19448,#19449,#19450,#19451,#19452),
 .UNSPECIFIED.,.F.,.F.,(4,2,2,2,2,2,2,2,2,2,2,2,2,2,2,2,2,4),(9.61221885207275,
9.66288666337229,9.73747403439585,9.81328637680854,9.88600495943817,9.96154694365518,
10.0359273989204,10.1094979228893,10.1859989158825,10.2587446558326,10.3331687130746,
10.4090226703821,10.4815480891719,10.5568140406692,10.631811171281,10.705141054464,
10.7813706230653,10.8150631151595),.UNSPECIFIED.);
#877=B_SPLINE_CURVE_WITH_KNOTS('',3,(#19457,#19458,#19459,#19460,#19461,
#19462,#19463,#19464,#19465,#19466,#19467,#19468,#19469,#19470,#19471,#19472,
#19473,#19474,#19475,#19476,#19477,#19478,#19479,#19480,#19481,#19482,#19483,
#19484,#19485,#19486,#19487,#19488,#19489,#19490,#19491,#19492),
 .UNSPECIFIED.,.F.,.F.,(4,2,2,2,2,2,2,2,2,2,2,2,2,2,2,2,2,4),(10.3044171497523,
10.3401614858824,10.4140935645159,10.489832598554,10.5621534139354,10.6369182779871,
10.7130332981672,10.7859288776338,10.861677195313,10.9352141470178,11.0089534074536,
11.0847186438897,11.1571276956958,11.2316974123293,11.3043040355563,11.3799904932741,
11.4544634746901,11.5053094523182),.UNSPECIFIED.);
#878=B_SPLINE_CURVE_WITH_KNOTS('',3,(#19493,#19494,#19495,#19496,#19497,
#19498,#19499,#19500,#19501,#19502,#19503,#19504,#19505,#19506,#19507,#19508,
#19509,#19510,#19511,#19512,#19513,#19514,#19515,#19516,#19517,#19518,#19519,
#19520,#19521,#19522,#19523,#19524,#19525,#19526,#19527,#19528),
 .UNSPECIFIED.,.F.,.F.,(4,2,2,2,2,2,2,2,2,2,2,2,2,2,2,2,2,4),(10.8150631151595,
10.8543722558447,10.928549127917,11.0043927799348,11.0768188941975,11.1518322431134,
11.2275640823162,11.3034083276436,11.3775655232947,11.4505952542184,11.5268030118463,
11.6001136025955,11.6751704644753,11.7504138876136,11.8229261851396,11.8987786494732,
11.9731806969486,12.0177749705651),.UNSPECIFIED.);
#879=B_SPLINE_CURVE_WITH_KNOTS('',3,(#19533,#19534,#19535,#19536,#19537,
#19538,#19539,#19540,#19541,#19542,#19543,#19544,#19545,#19546,#19547,#19548,
#19549,#19550,#19551,#19552,#19553,#19554,#19555,#19556,#19557,#19558,#19559,
#19560,#19561,#19562,#19563,#19564,#19565,#19566,#19567,#19568),
 .UNSPECIFIED.,.F.,.F.,(4,2,2,2,2,2,2,2,2,2,2,2,2,2,2,2,2,4),(9.10333053600743,
9.15055193771733,9.22496917372991,9.30072377279127,9.37321466466583,9.44847498318585,
9.52311148303587,9.59642450060639,9.67264449108136,9.74542789452109,9.81958874887466,
9.89532358746586,9.96766812633393,10.0426661407919,10.1179953699147,10.1910837755611,
10.2670501800193,10.3044171497523),.UNSPECIFIED.);
#880=B_SPLINE_CURVE_WITH_KNOTS('',3,(#19569,#19570,#19571,#19572,#19573,
#19574,#19575,#19576,#19577,#19578,#19579,#19580,#19581,#19582,#19583,#19584,
#19585,#19586,#19587,#19588,#19589,#19590,#19591,#19592,#19593,#19594,#19595,
#19596,#19597,#19598,#19599,#19600,#19601,#19602,#19603,#19604),
 .UNSPECIFIED.,.F.,.F.,(4,2,2,2,2,2,2,2,2,2,2,2,2,2,2,2,2,4),(12.0177749705651,
12.0459439977539,12.1224209422467,12.1959701551707,12.2703988259824,12.3459166164042,
12.4186131843801,12.4944189632762,12.5689829374183,12.6415023536567,12.7173389558782,
12.7910721614232,12.864839149528,12.9405736130224,13.0134614850999,13.0899381426276,
13.1646814782178,13.2202175978974),.UNSPECIFIED.);
#881=B_SPLINE_CURVE_WITH_KNOTS('',3,(#19609,#19610,#19611,#19612,#19613,
#19614,#19615,#19616,#19617,#19618,#19619,#19620,#19621,#19622,#19623,#19624,
#19625,#19626,#19627,#19628,#19629,#19630,#19631,#19632,#19633,#19634,#19635,
#19636,#19637,#19638,#19639,#19640,#19641,#19642,#19643,#19644),
 .UNSPECIFIED.,.F.,.F.,(4,2,2,2,2,2,2,2,2,2,2,2,2,2,2,2,2,4),(7.90214345446006,
7.96039945586104,8.03518468932147,8.11120319187168,8.18411460885446,8.25988125009896,
8.33336199006571,8.4071168320765,8.48287370775027,8.55526368666003,8.62984909064281,
8.70558475614216,8.77829819812881,8.8538407735689,8.92791467968878,9.0014762398683,
9.07797636059719,9.10333053600743),.UNSPECIFIED.);
#882=B_SPLINE_CURVE_WITH_KNOTS('',3,(#19645,#19646,#19647,#19648,#19649,
#19650,#19651,#19652,#19653,#19654,#19655,#19656,#19657,#19658,#19659,#19660,
#19661,#19662,#19663,#19664,#19665,#19666,#19667,#19668,#19669,#19670,#19671,
#19672,#19673,#19674,#19675,#19676,#19677,#19678,#19679,#19680),
 .UNSPECIFIED.,.F.,.F.,(4,2,2,2,2,2,2,2,2,2,2,2,2,2,2,2,2,4),(13.2202175978974,
13.2370767530604,13.3128793204275,13.3867903685147,13.460104092076,13.5360416304297,
13.6091088630933,13.6847766992306,13.7597402374587,13.8321156847763,13.9079057206965,
13.982033311037,14.0549791174888,14.1311582866812,14.204439423608,14.2793744030468,
14.354590742388,14.4220042621459),.UNSPECIFIED.);
#883=B_SPLINE_CURVE_WITH_KNOTS('',3,(#19685,#19686,#19687,#19688,#19689,
#19690,#19691,#19692,#19693,#19694,#19695,#19696,#19697,#19698,#19699,#19700,
#19701,#19702,#19703,#19704,#19705,#19706,#19707,#19708,#19709,#19710,#19711,
#19712,#19713,#19714,#19715,#19716,#19717,#19718,#19719,#19720),
 .UNSPECIFIED.,.F.,.F.,(4,2,2,2,2,2,2,2,2,2,2,2,2,2,2,2,2,4),(6.70124289322726,
6.7715290879724,6.84681622467596,6.9213776981955,6.99471361200024,7.07095980223775,
7.14370921775499,7.21789363955208,7.29362513808374,7.36597592622018,7.44099806657252,
7.51623904898732,7.58934725641939,7.66533640932017,7.73840086116704,7.812352957716,
7.88808605229705,7.90214345446006),.UNSPECIFIED.);
#884=B_SPLINE_CURVE_WITH_KNOTS('',3,(#19721,#19722,#19723,#19724,#19725,
#19726,#19727,#19728,#19729,#19730,#19731,#19732,#19733,#19734,#19735,#19736,
#19737,#19738,#19739,#19740,#19741,#19742,#19743,#19744,#19745,#19746,#19747,
#19748,#19749,#19750,#19751,#19752,#19753,#19754,#19755,#19756,#19757,#19758),
 .UNSPECIFIED.,.F.,.F.,(4,2,2,2,2,2,2,2,2,2,2,2,2,2,2,2,2,2,4),(14.4220042621459,
14.4270670869734,14.502867746995,14.5772427049859,14.6499344470954,14.7263851908868,
14.7999071073808,14.8742276556564,14.9497200860508,15.0223907681477,15.0981506329107,
15.172688996992,15.2451496511092,15.320938380604,15.3946463929566,15.468320170018,
15.5440309579608,15.616894466422,15.6238544618538),.UNSPECIFIED.);
#885=B_SPLINE_CURVE_WITH_KNOTS('',3,(#19763,#19764,#19765,#19766,#19767,
#19768,#19769,#19770,#19771,#19772,#19773,#19774,#19775,#19776,#19777,#19778,
#19779,#19780,#19781,#19782,#19783,#19784,#19785,#19786,#19787,#19788,#19789,
#19790,#19791,#19792,#19793,#19794,#19795,#19796,#19797,#19798,#19799,#19800),
 .UNSPECIFIED.,.F.,.F.,(4,2,2,2,2,2,2,2,2,2,2,2,2,2,2,2,2,2,4),(5.49987666712128,
5.50936969912529,5.58230823770329,5.65810491492989,5.73154304558173,5.80532493915137,
5.8810855957766,5.95346927632274,6.02808199011211,6.10382388051154,6.17656308684462,
6.25213419297739,6.32614937751272,6.39973604327568,6.47626478262863,6.54882068220162,
6.62326404859892,6.6990181768668,6.70124289322726),.UNSPECIFIED.);
#886=B_SPLINE_CURVE_WITH_KNOTS('',3,(#19801,#19802,#19803,#19804,#19805,
#19806,#19807,#19808,#19809,#19810,#19811,#19812,#19813,#19814,#19815,#19816,
#19817,#19818,#19819,#19820,#19821,#19822,#19823,#19824,#19825,#19826,#19827,
#19828,#19829,#19830,#19831,#19832,#19833,#19834,#19835,#19836),
 .UNSPECIFIED.,.F.,.F.,(4,2,2,2,2,2,2,2,2,2,2,2,2,2,2,2,2,4),(15.6238544618538,
15.6932394001919,15.7679616847285,15.8403081894406,15.9160651326732,15.9899553136894,
16.0631834109938,16.1391016155685,16.2121483828073,16.2876906971423,16.362636948483,
16.4349759477711,16.5107227353739,16.584833013443,16.657704448787,16.7338677596132,
16.8071315434702,16.8249604142555),.UNSPECIFIED.);
#887=B_SPLINE_CURVE_WITH_KNOTS('',3,(#19841,#19842,#19843,#19844,#19845,
#19846,#19847,#19848,#19849,#19850,#19851,#19852,#19853,#19854,#19855,#19856,
#19857,#19858,#19859,#19860,#19861,#19862,#19863,#19864,#19865,#19866,#19867,
#19868,#19869,#19870,#19871,#19872,#19873,#19874,#19875,#19876),
 .UNSPECIFIED.,.F.,.F.,(4,2,2,2,2,2,2,2,2,2,2,2,2,2,2,2,2,4),(4.29888383168269,
4.31944357582395,4.39281336408965,4.46909712483566,4.54182615941889,4.61604528467895,
4.6917854903481,4.76415503769022,4.83921257243693,4.91438042167323,4.98751955350481,
5.06354298907082,5.13657441885952,5.21055783230592,5.28629707756517,5.35861581800472,
5.43343286402621,5.49987666712128),.UNSPECIFIED.);
#888=B_SPLINE_CURVE_WITH_KNOTS('',3,(#19877,#19878,#19879,#19880,#19881,
#19882,#19883,#19884,#19885,#19886,#19887,#19888,#19889,#19890,#19891,#19892,
#19893,#19894,#19895,#19896,#19897,#19898,#19899,#19900,#19901,#19902,#19903,
#19904,#19905,#19906,#19907,#19908,#19909,#19910,#19911,#19912),
 .UNSPECIFIED.,.F.,.F.,(4,2,2,2,2,2,2,2,2,2,2,2,2,2,2,2,2,4),(16.8249604142555,
16.8819522219098,16.9571540489601,17.0296070213112,17.1053670193323,17.1797272900657,
17.2523579029735,17.3287952776113,17.4023020941915,17.4765231421258,17.5520028504968,
17.6246597107687,17.7003851939233,17.7749103429322,17.8473232637256,17.9230754686744,
17.9967705304612,18.0262961697653),.UNSPECIFIED.);
#889=B_SPLINE_CURVE_WITH_KNOTS('',3,(#19917,#19918,#19919,#19920,#19921,
#19922,#19923,#19924,#19925,#19926,#19927,#19928,#19929,#19930,#19931,#19932,
#19933,#19934,#19935,#19936,#19937,#19938,#19939,#19940,#19941,#19942,#19943,
#19944,#19945,#19946,#19947,#19948,#19949,#19950,#19951,#19952),
 .UNSPECIFIED.,.F.,.F.,(4,2,2,2,2,2,2,2,2,2,2,2,2,2,2,2,2,4),(3.09726687965577,
3.1293327078715,3.20315237979801,3.27892867777479,3.35131868834466,3.42596958146837,
3.50172952178251,3.57450514884734,3.65011581516003,3.7240870698342,3.79770971006065,
3.87427831122171,3.94682778477419,4.02130828556258,4.09707395257375,4.16961694382427,
4.24494202381471,4.29888383168269),.UNSPECIFIED.);
#890=B_SPLINE_CURVE_WITH_KNOTS('',3,(#19953,#19954,#19955,#19956,#19957,
#19958,#19959,#19960,#19961,#19962,#19963,#19964,#19965,#19966,#19967,#19968,
#19969,#19970,#19971,#19972,#19973,#19974,#19975,#19976,#19977,#19978,#19979,
#19980,#19981,#19982,#19983,#19984,#19985,#19986,#19987,#19988),
 .UNSPECIFIED.,.F.,.F.,(4,2,2,2,2,2,2,2,2,2,2,2,2,2,2,2,2,4),(18.0262961697653,
18.0703605134091,18.14606029023,18.2189115217723,18.2951327104639,18.3698464948732,
18.4421559925931,18.51787876332,18.5917604656892,18.6649130484959,18.7408247221732,
18.8138632321234,18.8892887401014,18.9642303518526,19.0365453779641,19.1122604897676,
19.1863659359319,19.2269385903047),.UNSPECIFIED.);
#891=B_SPLINE_CURVE_WITH_KNOTS('',3,(#19993,#19994,#19995,#19996,#19997,
#19998,#19999,#20000,#20001,#20002,#20003,#20004,#20005,#20006,#20007,#20008,
#20009,#20010,#20011,#20012,#20013,#20014,#20015,#20016,#20017,#20018,#20019,
#20020,#20021,#20022,#20023,#20024,#20025,#20026,#20027,#20028),
 .UNSPECIFIED.,.F.,.F.,(4,2,2,2,2,2,2,2,2,2,2,2,2,2,2,2,2,4),(1.8959795055474,
1.9393592958045,2.01362339134596,2.08938397654367,2.16178410462566,2.23688741543728,
2.31199833731952,2.3851787149032,2.46124709092875,2.53425958502741,2.60828479791366,
2.6840419580893,2.75637837799298,2.83123784888653,2.90710918892568,2.98008539530125,
3.0559230158524,3.09726687965577),.UNSPECIFIED.);
#892=B_SPLINE_CURVE_WITH_KNOTS('',3,(#20029,#20030,#20031,#20032,#20033,
#20034,#20035,#20036,#20037,#20038,#20039,#20040,#20041,#20042,#20043,#20044,
#20045,#20046,#20047,#20048,#20049,#20050,#20051,#20052,#20053,#20054,#20055,
#20056,#20057,#20058,#20059,#20060,#20061,#20062,#20063,#20064),
 .UNSPECIFIED.,.F.,.F.,(4,2,2,2,2,2,2,2,2,2,2,2,2,2,2,2,2,4),(19.2269385903047,
19.2591738665856,19.3353342063483,19.4085929213386,19.4833088738998,19.558508885276,
19.6309515126468,19.7066825650131,19.7810406793351,19.853621686921,19.930058624413,
20.0035626708721,20.0776946111672,20.1531743178055,20.2258295252266,20.3015326258325,
20.3760570414271,20.4278890513381),.UNSPECIFIED.);
#893=B_SPLINE_CURVE_WITH_KNOTS('',3,(#20069,#20070,#20071,#20072,#20073,
#20074,#20075,#20076,#20077,#20078,#20079,#20080,#20081,#20082,#20083,#20084,
#20085,#20086,#20087,#20088,#20089,#20090,#20091,#20092,#20093,#20094,#20095,
#20096,#20097,#20098,#20099,#20100,#20101,#20102,#20103,#20104),
 .UNSPECIFIED.,.F.,.F.,(4,2,2,2,2,2,2,2,2,2,2,2,2,2,2,2,2,4),(0.693996851653457,
0.748401533499502,0.823100571323074,0.898889829797497,0.971711662205941,
1.04737197901952,1.12131453444175,1.19498314402497,1.27160189386835,1.34415795995857,
1.41868569673119,1.49447448163682,1.56706066862621,1.6424338957219,1.71689141144651,
1.79030520660482,1.86663698237822,1.8959795055474),.UNSPECIFIED.);
#894=B_SPLINE_CURVE_WITH_KNOTS('',3,(#20105,#20106,#20107,#20108,#20109,
#20110,#20111,#20112,#20113,#20114,#20115,#20116,#20117,#20118,#20119,#20120,
#20121,#20122,#20123,#20124,#20125,#20126,#20127,#20128,#20129,#20130,#20131,
#20132,#20133,#20134,#20135,#20136,#20137,#20138,#20139,#20140),
 .UNSPECIFIED.,.F.,.F.,(4,2,2,2,2,2,2,2,2,2,2,2,2,2,2,2,2,4),(20.4278890513381,
20.4484340912896,20.5241616208347,20.5978560559012,20.6713731521802,20.7470746205059,
20.8199257271634,20.8960333809615,20.9707512015188,21.0430361070662,21.1187366153993,
21.1926222126879,21.2657107641379,21.3416286508347,21.4146710898949,21.4899906638883,
21.5649401850703,21.6282084253952),.UNSPECIFIED.);
#895=B_SPLINE_CURVE_WITH_KNOTS('',3,(#20146,#20147,#20148,#20149,#20150,
#20151,#20152,#20153,#20154,#20155,#20156,#20157,#20158,#20159,#20160,#20161,
#20162,#20163,#20164,#20165,#20166,#20167,#20168,#20169,#20170,#20171,#20172,
#20173,#20174,#20175,#20176,#20177,#20178,#20179),.UNSPECIFIED.,.F.,.F.,
(4,2,2,2,2,2,2,2,2,2,2,2,2,2,2,2,4),(21.3998620379566,21.4010821380198,
21.4745419758515,21.5484483384161,21.6238885835661,21.6965022150209,21.7721179655765,
21.8466016752083,21.9188674724763,21.994502511453,22.0681568289235,22.1414834717519,
22.2171485887074,22.2899609285255,22.3657908963153,22.4066118716899,22.447261954037),
 .UNSPECIFIED.);
#896=B_SPLINE_CURVE_WITH_KNOTS('',3,(#20182,#20183,#20184,#20185,#20186,
#20187,#20188,#20189,#20190,#20191,#20192,#20193,#20194,#20195,#20196,#20197,
#20198,#20199,#20200,#20201,#20202,#20203,#20204,#20205,#20206,#20207,#20208,
#20209,#20210,#20211),.UNSPECIFIED.,.F.,.F.,(4,2,2,2,2,2,2,2,2,2,2,2,2,
2,4),(9.99999992557917E-7,0.0390553475424834,0.0794268420902697,0.155094300389673,
0.228753948163334,0.302420633338845,0.378175682123393,0.450609245608276,
0.525105867869494,0.600831277267472,0.673461628031261,0.748911544765981,
0.823223502985756,0.896705054014033,0.900735091737263),.UNSPECIFIED.);
#897=B_SPLINE_CURVE_WITH_KNOTS('',3,(#20216,#20217,#20218,#20219,#20220,
#20221,#20222,#20223,#20224,#20225,#20226,#20227,#20228,#20229,#20230,#20231,
#20232,#20233,#20234,#20235,#20236,#20237,#20238,#20239,#20240,#20241,#20242,
#20243,#20244,#20245,#20246,#20247,#20248,#20249,#20250,#20251),
 .UNSPECIFIED.,.F.,.F.,(4,2,2,2,2,2,2,2,2,2,2,2,2,2,2,2,2,4),(20.2007312380072,
20.2134304027239,20.286413815735,20.3615507327354,20.4364439593744,20.5086741450774,
20.5842817477222,20.6583387616512,20.7309759746707,20.8070907732301,20.8803008305636,
20.954756341213,21.0299135327095,21.1023004889085,21.1779300353889,21.2522450006783,
21.3246857908901,21.3998620379566),.UNSPECIFIED.);
#898=B_SPLINE_CURVE_WITH_KNOTS('',3,(#20252,#20253,#20254,#20255,#20256,
#20257,#20258,#20259,#20260,#20261,#20262,#20263,#20264,#20265,#20266,#20267,
#20268,#20269,#20270,#20271,#20272,#20273,#20274,#20275,#20276,#20277,#20278,
#20279,#20280,#20281,#20282,#20283,#20284,#20285,#20286,#20287),
 .UNSPECIFIED.,.F.,.F.,(4,2,2,2,2,2,2,2,2,2,2,2,2,2,2,2,2,4),(0.900735091737263,
0.973113026033783,1.0457827221505,1.12011671494025,1.19588534560907,1.26832549045455,
1.34350027467199,1.41843188079472,1.49167375924559,1.56781129900037,1.64073986869053,
1.7148276667715,1.79058665025377,1.86293090550078,1.93785412351329,2.01352224202086,
2.08655154961337,2.10211990279725),.UNSPECIFIED.);
#899=B_SPLINE_CURVE_WITH_KNOTS('',3,(#20292,#20293,#20294,#20295,#20296,
#20297,#20298,#20299,#20300,#20301,#20302,#20303,#20304,#20305,#20306,#20307,
#20308,#20309,#20310,#20311,#20312,#20313,#20314,#20315,#20316,#20317,#20318,
#20319,#20320,#20321,#20322,#20323,#20324,#20325,#20326,#20327),
 .UNSPECIFIED.,.F.,.F.,(4,2,2,2,2,2,2,2,2,2,2,2,2,2,2,2,2,4),(19.0017088956488,
19.026413597501,19.0990040972824,19.1746164405539,19.2490755302594,19.321350577979,
19.3969846493222,19.4706145700775,19.5439869692317,19.6196247612694,19.6924125917538,
19.768327665187,19.8429852098392,19.9151811574575,19.9907909406617,20.0646168007593,
20.1375714521606,20.2007312380072),.UNSPECIFIED.);
#900=B_SPLINE_CURVE_WITH_KNOTS('',3,(#20328,#20329,#20330,#20331,#20332,
#20333,#20334,#20335,#20336,#20337,#20338,#20339,#20340,#20341,#20342,#20343,
#20344,#20345,#20346,#20347,#20348,#20349,#20350,#20351,#20352,#20353,#20354,
#20355,#20356,#20357,#20358,#20359,#20360,#20361,#20362,#20363),
 .UNSPECIFIED.,.F.,.F.,(4,2,2,2,2,2,2,2,2,2,2,2,2,2,2,2,2,4),(2.10211990279725,
2.16244894936447,2.23574937496902,2.30962213376385,2.38539453398937,2.4577632128723,
2.53246781384893,2.60823013701643,2.68105622872575,2.75672375742662,2.83054621909795,
2.90421795092189,2.98002840864426,3.05254665410568,3.12704873372042,3.20280316035751,
3.27536365707667,3.30365799318677),.UNSPECIFIED.);
#901=B_SPLINE_CURVE_WITH_KNOTS('',3,(#20368,#20369,#20370,#20371,#20372,
#20373,#20374,#20375,#20376,#20377,#20378,#20379,#20380,#20381,#20382,#20383,
#20384,#20385,#20386,#20387,#20388,#20389,#20390,#20391,#20392,#20393,#20394,
#20395,#20396,#20397,#20398,#20399,#20400,#20401,#20402,#20403),
 .UNSPECIFIED.,.F.,.F.,(4,2,2,2,2,2,2,2,2,2,2,2,2,2,2,2,2,4),(17.8023401640365,
17.8389668145887,17.9111936616507,17.9868073571536,18.0608434695502,18.133517651016,
18.2096089813251,18.2827987686193,18.3573324455908,18.4324654961022,18.5048353047865,
18.5804680791381,18.6547595601668,18.7272229946283,18.8035934363314,18.8770308485898,
18.9509991493981,19.0017088956488),.UNSPECIFIED.);
#902=B_SPLINE_CURVE_WITH_KNOTS('',3,(#20404,#20405,#20406,#20407,#20408,
#20409,#20410,#20411,#20412,#20413,#20414,#20415,#20416,#20417,#20418,#20419,
#20420,#20421,#20422,#20423,#20424,#20425,#20426,#20427,#20428,#20429,#20430,
#20431,#20432,#20433,#20434,#20435,#20436,#20437,#20438,#20439),
 .UNSPECIFIED.,.F.,.F.,(4,2,2,2,2,2,2,2,2,2,2,2,2,2,2,2,2,4),(3.30365799318677,
3.35071106186011,3.42511288438873,3.49850057876448,3.57480597153522,3.64748593997752,
3.72172379123405,3.7974491155508,3.86981948936067,3.94489636093728,4.01994685668824,
4.09310036383744,4.16914150257682,4.24210737920037,4.31610544665387,4.39182652214827,
4.46412891541083,4.50446478944951),.UNSPECIFIED.);
#903=B_SPLINE_CURVE_WITH_KNOTS('',3,(#20444,#20445,#20446,#20447,#20448,
#20449,#20450,#20451,#20452,#20453,#20454,#20455,#20456,#20457,#20458,#20459,
#20460,#20461,#20462,#20463,#20464,#20465,#20466,#20467,#20468,#20469,#20470,
#20471,#20472,#20473,#20474,#20475,#20476,#20477,#20478,#20479),
 .UNSPECIFIED.,.F.,.F.,(4,2,2,2,2,2,2,2,2,2,2,2,2,2,2,2,2,4),(16.6032707324218,
16.6513817973194,16.723678768177,16.7993239524381,16.8729409992827,16.9463724810034,
17.0219947252625,17.094769384138,17.170783948967,17.2454238472081,17.3176301069999,
17.3932485807392,17.4670571110006,17.5400615604984,17.6159005169778,17.6888667744311,
17.7640950147645,17.8023401640365),.UNSPECIFIED.);
#904=B_SPLINE_CURVE_WITH_KNOTS('',3,(#20480,#20481,#20482,#20483,#20484,
#20485,#20486,#20487,#20488,#20489,#20490,#20491,#20492,#20493,#20494,#20495,
#20496,#20497,#20498,#20499,#20500,#20501,#20502,#20503,#20504,#20505,#20506,
#20507,#20508,#20509,#20510,#20511,#20512,#20513,#20514,#20515),
 .UNSPECIFIED.,.F.,.F.,(4,2,2,2,2,2,2,2,2,2,2,2,2,2,2,2,2,4),(4.50446478944951,
4.53896099017265,4.61476851462214,4.68771679150871,4.76352599294146,4.83688560323665,
4.91067692380354,4.98641636639118,5.05876849076569,5.13339070946845,5.20911462118278,
5.28186203260248,5.35744396510543,5.43135962875759,5.5049534453086,5.58149289583282,
5.65400014953507,5.70546524065298),.UNSPECIFIED.);
#905=B_SPLINE_CURVE_WITH_KNOTS('',3,(#20520,#20521,#20522,#20523,#20524,
#20525,#20526,#20527,#20528,#20529,#20530,#20531,#20532,#20533,#20534,#20535,
#20536,#20537,#20538,#20539,#20540,#20541,#20542,#20543,#20544,#20545,#20546,
#20547,#20548,#20549,#20550,#20551,#20552,#20553,#20554,#20555),
 .UNSPECIFIED.,.F.,.F.,(4,2,2,2,2,2,2,2,2,2,2,2,2,2,2,2,2,4),(15.4036127818561,
15.4629837689097,15.5357079153789,15.6117880203978,15.68496929525,15.7595946060973,
15.8347155210961,15.9070810189327,15.9827292214831,16.0570090817769,16.1295081903979,
16.2058648944736,16.2792915083073,16.3533352798644,16.4287358039088,16.501314596555,
16.5769356517096,16.6032707324218),.UNSPECIFIED.);
#906=B_SPLINE_CURVE_WITH_KNOTS('',3,(#20556,#20557,#20558,#20559,#20560,
#20561,#20562,#20563,#20564,#20565,#20566,#20567,#20568,#20569,#20570,#20571,
#20572,#20573,#20574,#20575,#20576,#20577,#20578,#20579,#20580,#20581,#20582,
#20583,#20584,#20585,#20586,#20587,#20588,#20589,#20590,#20591),
 .UNSPECIFIED.,.F.,.F.,(4,2,2,2,2,2,2,2,2,2,2,2,2,2,2,2,2,4),(5.70546524065298,
5.72845174646461,5.80417918889931,5.87669291399989,5.95198889447905,6.02642912834167,
6.099769545299,6.17602356503088,6.24870556733163,6.32289513760141,6.39859617033174,
6.47093208541315,6.54595983515997,6.62106144576296,6.69417036178633,6.77016311771506,
6.8431430391509,6.90599013816734),.UNSPECIFIED.);
#907=B_SPLINE_CURVE_WITH_KNOTS('',3,(#20596,#20597,#20598,#20599,#20600,
#20601,#20602,#20603,#20604,#20605,#20606,#20607,#20608,#20609,#20610,#20611,
#20612,#20613,#20614,#20615,#20616,#20617,#20618,#20619,#20620,#20621,#20622,
#20623,#20624,#20625,#20626,#20627,#20628,#20629,#20630,#20631),
 .UNSPECIFIED.,.F.,.F.,(4,2,2,2,2,2,2,2,2,2,2,2,2,2,2,2,2,4),(14.2043028097508,
14.2747055373133,14.3482084709696,14.4238275610328,14.4966009415762,14.5727275919946,
14.6473620165199,14.7195913711808,14.795230680713,14.8690338970156,14.9421008958382,
15.0179321830715,15.0908931142881,15.1662257781497,15.2410882395189,15.3133246655807,
15.3889566201665,15.4036127818561),.UNSPECIFIED.);
#908=B_SPLINE_CURVE_WITH_KNOTS('',3,(#20632,#20633,#20634,#20635,#20636,
#20637,#20638,#20639,#20640,#20641,#20642,#20643,#20644,#20645,#20646,#20647,
#20648,#20649,#20650,#20651,#20652,#20653,#20654,#20655,#20656,#20657,#20658,
#20659,#20660,#20661,#20662,#20663,#20664,#20665,#20666,#20667,#20668,#20669),
 .UNSPECIFIED.,.F.,.F.,(4,2,2,2,2,2,2,2,2,2,2,2,2,2,2,2,2,2,4),(6.90599013816734,
6.91709591054206,6.99279511544632,7.06507570458308,7.13986191697079,7.21572907571421,
7.28863624774249,7.36440096151241,7.43778401952338,7.51153406441721,7.58725386603195,
7.65959537324807,7.73417586888514,7.80987775822848,7.88258527044843,7.95812405247512,
8.03207835995344,8.10563264968525,8.10649808593899),.UNSPECIFIED.);
#909=B_SPLINE_CURVE_WITH_KNOTS('',3,(#20674,#20675,#20676,#20677,#20678,
#20679,#20680,#20681,#20682,#20683,#20684,#20685,#20686,#20687,#20688,#20689,
#20690,#20691,#20692,#20693,#20694,#20695,#20696,#20697,#20698,#20699,#20700,
#20701,#20702,#20703,#20704,#20705,#20706,#20707,#20708,#20709,#20710,#20711),
 .UNSPECIFIED.,.F.,.F.,(4,2,2,2,2,2,2,2,2,2,2,2,2,2,2,2,2,2,4),(13.0043185145707,
13.0131961618393,13.0863810742337,13.1611097586802,13.2362310180851,13.3086053228822,
13.3842810516299,13.4585616154906,13.5311088763717,13.6074645223847,13.6808924755368,
13.7550239419564,13.8304229984377,13.9030020346595,13.9786440351523,14.0530894710899,
14.1254208536733,14.2010892882464,14.2043028097508),.UNSPECIFIED.);
#910=B_SPLINE_CURVE_WITH_KNOTS('',3,(#20712,#20713,#20714,#20715,#20716,
#20717,#20718,#20719,#20720,#20721,#20722,#20723,#20724,#20725,#20726,#20727,
#20728,#20729,#20730,#20731,#20732,#20733,#20734,#20735,#20736,#20737,#20738,
#20739,#20740,#20741,#20742,#20743,#20744,#20745,#20746,#20747),
 .UNSPECIFIED.,.F.,.F.,(4,2,2,2,2,2,2,2,2,2,2,2,2,2,2,2,2,4),(8.10649808593899,
8.18212857782179,8.25463769233127,8.32904856291924,8.40476039560251,8.47723808436404,
8.55249249244931,8.6269871616477,8.70029010543794,8.77650284076587,8.84920045806996,
8.92335167723176,8.99903990378592,9.07135287698761,9.14634154317815,9.22151071619755,
9.29458504609435,9.30692725994904),.UNSPECIFIED.);
#911=B_SPLINE_CURVE_WITH_KNOTS('',3,(#20752,#20753,#20754,#20755,#20756,
#20757,#20758,#20759,#20760,#20761,#20762,#20763,#20764,#20765,#20766,#20767,
#20768,#20769,#20770,#20771,#20772,#20773,#20774,#20775,#20776,#20777,#20778,
#20779,#20780,#20781,#20782,#20783,#20784,#20785,#20786,#20787),
 .UNSPECIFIED.,.F.,.F.,(4,2,2,2,2,2,2,2,2,2,2,2,2,2,2,2,2,4),(11.8045357693031,
11.8246955167202,11.8974797480381,11.973728941363,12.048370394829,12.1206353038175,
12.1963073859733,12.2701176287412,12.3432587958549,12.4190951183632,12.4920628764287,
12.5675110699007,12.6423766978021,12.714635590817,12.7902978126314,12.8643283394953,
12.9371145822676,13.0043185145707),.UNSPECIFIED.);
#912=B_SPLINE_CURVE_WITH_KNOTS('',3,(#20788,#20789,#20790,#20791,#20792,
#20793,#20794,#20795,#20796,#20797,#20798,#20799,#20800,#20801,#20802,#20803,
#20804,#20805,#20806,#20807,#20808,#20809,#20810,#20811,#20812,#20813,#20814,
#20815,#20816,#20817,#20818,#20819,#20820,#20821,#20822,#20823),
 .UNSPECIFIED.,.F.,.F.,(4,2,2,2,2,2,2,2,2,2,2,2,2,2,2,2,2,4),(9.30692725994904,
9.37053973428254,9.4435477643714,9.51746559946554,9.59315452652494,9.66542543740846,
9.74017607133259,9.81611935995928,9.88899567467958,9.96472648537345,10.0381472533,
10.1118664472855,10.1875783107606,10.2599216974399,10.3344710332621,10.4101625475177,
10.4828405221781,10.507197202247),.UNSPECIFIED.);
#913=B_SPLINE_CURVE_WITH_KNOTS('',3,(#20828,#20829,#20830,#20831,#20832,
#20833,#20834,#20835,#20836,#20837,#20838,#20839,#20840,#20841,#20842,#20843,
#20844,#20845,#20846,#20847,#20848,#20849,#20850,#20851,#20852,#20853,#20854,
#20855,#20856,#20857,#20858,#20859,#20860,#20861,#20862,#20863),
 .UNSPECIFIED.,.F.,.F.,(4,2,2,2,2,2,2,2,2,2,2,2,2,2,2,2,2,4),(10.6039329181875,
10.6363651346832,10.7124501879071,10.7853405670855,10.8610838827621,10.934599898383,
11.008333799212,11.0840882660137,11.156484544635,11.2310488243127,11.3036402546897,
11.3793152266208,11.4537724131331,11.5261501395238,11.6018537056525,11.6754814591988,
11.7490669060118,11.8045357693031),.UNSPECIFIED.);
#914=B_SPLINE_CURVE_WITH_KNOTS('',3,(#20864,#20865,#20866,#20867,#20868,
#20869,#20870,#20871,#20872,#20873,#20874,#20875,#20876,#20877,#20878,#20879,
#20880,#20881,#20882,#20883,#20884,#20885,#20886,#20887,#20888,#20889,#20890,
#20891,#20892,#20893,#20894,#20895,#20896,#20897,#20898,#20899),
 .UNSPECIFIED.,.F.,.F.,(4,2,2,2,2,2,2,2,2,2,2,2,2,2,2,2,2,4),(10.507197202247,
10.5583468648772,10.6323548055098,10.7058801425724,10.7823434678229,10.8548676450864,
10.929248488786,11.004956589598,11.0774099932164,11.1526336429167,11.2271981730393,
11.3029101516168,11.3766290823305,11.4500507067516,11.5257812108603,11.5986572591126,
11.6746020373567,11.7077777116762),.UNSPECIFIED.);
#915=B_SPLINE_CURVE_WITH_KNOTS('',3,(#20904,#20905,#20906,#20907,#20908,
#20909,#20910,#20911,#20912,#20913,#20914,#20915,#20916,#20917,#20918,#20919,
#20920,#20921,#20922,#20923,#20924,#20925,#20926,#20927,#20928,#20929,#20930,
#20931,#20932,#20933,#20934,#20935,#20936,#20937,#20938,#20939),
 .UNSPECIFIED.,.F.,.F.,(4,2,2,2,2,2,2,2,2,2,2,2,2,2,2,2,2,4),(9.40314292363424,
9.44807926432923,9.52269054080882,9.59599985679214,9.67221651690302,9.74498383159651,
9.81914102601776,9.8948661844282,9.96720341425604,10.0421977895991,10.1174988854888,
10.1905829359148,10.2665452811273,10.3396376931852,10.413565359407,10.4892941509423,
10.5616047072099,10.6039329181875),.UNSPECIFIED.);
#916=B_SPLINE_CURVE_WITH_KNOTS('',3,(#20940,#20941,#20942,#20943,#20944,
#20945,#20946,#20947,#20948,#20949,#20950,#20951,#20952,#20953,#20954,#20955,
#20956,#20957,#20958,#20959,#20960,#20961,#20962,#20963,#20964,#20965,#20966,
#20967,#20968,#20969,#20970,#20971,#20972,#20973,#20974,#20975),
 .UNSPECIFIED.,.F.,.F.,(4,2,2,2,2,2,2,2,2,2,2,2,2,2,2,2,2,4),(11.7077777116762,
11.7493523337136,11.8216233292765,11.8973123329413,11.9712298364502,12.0442385684753,
12.1201928820956,12.1932668846388,12.2684374097942,12.3434256811156,12.4157385236044,
12.4914267857389,12.5655776191594,12.6382757357031,12.7144880439345,12.7877906132398,
12.8622864217306,12.9079875737808),.UNSPECIFIED.);
#917=B_SPLINE_CURVE_WITH_KNOTS('',3,(#20980,#20981,#20982,#20983,#20984,
#20985,#20986,#20987,#20988,#20989,#20990,#20991,#20992,#20993,#20994,#20995,
#20996,#20997,#20998,#20999,#21000,#21001,#21002,#21003,#21004,#21005,#21006,
#21007,#21008,#21009,#21010,#21011,#21012,#21013,#21014,#21015),
 .UNSPECIFIED.,.F.,.F.,(4,2,2,2,2,2,2,2,2,2,2,2,2,2,2,2,2,4),(8.20191590591913,
8.25960106122842,8.33306373764413,8.40681574654923,8.48256448506601,8.55494444504399,
8.62952697206071,8.70525502991575,8.77796547717747,8.85350532364393,8.92755759145257,
9.00111590817091,9.07761319994366,9.15017581215132,9.22458992342226,9.30033545956258,
9.37282202157872,9.40314292363424),.UNSPECIFIED.);
#918=B_SPLINE_CURVE_WITH_KNOTS('',3,(#21016,#21017,#21018,#21019,#21020,
#21021,#21022,#21023,#21024,#21025,#21026,#21027,#21028,#21029,#21030,#21031,
#21032,#21033,#21034,#21035,#21036,#21037,#21038,#21039,#21040,#21041,#21042,
#21043,#21044,#21045,#21046,#21047,#21048,#21049,#21050,#21051),
 .UNSPECIFIED.,.F.,.F.,(4,2,2,2,2,2,2,2,2,2,2,2,2,2,2,2,2,4),(12.9079875737808,
12.937540394313,13.0100177383184,13.0857295612112,13.1601400073282,13.2326493964309,
13.309144861033,13.3826987428871,13.4566539318281,13.5321922527912,13.6048993478474,
13.6806011226957,13.7551811771442,13.8275227529135,13.9032424787233,13.976992086904,
14.0503757757738,14.1087366371979),.UNSPECIFIED.);
#919=B_SPLINE_CURVE_WITH_KNOTS('',3,(#21056,#21057,#21058,#21059,#21060,
#21061,#21062,#21063,#21064,#21065,#21066,#21067,#21068,#21069,#21070,#21071,
#21072,#21073,#21074,#21075,#21076,#21077,#21078,#21079,#21080,#21081,#21082,
#21083,#21084,#21085,#21086,#21087,#21088,#21089,#21090,#21091),
 .UNSPECIFIED.,.F.,.F.,(4,2,2,2,2,2,2,2,2,2,2,2,2,2,2,2,2,4),(7.00118688689761,
7.07080206795146,7.14353831016436,7.21772153799166,7.29344597627649,7.36579219781796,
7.44081319493958,7.51602919589249,7.58913550527881,7.66512315080874,7.73817162506754,
7.81212180542193,7.88784728261179,7.96015319704089,8.03493652227658,8.11092813520778,
8.18383683814882,8.20191590591913),.UNSPECIFIED.);
#920=B_SPLINE_CURVE_WITH_KNOTS('',3,(#21092,#21093,#21094,#21095,#21096,
#21097,#21098,#21099,#21100,#21101,#21102,#21103,#21104,#21105,#21106,#21107,
#21108,#21109,#21110,#21111,#21112,#21113,#21114,#21115,#21116,#21117,#21118,
#21119,#21120,#21121,#21122,#21123,#21124,#21125,#21126,#21127),
 .UNSPECIFIED.,.F.,.F.,(4,2,2,2,2,2,2,2,2,2,2,2,2,2,2,2,2,4),(14.1087366371979,
14.1261400064869,14.1990467415146,14.274915133928,14.3497008369486,14.4219813121166,
14.497680404552,14.5716327746707,14.6446131737348,14.7206053824683,14.7937138040713,
14.8688165097389,14.9438436963948,15.016179289806,15.0918801703987,15.1660691885856,
15.2387514714241,15.3090799178937),.UNSPECIFIED.);
#921=B_SPLINE_CURVE_WITH_KNOTS('',3,(#21132,#21133,#21134,#21135,#21136,
#21137,#21138,#21139,#21140,#21141,#21142,#21143,#21144,#21145,#21146,#21147,
#21148,#21149,#21150,#21151,#21152,#21153,#21154,#21155,#21156,#21157,#21158,
#21159,#21160,#21161,#21162,#21163,#21164,#21165,#21166,#21167,#21168,#21169),
 .UNSPECIFIED.,.F.,.F.,(4,2,2,2,2,2,2,2,2,2,2,2,2,2,2,2,2,2,4),(5.79993999134698,
5.80524971510209,5.88100482499339,5.95338123541158,6.02799348446614,6.10373035479458,
6.17646893000621,6.2520397566395,6.32603643947841,6.39962227107694,6.4761506781555,
6.54869647616329,6.62313915849589,6.69888684027576,6.77139608977099,6.84668261898845,
6.9212220444047,6.99455668680605,7.00118688689761),.UNSPECIFIED.);
#922=B_SPLINE_CURVE_WITH_KNOTS('',3,(#21170,#21171,#21172,#21173,#21174,
#21175,#21176,#21177,#21178,#21179,#21180,#21181,#21182,#21183,#21184,#21185,
#21186,#21187,#21188,#21189,#21190,#21191,#21192,#21193,#21194,#21195,#21196,
#21197,#21198,#21199,#21200,#21201,#21202,#21203,#21204,#21205,#21206,#21207),
 .UNSPECIFIED.,.F.,.F.,(4,2,2,2,2,2,2,2,2,2,2,2,2,2,2,2,2,2,4),(15.3090799178937,
15.3150048947458,15.3883447730857,15.4627858935473,15.5380812730832,15.6105944732051,
15.6863217194936,15.7607727281917,15.8332800474004,15.9098188675437,15.983412114232,
16.0573284163402,16.1329097241255,16.2056565597743,16.2813801753304,16.3560017912743,
16.4283537881353,16.5040929719216,16.5100414867088),.UNSPECIFIED.);
#923=B_SPLINE_CURVE_WITH_KNOTS('',3,(#21212,#21213,#21214,#21215,#21216,
#21217,#21218,#21219,#21220,#21221,#21222,#21223,#21224,#21225,#21226,#21227,
#21228,#21229,#21230,#21231,#21232,#21233,#21234,#21235,#21236,#21237,#21238,
#21239,#21240,#21241,#21242,#21243,#21244,#21245,#21246,#21247),
 .UNSPECIFIED.,.F.,.F.,(4,2,2,2,2,2,2,2,2,2,2,2,2,2,2,2,2,4),(4.5990670002631,
4.61605684680242,4.69179254909771,4.76416014599027,4.83921885367157,4.91436515169427,
4.98750468221458,5.06352898580182,5.13654749103522,5.21053132121442,5.28626552208576,
5.35857948073502,5.43339698071682,5.5093103302291,5.58224849564028,5.65804517900355,
5.73146827412131,5.79993999134698),.UNSPECIFIED.);
#924=B_SPLINE_CURVE_WITH_KNOTS('',3,(#21248,#21249,#21250,#21251,#21252,
#21253,#21254,#21255,#21256,#21257,#21258,#21259,#21260,#21261,#21262,#21263,
#21264,#21265,#21266,#21267,#21268,#21269,#21270,#21271,#21272,#21273,#21274,
#21275,#21276,#21277,#21278,#21279,#21280,#21281,#21282,#21283),
 .UNSPECIFIED.,.F.,.F.,(4,2,2,2,2,2,2,2,2,2,2,2,2,2,2,2,2,4),(16.5100414867088,
16.5778836963156,16.6512437083802,16.7270522652006,16.7999999483695,16.875808436759,
16.9506398455013,17.0229419365147,17.0986627186034,17.1726601299846,17.2456262600853,
17.3216666947875,17.3948195550358,17.4698708787336,17.5449470347907,17.6173169102686,
17.6930419035619,17.7107202775431),.UNSPECIFIED.);
#925=B_SPLINE_CURVE_WITH_KNOTS('',3,(#21288,#21289,#21290,#21291,#21292,
#21293,#21294,#21295,#21296,#21297,#21298,#21299,#21300,#21301,#21302,#21303,
#21304,#21305,#21306,#21307,#21308,#21309,#21310,#21311,#21312,#21313,#21314,
#21315,#21316,#21317,#21318,#21319,#21320,#21321,#21322,#21323),
 .UNSPECIFIED.,.F.,.F.,(4,2,2,2,2,2,2,2,2,2,2,2,2,2,2,2,2,4),(3.3975365581224,
3.42602438710494,3.5017817905074,3.57455897160418,3.65017161489103,3.7241276379769,
3.79775167506893,3.87432224447071,3.94686445750292,4.02134653058967,4.09710829208354,
4.16965210409428,4.24497885654866,4.31946174601459,4.39283252180053,4.46911780612146,
4.54183662559879,4.5990670002631),.UNSPECIFIED.);
#926=B_SPLINE_CURVE_WITH_KNOTS('',3,(#21324,#21325,#21326,#21327,#21328,
#21329,#21330,#21331,#21332,#21333,#21334,#21335,#21336,#21337,#21338,#21339,
#21340,#21341,#21342,#21343,#21344,#21345,#21346,#21347,#21348,#21349,#21350,
#21351,#21352,#21353,#21354,#21355,#21356,#21357,#21358,#21359),
 .UNSPECIFIED.,.F.,.F.,(4,2,2,2,2,2,2,2,2,2,2,2,2,2,2,2,2,4),(17.7107202775431,
17.7672790518916,17.8399590864096,17.9162637298069,17.9896507365271,18.0640531875706,
18.1393998421222,18.2119596512683,18.2877137050319,18.3622150485036,18.434733158509,
18.5105432221001,18.5842142230993,18.658037094598,18.7337038356029,18.8065291945043,
18.8822910488291,18.9121502857923),.UNSPECIFIED.);
#927=B_SPLINE_CURVE_WITH_KNOTS('',3,(#21364,#21365,#21366,#21367,#21368,
#21369,#21370,#21371,#21372,#21373,#21374,#21375,#21376,#21377,#21378,#21379,
#21380,#21381,#21382,#21383,#21384,#21385,#21386,#21387,#21388,#21389,#21390,
#21391,#21392,#21393,#21394,#21395,#21396,#21397,#21398,#21399),
 .UNSPECIFIED.,.F.,.F.,(4,2,2,2,2,2,2,2,2,2,2,2,2,2,2,2,2,4),(2.19630130324308,
2.23699605736667,2.31208902084933,2.38527190148058,2.46134331220889,2.53434591982495,
2.60837368609728,2.68412827430948,2.75646249211865,2.83132457944634,2.90717605118273,
2.98015404422193,3.05599389927964,3.12939165042261,3.20321306725771,3.27898631713552,
3.3513717320634,3.3975365581224),.UNSPECIFIED.);
#928=B_SPLINE_CURVE_WITH_KNOTS('',3,(#21400,#21401,#21402,#21403,#21404,
#21405,#21406,#21407,#21408,#21409,#21410,#21411,#21412,#21413,#21414,#21415,
#21416,#21417,#21418,#21419,#21420,#21421,#21422,#21423,#21424,#21425,#21426,
#21427,#21428,#21429,#21430,#21431,#21432,#21433,#21434,#21435),
 .UNSPECIFIED.,.F.,.F.,(4,2,2,2,2,2,2,2,2,2,2,2,2,2,2,2,2,4),(18.9121502857923,
18.9569948872441,19.029363239932,19.1051352086863,19.1790072138826,19.2523078208173,
19.3282044162291,19.4012329759683,19.4769018075669,19.5518242052145,19.6241679619349,
19.6999264806165,19.774013470379,19.8469420709271,19.9230787522869,19.996319834517,
20.071252010965,20.1134543703229),.UNSPECIFIED.);
#929=B_SPLINE_CURVE_WITH_KNOTS('',3,(#21440,#21441,#21442,#21443,#21444,
#21445,#21446,#21447,#21448,#21449,#21450,#21451,#21452,#21453,#21454,#21455,
#21456,#21457,#21458,#21459,#21460,#21461,#21462,#21463,#21464,#21465,#21466,
#21467,#21468,#21469,#21470,#21471,#21472,#21473,#21474,#21475),
 .UNSPECIFIED.,.F.,.F.,(4,2,2,2,2,2,2,2,2,2,2,2,2,2,2,2,2,4),(0.994462254792754,
1.04749156011108,1.12142218453664,1.19509421741773,1.27171701403914,1.34426856529834,
1.41879991994479,1.49458721880891,1.56717647764929,1.64255344225318,1.71699577898508,
1.7904126205899,1.86674803540827,1.93946305186304,2.01373032787344,2.08948885623164,
2.16188946682002,2.19630130324308),.UNSPECIFIED.);
#930=B_SPLINE_CURVE_WITH_KNOTS('',3,(#21476,#21477,#21478,#21479,#21480,
#21481,#21482,#21483,#21484,#21485,#21486,#21487,#21488,#21489,#21490,#21491,
#21492,#21493,#21494,#21495,#21496,#21497,#21498,#21499,#21500,#21501,#21502,
#21503,#21504,#21505,#21506,#21507,#21508,#21509,#21510,#21511),
 .UNSPECIFIED.,.F.,.F.,(4,2,2,2,2,2,2,2,2,2,2,2,2,2,2,2,2,4),(20.1134543703229,
20.1464259304583,20.2188653895587,20.2946335188956,20.3689666613071,20.4416362056508,
20.51804328322,20.5915240830594,20.665836496343,20.7412856015319,20.8139151933508,
20.8896400971914,20.9641359268394,21.0365692298324,21.1123238022716,21.1859897017057,
21.2596495896079,21.3148424617523),.UNSPECIFIED.);
#931=B_SPLINE_CURVE_WITH_KNOTS('',3,(#21518,#21519,#21520,#21521,#21522,
#21523,#21524,#21525,#21526,#21527,#21528,#21529,#21530,#21531),
 .UNSPECIFIED.,.F.,.F.,(4,2,2,2,2,2,4),(9.99999998850988E-7,0.0516169518680174,
0.104845041291632,0.181709819458214,0.255107103717481,0.330970348449006,
0.40012180130331),.UNSPECIFIED.);
#932=B_SPLINE_CURVE_WITH_KNOTS('',3,(#21537,#21538,#21539,#21540,#21541,
#21542,#21543,#21544,#21545,#21546,#21547,#21548,#21549,#21550,#21551,#21552),
 .UNSPECIFIED.,.F.,.F.,(4,2,2,2,2,2,2,4),(7.19320368172551,7.22969104326796,
7.30685234317664,7.3810857236285,7.45736679269846,7.53354842516138,7.60230579027905,
7.67143903153145),.UNSPECIFIED.);
#933=B_SPLINE_CURVE_WITH_KNOTS('',3,(#21554,#21555,#21556,#21557,#21558,
#21559,#21560,#21561,#21562,#21563,#21564,#21565,#21566,#21567,#21568,#21569,
#21570,#21571,#21572,#21573,#21574,#21575,#21576,#21577,#21578,#21579,#21580,
#21581,#21582,#21583,#21584,#21585,#21586,#21587,#21588,#21589,#21590,#21591),
 .UNSPECIFIED.,.F.,.F.,(4,2,2,2,2,2,2,2,2,2,2,2,2,2,2,2,2,2,4),(0.40012180130331,
0.408263585102685,0.48223140566233,0.559093024369444,0.633749160630985,
0.7085728423697,0.785465068742682,0.858957556763468,0.934624119514201,1.0114910968397,
1.08525873800664,1.16189369275507,1.23717718819415,1.31180620569013,1.38941296914438,
1.46311419611182,1.53861020423359,1.61550600313119,1.61947369254408),
 .UNSPECIFIED.);
#934=B_SPLINE_CURVE_WITH_KNOTS('',3,(#21596,#21597,#21598,#21599,#21600,
#21601,#21602,#21603,#21604,#21605,#21606,#21607,#21608,#21609,#21610,#21611,
#21612,#21613,#21614,#21615,#21616,#21617,#21618,#21619,#21620,#21621,#21622,
#21623,#21624,#21625,#21626,#21627,#21628,#21629,#21630,#21631),
 .UNSPECIFIED.,.F.,.F.,(4,2,2,2,2,2,2,2,2,2,2,2,2,2,2,2,2,4),(5.97412374915921,
6.02336400908153,6.10006341983446,6.17388859911262,6.25076071689292,6.32648861381787,
6.39995163611774,6.47684257850208,6.55172701295907,6.62625691294416,6.70318696736095,
6.77721590254118,6.85427849813963,6.93021529133003,7.0036137704599,7.08048358099157,
7.15557375602929,7.19320368172551),.UNSPECIFIED.);
#935=B_SPLINE_CURVE_WITH_KNOTS('',3,(#21632,#21633,#21634,#21635,#21636,
#21637,#21638,#21639,#21640,#21641,#21642,#21643,#21644,#21645,#21646,#21647,
#21648,#21649,#21650,#21651,#21652,#21653,#21654,#21655,#21656,#21657,#21658,
#21659,#21660,#21661,#21662,#21663,#21664,#21665,#21666,#21667),
 .UNSPECIFIED.,.F.,.F.,(4,2,2,2,2,2,2,2,2,2,2,2,2,2,2,2,2,4),(1.61947369254408,
1.68905949729837,1.76541133090778,1.84129353055796,1.91567439290728,1.99300112987828,
2.06693716068424,2.14217746504849,2.21905840786482,2.29248563659418,2.36857555377319,
2.44518301605857,2.51934077538404,2.59641539895315,2.67070516811205,2.74571872212431,
2.82260805308708,2.83860378589876),.UNSPECIFIED.);
#936=B_SPLINE_CURVE_WITH_KNOTS('',3,(#21672,#21673,#21674,#21675,#21676,
#21677,#21678,#21679,#21680,#21681,#21682,#21683,#21684,#21685,#21686,#21687,
#21688,#21689,#21690,#21691,#21692,#21693,#21694,#21695,#21696,#21697,#21698,
#21699,#21700,#21701,#21702,#21703,#21704,#21705,#21706,#21707),
 .UNSPECIFIED.,.F.,.F.,(4,2,2,2,2,2,2,2,2,2,2,2,2,2,2,2,2,4),(4.75497373082595,
4.81676779439483,4.89291059092831,4.96634139895796,5.04320276423669,5.11849451622994,
5.19232799860222,5.26971286679952,5.34414356990701,5.41981447495191,5.49622630207658,
5.56981970532191,5.6467031993106,5.72225738249546,5.79589351190913,5.87356474205255,
5.94824936086062,5.97412374915921),.UNSPECIFIED.);
#937=B_SPLINE_CURVE_WITH_KNOTS('',3,(#21708,#21709,#21710,#21711,#21712,
#21713,#21714,#21715,#21716,#21717,#21718,#21719,#21720,#21721,#21722,#21723,
#21724,#21725,#21726,#21727,#21728,#21729,#21730,#21731,#21732,#21733,#21734,
#21735,#21736,#21737,#21738,#21739,#21740,#21741,#21742,#21743),
 .UNSPECIFIED.,.F.,.F.,(4,2,2,2,2,2,2,2,2,2,2,2,2,2,2,2,2,4),(2.83860378589876,
2.89603271526497,2.97189145574824,3.04931019004864,3.12327790223017,3.20013738661533,
3.27487393439905,3.34969805164721,3.42661722293439,3.50014925659483,3.57581635011919,
3.65270773672471,3.72647689856381,3.80311152982859,3.87849324951609,3.95312500868852,
4.03073191878357,4.05823923276311),.UNSPECIFIED.);
#938=B_SPLINE_CURVE_WITH_KNOTS('',3,(#21748,#21749,#21750,#21751,#21752,
#21753,#21754,#21755,#21756,#21757,#21758,#21759,#21760,#21761,#21762,#21763,
#21764,#21765,#21766,#21767,#21768,#21769,#21770,#21771,#21772,#21773,#21774,
#21775,#21776,#21777,#21778,#21779,#21780,#21781,#21782,#21783),
 .UNSPECIFIED.,.F.,.F.,(4,2,2,2,2,2,2,2,2,2,2,2,2,2,2,2,2,4),(3.53614671007338,
3.60978705097125,3.68629180592067,3.76172365012633,3.83623446884164,3.91108901947874,
3.98566617435956,4.06256304463242,4.13656203704878,4.21371517669569,4.289616859908,
4.36300950126705,4.43987265648916,4.51492830685511,4.58908233354689,4.6662059935342,
4.74040545873923,4.75497373082595),.UNSPECIFIED.);
#939=B_SPLINE_CURVE_WITH_KNOTS('',3,(#21784,#21785,#21786,#21787,#21788,
#21789,#21790,#21791,#21792,#21793,#21794,#21795,#21796,#21797,#21798,#21799,
#21800,#21801,#21802,#21803,#21804,#21805,#21806,#21807,#21808,#21809,#21810,
#21811,#21812,#21813,#21814,#21815,#21816,#21817,#21818,#21819),
 .UNSPECIFIED.,.F.,.F.,(4,2,2,2,2,2,2,2,2,2,2,2,2,2,2,2,2,4),(4.05823923276311,
4.10448780523323,4.17998586227126,4.25691320464737,4.33047807862384,4.40683152944232,
4.48029143252306,4.5572212291454,4.63229802958326,4.70658708030576,4.78372874807228,
4.8579491025357,4.93451870778849,5.01067645232983,5.08415139575935,5.1610751136448,
5.23638220426729,5.27807262241528),.UNSPECIFIED.);
#940=B_SPLINE_CURVE_WITH_KNOTS('',3,(#21824,#21825,#21826,#21827,#21828,
#21829,#21830,#21831,#21832,#21833,#21834,#21835,#21836,#21837,#21838,#21839,
#21840,#21841,#21842,#21843,#21844,#21845,#21846,#21847,#21848,#21849,#21850,
#21851,#21852,#21853,#21854,#21855,#21856,#21857,#21858,#21859,#21860,#21861),
 .UNSPECIFIED.,.F.,.F.,(4,2,2,2,2,2,2,2,2,2,2,2,2,2,2,2,2,2,4),(2.31659118770115,
2.32826973319217,2.40239574110813,2.47943317469564,2.55383013302291,2.62881186695812,
2.70572051605027,2.7791742554401,2.85500063903863,2.93262228782763,3.00656660516336,
3.08339822550777,3.15825784805007,3.23305942009264,3.31000255015091,3.38358499197676,
3.4592295195039,3.53611466606664,3.53614671007338),.UNSPECIFIED.);
#941=B_SPLINE_CURVE_WITH_KNOTS('',3,(#21862,#21863,#21864,#21865,#21866,
#21867,#21868,#21869,#21870,#21871,#21872,#21873,#21874,#21875,#21876,#21877,
#21878,#21879,#21880,#21881,#21882,#21883,#21884,#21885,#21886,#21887,#21888,
#21889,#21890,#21891,#21892,#21893,#21894,#21895,#21896,#21897),
 .UNSPECIFIED.,.F.,.F.,(4,2,2,2,2,2,2,2,2,2,2,2,2,2,2,2,2,4),(5.27807262241528,
5.31032878063387,5.38772603381421,5.46217259388101,5.53802804503023,5.61445048702391,
5.68806469121006,5.76500582066864,5.84057124764373,5.9142960449069,5.991975837307,
6.06667282701779,6.14194400467577,6.21865141096818,6.29248720387191,6.36940565933153,
6.44514297831244,6.49826455965138),.UNSPECIFIED.);
#942=B_SPLINE_CURVE_WITH_KNOTS('',3,(#21903,#21904,#21905,#21906,#21907,
#21908,#21909,#21910,#21911,#21912,#21913,#21914,#21915,#21916,#21917,#21918,
#21919,#21920,#21921,#21922,#21923,#21924,#21925,#21926,#21927,#21928,#21929,
#21930,#21931,#21932,#21933,#21934,#21935,#21936),.UNSPECIFIED.,.F.,.F.,
(4,2,2,2,2,2,2,2,2,2,2,2,2,2,2,2,4),(7.71789666424489,7.72653208826837,
7.80344520584536,7.87877178630723,7.95267300617573,8.030092507589,8.10455789544369,
8.18032197698524,8.25676746857915,8.33039655432369,8.40733016361098,8.48291789543391,
8.55661319786207,8.63431788624882,8.70903611278883,8.76144236640241,8.8157845358832),
 .UNSPECIFIED.);
#943=B_SPLINE_CURVE_WITH_KNOTS('',3,(#21939,#21940,#21941,#21942,#21943,
#21944,#21945,#21946,#21947,#21948,#21949,#21950,#21951,#21952,#21953,#21954,
#21955,#21956,#21957,#21958,#21959,#21960,#21961,#21962,#21963,#21964,#21965,
#21966,#21967,#21968,#21969,#21970),.UNSPECIFIED.,.F.,.F.,(4,2,2,2,2,2,
2,2,2,2,2,2,2,2,2,4),(3.04265172955979E-8,0.0696297941849091,0.137949529099503,
0.213754729172505,0.291233561600052,0.365153025689182,0.441960629532694,
0.516719666380062,0.591495500873055,0.668388103886677,0.741907722473969,
0.81752609162172,0.894388800621883,0.968111365668341,1.044695954011,1.09710239300357),
 .UNSPECIFIED.);
#944=B_SPLINE_CURVE_WITH_KNOTS('',3,(#21977,#21978,#21979,#21980,#21981,
#21982,#21983,#21984,#21985,#21986,#21987,#21988,#21989,#21990),
 .UNSPECIFIED.,.F.,.F.,(4,2,2,2,2,2,4),(0.,0.0516156037256129,0.104843298805831,
0.181708269088802,0.255105736797692,0.330969171143205,0.40012079681341),
 .UNSPECIFIED.);
#945=B_SPLINE_CURVE_WITH_KNOTS('',3,(#21996,#21997,#21998,#21999,#22000,
#22001,#22002,#22003,#22004,#22005,#22006,#22007,#22008,#22009,#22010,#22011),
 .UNSPECIFIED.,.F.,.F.,(4,2,2,2,2,2,2,4),(7.19320368173748,7.22969104328008,
7.30685234318868,7.38108572364049,7.45736679271042,7.5335484251732,7.60230579029071,
7.67143903154297),.UNSPECIFIED.);
#946=B_SPLINE_CURVE_WITH_KNOTS('',3,(#22013,#22014,#22015,#22016,#22017,
#22018,#22019,#22020,#22021,#22022,#22023,#22024,#22025,#22026,#22027,#22028,
#22029,#22030,#22031,#22032,#22033,#22034,#22035,#22036,#22037,#22038,#22039,
#22040,#22041,#22042,#22043,#22044,#22045,#22046,#22047,#22048,#22049,#22050),
 .UNSPECIFIED.,.F.,.F.,(4,2,2,2,2,2,2,2,2,2,2,2,2,2,2,2,2,2,4),(0.40012079681341,
0.408262580632944,0.482230401205284,0.559092019925671,0.63374815619767,
0.70857183794918,0.785464064334543,0.85895655236679,0.934623115130469,1.01149009246842,
1.08525773364797,1.16189268840959,1.23717618385871,1.31180520136737,1.38941196483489,
1.46311319181338,1.53860919994804,1.61550499885784,1.6194726882503),
 .UNSPECIFIED.);
#947=B_SPLINE_CURVE_WITH_KNOTS('',3,(#22055,#22056,#22057,#22058,#22059,
#22060,#22061,#22062,#22063,#22064,#22065,#22066,#22067,#22068,#22069,#22070,
#22071,#22072,#22073,#22074,#22075,#22076,#22077,#22078,#22079,#22080,#22081,
#22082,#22083,#22084,#22085,#22086,#22087,#22088,#22089,#22090),
 .UNSPECIFIED.,.F.,.F.,(4,2,2,2,2,2,2,2,2,2,2,2,2,2,2,2,2,4),(5.97412374917029,
6.02336400909286,6.10006341984595,6.17388859912431,6.25076071690477,6.32648861382979,
6.39995163612972,6.47684257851413,6.55172701297119,6.62625691295634,6.70318696737316,
6.77721590255347,6.854278498152,6.93021529134235,7.00361377047219,7.08048358100381,
7.15557375604146,7.19320368173748),.UNSPECIFIED.);
#948=B_SPLINE_CURVE_WITH_KNOTS('',3,(#22091,#22092,#22093,#22094,#22095,
#22096,#22097,#22098,#22099,#22100,#22101,#22102,#22103,#22104,#22105,#22106,
#22107,#22108,#22109,#22110,#22111,#22112,#22113,#22114,#22115,#22116,#22117,
#22118,#22119,#22120,#22121,#22122,#22123,#22124,#22125,#22126),
 .UNSPECIFIED.,.F.,.F.,(4,2,2,2,2,2,2,2,2,2,2,2,2,2,2,2,2,4),(1.6194726882503,
1.68905849303729,1.76541032665973,1.84129252631949,1.91567338868131,1.99300012566542,
2.06693615648198,2.14217646085893,2.21905740368734,2.29248463242846,2.36857454962031,
2.44518201191493,2.51933977125269,2.59641439483466,2.67070416400376,2.74571771802852,
2.82260704900321,2.83860278179673),.UNSPECIFIED.);
#949=B_SPLINE_CURVE_WITH_KNOTS('',3,(#22131,#22132,#22133,#22134,#22135,
#22136,#22137,#22138,#22139,#22140,#22141,#22142,#22143,#22144,#22145,#22146,
#22147,#22148,#22149,#22150,#22151,#22152,#22153,#22154,#22155,#22156,#22157,
#22158,#22159,#22160,#22161,#22162,#22163,#22164,#22165,#22166),
 .UNSPECIFIED.,.F.,.F.,(4,2,2,2,2,2,2,2,2,2,2,2,2,2,2,2,2,4),(4.75497373083379,
4.81676779440289,4.89291059093653,4.96634139896639,5.04320276424534,5.11849451623879,
5.19232799861128,5.26971286680881,5.34414356991651,5.41981447496161,5.49622630208646,
5.569819705332,5.6467031993209,5.72225738250597,5.79589351191985,5.87356474206349,
5.94824936087176,5.97412374917029),.UNSPECIFIED.);
#950=B_SPLINE_CURVE_WITH_KNOTS('',3,(#22167,#22168,#22169,#22170,#22171,
#22172,#22173,#22174,#22175,#22176,#22177,#22178,#22179,#22180,#22181,#22182,
#22183,#22184,#22185,#22186,#22187,#22188,#22189,#22190,#22191,#22192,#22193,
#22194,#22195,#22196,#22197,#22198,#22199,#22200,#22201,#22202),
 .UNSPECIFIED.,.F.,.F.,(4,2,2,2,2,2,2,2,2,2,2,2,2,2,2,2,2,4),(2.83860278179673,
2.89603171119237,2.97189045168826,3.04930918599773,3.12327689819132,3.2001363825891,
3.27487293038277,3.34969704764319,3.42661621894219,3.50014825261352,3.57581534615027,
3.65270673276762,3.72647589461863,3.80311052589585,3.87849224559284,3.95312400477735,
4.03073091488501,4.05823822884819),.UNSPECIFIED.);
#951=B_SPLINE_CURVE_WITH_KNOTS('',3,(#22207,#22208,#22209,#22210,#22211,
#22212,#22213,#22214,#22215,#22216,#22217,#22218,#22219,#22220,#22221,#22222,
#22223,#22224,#22225,#22226,#22227,#22228,#22229,#22230,#22231,#22232,#22233,
#22234,#22235,#22236,#22237,#22238,#22239,#22240,#22241,#22242),
 .UNSPECIFIED.,.F.,.F.,(4,2,2,2,2,2,2,2,2,2,2,2,2,2,2,2,2,4),(3.53614671007836,
3.60978705097627,3.68629180592578,3.76172365013153,3.83623446884695,3.9110890194842,
3.98566617436521,4.06256304463833,4.13656203705491,4.21371517670204,4.28961685991457,
4.36300950127383,4.43987265649615,4.51492830686231,4.58908233355429,4.66620599354184,
4.74040545874708,4.75497373083379),.UNSPECIFIED.);
#952=B_SPLINE_CURVE_WITH_KNOTS('',3,(#22243,#22244,#22245,#22246,#22247,
#22248,#22249,#22250,#22251,#22252,#22253,#22254,#22255,#22256,#22257,#22258,
#22259,#22260,#22261,#22262,#22263,#22264,#22265,#22266,#22267,#22268,#22269,
#22270,#22271,#22272,#22273,#22274,#22275,#22276,#22277,#22278),
 .UNSPECIFIED.,.F.,.F.,(4,2,2,2,2,2,2,2,2,2,2,2,2,2,2,2,2,4),(4.05823822884819,
4.1044868013451,4.17998485839536,4.25691220078312,4.33047707477126,4.40683052560212,
4.4802904286941,4.5572202253281,4.63229702577646,4.70658607651159,4.78372774428882,
4.85794809876263,4.93451770402981,5.01067544858162,5.08415039202188,5.16107410991884,
5.23638120055169,5.27807161868402),.UNSPECIFIED.);
#953=B_SPLINE_CURVE_WITH_KNOTS('',3,(#22283,#22284,#22285,#22286,#22287,
#22288,#22289,#22290,#22291,#22292,#22293,#22294,#22295,#22296,#22297,#22298,
#22299,#22300,#22301,#22302,#22303,#22304,#22305,#22306,#22307,#22308,#22309,
#22310,#22311,#22312,#22313,#22314,#22315,#22316,#22317,#22318,#22319,#22320),
 .UNSPECIFIED.,.F.,.F.,(4,2,2,2,2,2,2,2,2,2,2,2,2,2,2,2,2,2,4),(2.31659118770463,
2.32826973319563,2.40239574111168,2.47943317469931,2.55383013302671,2.62881186696204,
2.7057205160543,2.77917425544425,2.85500063904291,2.93262228783198,3.00656660516777,
3.08339822551228,3.15825784805468,3.23305942009734,3.31000255015569,3.38358499198161,
3.45922951950883,3.5361146660716,3.53614671007836),.UNSPECIFIED.);
#954=B_SPLINE_CURVE_WITH_KNOTS('',3,(#22321,#22322,#22323,#22324,#22325,
#22326,#22327,#22328,#22329,#22330,#22331,#22332,#22333,#22334,#22335,#22336,
#22337,#22338,#22339,#22340,#22341,#22342,#22343,#22344,#22345,#22346,#22347,
#22348,#22349,#22350,#22351,#22352,#22353,#22354,#22355,#22356),
 .UNSPECIFIED.,.F.,.F.,(4,2,2,2,2,2,2,2,2,2,2,2,2,2,2,2,2,4),(5.27807161868402,
5.31032777693036,5.38772503012124,5.46217159019827,5.53802704136127,5.6144494833653,
5.68806368756168,5.76500481703162,5.84057024401696,5.91429504129166,5.99197483370221,
6.06667182342315,6.14194300109424,6.21865040739694,6.29248620031064,6.36940465578137,
6.4451419747725,6.49826355609911),.UNSPECIFIED.);
#955=B_SPLINE_CURVE_WITH_KNOTS('',3,(#22362,#22363,#22364,#22365,#22366,
#22367,#22368,#22369,#22370,#22371,#22372,#22373,#22374,#22375,#22376,#22377,
#22378,#22379,#22380,#22381,#22382,#22383,#22384,#22385,#22386,#22387,#22388,
#22389,#22390,#22391,#22392,#22393,#22394,#22395),.UNSPECIFIED.,.F.,.F.,
(4,2,2,2,2,2,2,2,2,2,2,2,2,2,2,2,4),(7.71789566086823,7.72653108491538,
7.80344420250335,7.8787707829751,7.9526720028552,8.03009150427855,8.10455689214304,
8.18032097369781,8.25676646530167,8.33039555105596,8.40732916035414,8.48291689218689,
8.55661219462614,8.63431688302293,8.70903510957268,8.76144136318372,8.81578353266249),
 .UNSPECIFIED.);
#956=B_SPLINE_CURVE_WITH_KNOTS('',3,(#22398,#22399,#22400,#22401,#22402,
#22403,#22404,#22405,#22406,#22407,#22408,#22409,#22410,#22411,#22412,#22413,
#22414,#22415,#22416,#22417,#22418,#22419,#22420,#22421,#22422,#22423,#22424,
#22425,#22426,#22427,#22428,#22429),.UNSPECIFIED.,.F.,.F.,(4,2,2,2,2,2,
2,2,2,2,2,2,2,2,2,4),(3.04265128429249E-8,0.0696297941848276,0.137949529099356,
0.213754729172342,0.291233561599973,0.365153025689176,0.441960629532743,
0.516719666380159,0.591495500873206,0.668388103886912,0.741907722474293,
0.817526091622124,0.89438880062244,0.968111365669073,1.04469595401189,1.09710239300462),
 .UNSPECIFIED.);
#957=B_SPLINE_CURVE_WITH_KNOTS('',3,(#22436,#22437,#22438,#22439,#22440,
#22441,#22442,#22443,#22444,#22445,#22446,#22447,#22448,#22449),
 .UNSPECIFIED.,.F.,.F.,(4,2,2,2,2,2,4),(9.99999998850988E-7,0.0516169518680174,
0.104845041291632,0.181709819458214,0.255107103717481,0.330970348449006,
0.40012180130331),.UNSPECIFIED.);
#958=B_SPLINE_CURVE_WITH_KNOTS('',3,(#22455,#22456,#22457,#22458,#22459,
#22460,#22461,#22462,#22463,#22464,#22465,#22466,#22467,#22468,#22469,#22470),
 .UNSPECIFIED.,.F.,.F.,(4,2,2,2,2,2,2,4),(7.19320368172767,7.22969104327013,
7.30685234317884,7.38108572363072,7.4573667927007,7.53354842516364,7.60230579028133,
7.67143903153375),.UNSPECIFIED.);
#959=B_SPLINE_CURVE_WITH_KNOTS('',3,(#22472,#22473,#22474,#22475,#22476,
#22477,#22478,#22479,#22480,#22481,#22482,#22483,#22484,#22485,#22486,#22487,
#22488,#22489,#22490,#22491,#22492,#22493,#22494,#22495,#22496,#22497,#22498,
#22499,#22500,#22501,#22502,#22503,#22504,#22505,#22506,#22507,#22508,#22509),
 .UNSPECIFIED.,.F.,.F.,(4,2,2,2,2,2,2,2,2,2,2,2,2,2,2,2,2,2,4),(0.40012180130331,
0.408263585102685,0.48223140566233,0.559093024369444,0.633749160630985,
0.7085728423697,0.785465068742682,0.858957556763468,0.934624119514201,1.0114910968397,
1.08525873800664,1.16189369275507,1.23717718819415,1.31180620569013,1.38941296914438,
1.46311419611182,1.53861020423359,1.61550600313119,1.61947369254408),
 .UNSPECIFIED.);
#960=B_SPLINE_CURVE_WITH_KNOTS('',3,(#22514,#22515,#22516,#22517,#22518,
#22519,#22520,#22521,#22522,#22523,#22524,#22525,#22526,#22527,#22528,#22529,
#22530,#22531,#22532,#22533,#22534,#22535,#22536,#22537,#22538,#22539,#22540,
#22541,#22542,#22543,#22544,#22545,#22546,#22547,#22548,#22549),
 .UNSPECIFIED.,.F.,.F.,(4,2,2,2,2,2,2,2,2,2,2,2,2,2,2,2,2,4),(5.974123749161,
6.02336400908333,6.10006341983629,6.17388859911447,6.2507607168948,6.32648861381977,
6.39995163611967,6.47684257850402,6.55172701296104,6.62625691294614,6.70318696736296,
6.77721590254322,6.85427849814168,6.93021529133211,7.003613770462,7.08048358099369,
7.15557375603143,7.19320368172767),.UNSPECIFIED.);
#961=B_SPLINE_CURVE_WITH_KNOTS('',3,(#22550,#22551,#22552,#22553,#22554,
#22555,#22556,#22557,#22558,#22559,#22560,#22561,#22562,#22563,#22564,#22565,
#22566,#22567,#22568,#22569,#22570,#22571,#22572,#22573,#22574,#22575,#22576,
#22577,#22578,#22579,#22580,#22581,#22582,#22583,#22584,#22585),
 .UNSPECIFIED.,.F.,.F.,(4,2,2,2,2,2,2,2,2,2,2,2,2,2,2,2,2,4),(1.61947369254408,
1.68905949729837,1.76541133090778,1.84129353055796,1.91567439290728,1.99300112987828,
2.06693716068424,2.14217746504849,2.21905840786482,2.29248563659418,2.36857555377319,
2.44518301605857,2.51934077538404,2.59641539895315,2.67070516811205,2.74571872212431,
2.82260805308708,2.83860378589876),.UNSPECIFIED.);
#962=B_SPLINE_CURVE_WITH_KNOTS('',3,(#22590,#22591,#22592,#22593,#22594,
#22595,#22596,#22597,#22598,#22599,#22600,#22601,#22602,#22603,#22604,#22605,
#22606,#22607,#22608,#22609,#22610,#22611,#22612,#22613,#22614,#22615,#22616,
#22617,#22618,#22619,#22620,#22621,#22622,#22623,#22624,#22625),
 .UNSPECIFIED.,.F.,.F.,(4,2,2,2,2,2,2,2,2,2,2,2,2,2,2,2,2,4),(4.75497373082735,
4.81676779439626,4.89291059092976,4.96634139895943,5.04320276423819,5.11849451623147,
5.19232799860378,5.2697128668011,5.34414356990862,5.41981447495354,5.49622630207823,
5.56981970532358,5.6467031993123,5.72225738249718,5.79589351191087,5.87356474205431,
5.94824936086241,5.974123749161),.UNSPECIFIED.);
#963=B_SPLINE_CURVE_WITH_KNOTS('',3,(#22626,#22627,#22628,#22629,#22630,
#22631,#22632,#22633,#22634,#22635,#22636,#22637,#22638,#22639,#22640,#22641,
#22642,#22643,#22644,#22645,#22646,#22647,#22648,#22649,#22650,#22651,#22652,
#22653,#22654,#22655,#22656,#22657,#22658,#22659,#22660,#22661),
 .UNSPECIFIED.,.F.,.F.,(4,2,2,2,2,2,2,2,2,2,2,2,2,2,2,2,2,4),(2.83860378589876,
2.89603271526497,2.97189145574824,3.04931019004864,3.12327790223017,3.20013738661533,
3.27487393439905,3.34969805164721,3.42661722293439,3.50014925659483,3.57581635011919,
3.65270773672471,3.72647689856381,3.80311152982859,3.87849324951609,3.95312500868852,
4.03073191878357,4.05823923276311),.UNSPECIFIED.);
#964=B_SPLINE_CURVE_WITH_KNOTS('',3,(#22666,#22667,#22668,#22669,#22670,
#22671,#22672,#22673,#22674,#22675,#22676,#22677,#22678,#22679,#22680,#22681,
#22682,#22683,#22684,#22685,#22686,#22687,#22688,#22689,#22690,#22691,#22692,
#22693,#22694,#22695,#22696,#22697,#22698,#22699,#22700,#22701),
 .UNSPECIFIED.,.F.,.F.,(4,2,2,2,2,2,2,2,2,2,2,2,2,2,2,2,2,4),(3.53614671007441,
3.6097870509723,3.68629180592174,3.76172365012743,3.83623446884277,3.91108901947988,
3.98566617436073,4.06256304463361,4.13656203704999,4.21371517669692,4.28961685990926,
4.36300950126833,4.43987265649047,4.51492830685644,4.58908233354824,4.66620599353558,
4.74040545874063,4.75497373082735),.UNSPECIFIED.);
#965=B_SPLINE_CURVE_WITH_KNOTS('',3,(#22702,#22703,#22704,#22705,#22706,
#22707,#22708,#22709,#22710,#22711,#22712,#22713,#22714,#22715,#22716,#22717,
#22718,#22719,#22720,#22721,#22722,#22723,#22724,#22725,#22726,#22727,#22728,
#22729,#22730,#22731,#22732,#22733,#22734,#22735,#22736,#22737),
 .UNSPECIFIED.,.F.,.F.,(4,2,2,2,2,2,2,2,2,2,2,2,2,2,2,2,2,4),(4.05823923276311,
4.10448780523323,4.17998586227126,4.25691320464737,4.33047807862384,4.40683152944232,
4.48029143252306,4.5572212291454,4.63229802958326,4.70658708030576,4.78372874807228,
4.8579491025357,4.93451870778849,5.01067645232983,5.08415139575935,5.1610751136448,
5.23638220426729,5.27807262241528),.UNSPECIFIED.);
#966=B_SPLINE_CURVE_WITH_KNOTS('',3,(#22742,#22743,#22744,#22745,#22746,
#22747,#22748,#22749,#22750,#22751,#22752,#22753,#22754,#22755,#22756,#22757,
#22758,#22759,#22760,#22761,#22762,#22763,#22764,#22765,#22766,#22767,#22768,
#22769,#22770,#22771,#22772,#22773,#22774,#22775,#22776,#22777,#22778,#22779),
 .UNSPECIFIED.,.F.,.F.,(4,2,2,2,2,2,2,2,2,2,2,2,2,2,2,2,2,2,4),(2.31659118770178,
2.32826973319281,2.40239574110879,2.47943317469632,2.55383013302362,2.62881186695886,
2.70572051605103,2.77917425544088,2.85500063903944,2.93262228782847,3.00656660516422,
3.08339822550865,3.15825784805098,3.23305942009357,3.31000255015187,3.38358499197773,
3.45922951950491,3.53611466606766,3.53614671007441),.UNSPECIFIED.);
#967=B_SPLINE_CURVE_WITH_KNOTS('',3,(#22780,#22781,#22782,#22783,#22784,
#22785,#22786,#22787,#22788,#22789,#22790,#22791,#22792,#22793,#22794,#22795,
#22796,#22797,#22798,#22799,#22800,#22801,#22802,#22803,#22804,#22805,#22806,
#22807,#22808,#22809,#22810,#22811,#22812,#22813,#22814,#22815),
 .UNSPECIFIED.,.F.,.F.,(4,2,2,2,2,2,2,2,2,2,2,2,2,2,2,2,2,4),(5.27807262241528,
5.31032878063387,5.38772603381421,5.46217259388101,5.53802804503023,5.61445048702391,
5.68806469121006,5.76500582066864,5.84057124764373,5.9142960449069,5.991975837307,
6.06667282701779,6.14194400467577,6.21865141096818,6.29248720387191,6.36940565933153,
6.44514297831244,6.49826455965138),.UNSPECIFIED.);
#968=B_SPLINE_CURVE_WITH_KNOTS('',3,(#22821,#22822,#22823,#22824,#22825,
#22826,#22827,#22828,#22829,#22830,#22831,#22832,#22833,#22834,#22835,#22836,
#22837,#22838,#22839,#22840,#22841,#22842,#22843,#22844,#22845,#22846,#22847,
#22848,#22849,#22850,#22851,#22852,#22853,#22854),.UNSPECIFIED.,.F.,.F.,
(4,2,2,2,2,2,2,2,2,2,2,2,2,2,2,2,4),(7.71789666424489,7.72653208826837,
7.80344520584536,7.87877178630723,7.95267300617573,8.030092507589,8.10455789544369,
8.18032197698524,8.25676746857915,8.33039655432369,8.40733016361098,8.48291789543391,
8.55661319786207,8.63431788624882,8.70903611278883,8.76144236640241,8.8157845358832),
 .UNSPECIFIED.);
#969=B_SPLINE_CURVE_WITH_KNOTS('',3,(#22857,#22858,#22859,#22860,#22861,
#22862,#22863,#22864,#22865,#22866,#22867,#22868,#22869,#22870,#22871,#22872,
#22873,#22874,#22875,#22876,#22877,#22878,#22879,#22880,#22881,#22882,#22883,
#22884,#22885,#22886,#22887,#22888),.UNSPECIFIED.,.F.,.F.,(4,2,2,2,2,2,
2,2,2,2,2,2,2,2,2,4),(3.04265172991663E-8,0.0696297941849219,0.137949529099536,
0.21375472917256,0.291233561600128,0.365153025689274,0.441960629532807,
0.516719666380197,0.591495500873207,0.668388103886848,0.74190772247416,
0.817526091621932,0.894388800622119,0.968111365668598,1.04469595401127,
1.09710239300385),.UNSPECIFIED.);
#970=B_SPLINE_CURVE_WITH_KNOTS('',3,(#22895,#22896,#22897,#22898,#22899,
#22900,#22901,#22902,#22903,#22904,#22905,#22906,#22907,#22908),
 .UNSPECIFIED.,.F.,.F.,(4,2,2,2,2,2,4),(0.,0.0516156037392325,0.104843298833226,
0.181708269115714,0.255105736824021,0.330969171170157,0.400120796811339),
 .UNSPECIFIED.);
#971=B_SPLINE_CURVE_WITH_KNOTS('',3,(#22914,#22915,#22916,#22917,#22918,
#22919,#22920,#22921,#22922,#22923,#22924,#22925,#22926,#22927,#22928,#22929),
 .UNSPECIFIED.,.F.,.F.,(4,2,2,2,2,2,2,4),(7.19320368173771,7.22969111960813,
7.30685258093042,7.381086116671,7.45736734531324,7.53354913714033,7.60230617175925,
7.67143902533004),.UNSPECIFIED.);
#972=B_SPLINE_CURVE_WITH_KNOTS('',3,(#22931,#22932,#22933,#22934,#22935,
#22936,#22937,#22938,#22939,#22940,#22941,#22942,#22943,#22944,#22945,#22946,
#22947,#22948,#22949,#22950,#22951,#22952,#22953,#22954,#22955,#22956,#22957,
#22958,#22959,#22960,#22961,#22962,#22963,#22964,#22965,#22966,#22967,#22968),
 .UNSPECIFIED.,.F.,.F.,(4,2,2,2,2,2,2,2,2,2,2,2,2,2,2,2,2,2,4),(0.400120796811339,
0.408262580655585,0.482230401228364,0.559092019949293,0.633748156218688,
0.708571837970628,0.785464064355422,0.858956552386623,0.93462311515074,
1.01149009248822,1.08525773366815,1.16189268843024,1.23717618387609,1.3118052013851,
1.3894119648531,1.46311319182998,1.53860919996502,1.61550499887409,1.6194726882389),
 .UNSPECIFIED.);
#973=B_SPLINE_CURVE_WITH_KNOTS('',3,(#22973,#22974,#22975,#22976,#22977,
#22978,#22979,#22980,#22981,#22982,#22983,#22984,#22985,#22986,#22987,#22988,
#22989,#22990,#22991,#22992,#22993,#22994,#22995,#22996,#22997,#22998,#22999,
#23000,#23001,#23002,#23003,#23004,#23005,#23006,#23007,#23008),
 .UNSPECIFIED.,.F.,.F.,(4,2,2,2,2,2,2,2,2,2,2,2,2,2,2,2,2,4),(5.97412374917094,
6.02336400909344,6.1000634198465,6.17388859912484,6.25076071690528,6.32648861383027,
6.39995163613019,6.47684257851458,6.55172701297161,6.62625691295673,6.70318696737352,
6.77721590255381,6.8542784981523,6.93021529134263,7.00361377047243,7.08048358100402,
7.15557375604164,7.19320368173771),.UNSPECIFIED.);
#974=B_SPLINE_CURVE_WITH_KNOTS('',3,(#23009,#23010,#23011,#23012,#23013,
#23014,#23015,#23016,#23017,#23018,#23019,#23020,#23021,#23022,#23023,#23024,
#23025,#23026,#23027,#23028,#23029,#23030,#23031,#23032,#23033,#23034,#23035,
#23036,#23037,#23038,#23039,#23040,#23041,#23042,#23043,#23044),
 .UNSPECIFIED.,.F.,.F.,(4,2,2,2,2,2,2,2,2,2,2,2,2,2,2,2,2,4),(1.6194726882389,
1.68905849305358,1.76541032667645,1.84129252633228,1.91567338869436,1.99300012567884,
2.06693615649319,2.14217646087043,2.21905740369798,2.29248463243857,2.36857454963071,
2.4451820119209,2.5193397712588,2.596414394841,2.67070416400741,2.7457177180323,
2.82260704900607,2.83860278177238),.UNSPECIFIED.);
#975=B_SPLINE_CURVE_WITH_KNOTS('',3,(#23049,#23050,#23051,#23052,#23053,
#23054,#23055,#23056,#23057,#23058,#23059,#23060,#23061,#23062,#23063,#23064,
#23065,#23066,#23067,#23068,#23069,#23070,#23071,#23072,#23073,#23074,#23075,
#23076,#23077,#23078,#23079,#23080,#23081,#23082,#23083,#23084),
 .UNSPECIFIED.,.F.,.F.,(4,2,2,2,2,2,2,2,2,2,2,2,2,2,2,2,2,4),(4.75497373083482,
4.81676779440388,4.89291059093751,4.96634139896734,5.04320276424626,5.11849451623969,
5.19232799861215,5.26971286680966,5.34414356991732,5.41981447496239,5.4962263020872,
5.56981970533272,5.6467031993216,5.72225738250664,5.7958935119205,5.87356474206412,
5.94824936087237,5.97412374917094),.UNSPECIFIED.);
#976=B_SPLINE_CURVE_WITH_KNOTS('',3,(#23085,#23086,#23087,#23088,#23089,
#23090,#23091,#23092,#23093,#23094,#23095,#23096,#23097,#23098,#23099,#23100,
#23101,#23102,#23103,#23104,#23105,#23106,#23107,#23108,#23109,#23110,#23111,
#23112,#23113,#23114,#23115,#23116,#23117,#23118,#23119,#23120),
 .UNSPECIFIED.,.F.,.F.,(4,2,2,2,2,2,2,2,2,2,2,2,2,2,2,2,2,4),(2.83860278177238,
2.89603171119416,2.9718904516902,3.04930918599495,3.12327689818853,3.20013638258635,
3.27487293037699,3.34969704763737,3.42661621893534,3.50014825260515,3.57581534614186,
3.65270673275826,3.72647589460919,3.80311052588641,3.87849224557971,3.95312400476411,
4.03073091487175,4.05823822880769),.UNSPECIFIED.);
#977=B_SPLINE_CURVE_WITH_KNOTS('',3,(#23125,#23126,#23127,#23128,#23129,
#23130,#23131,#23132,#23133,#23134,#23135,#23136,#23137,#23138,#23139,#23140,
#23141,#23142,#23143,#23144,#23145,#23146,#23147,#23148,#23149,#23150,#23151,
#23152,#23153,#23154,#23155,#23156,#23157,#23158,#23159,#23160),
 .UNSPECIFIED.,.F.,.F.,(4,2,2,2,2,2,2,2,2,2,2,2,2,2,2,2,2,4),(3.53614671007962,
3.60978705097756,3.6862918059271,3.76172365013287,3.83623446884831,3.91108901948555,
3.98566617436653,4.06256304463961,4.13656203705616,4.21371517670325,4.28961685991574,
4.36300950127498,4.43987265649728,4.5149283068634,4.58908233355535,4.66620599354287,
4.74040545874809,4.75497373083482),.UNSPECIFIED.);
#978=B_SPLINE_CURVE_WITH_KNOTS('',3,(#23161,#23162,#23163,#23164,#23165,
#23166,#23167,#23168,#23169,#23170,#23171,#23172,#23173,#23174,#23175,#23176,
#23177,#23178,#23179,#23180,#23181,#23182,#23183,#23184,#23185,#23186,#23187,
#23188,#23189,#23190,#23191,#23192,#23193,#23194,#23195,#23196),
 .UNSPECIFIED.,.F.,.F.,(4,2,2,2,2,2,2,2,2,2,2,2,2,2,2,2,2,4),(4.05823822880769,
4.10448680132977,4.17998485837995,4.25691220076652,4.33047707475418,4.40683052558499,
4.48029042867599,4.55722022530881,4.6322970257549,4.70658607649072,4.78372774426551,
4.85794809873707,4.93451770400669,5.01067544855601,5.08415039199467,5.16107410989033,
5.23638120052075,5.2780716186238),.UNSPECIFIED.);
#979=B_SPLINE_CURVE_WITH_KNOTS('',3,(#23201,#23202,#23203,#23204,#23205,
#23206,#23207,#23208,#23209,#23210,#23211,#23212,#23213,#23214,#23215,#23216,
#23217,#23218,#23219,#23220,#23221,#23222,#23223,#23224,#23225,#23226,#23227,
#23228,#23229,#23230,#23231,#23232,#23233,#23234,#23235,#23236,#23237,#23238),
 .UNSPECIFIED.,.F.,.F.,(4,2,2,2,2,2,2,2,2,2,2,2,2,2,2,2,2,2,4),(2.31659118770536,
2.32826973319637,2.40239574111246,2.47943317470013,2.55383013302756,2.62881186696292,
2.70572051605522,2.77917425544518,2.85500063904386,2.93262228783295,3.00656660516877,
3.08339822551331,3.15825784805574,3.23305942009844,3.31000255015683,3.38358499198278,
3.45922951951005,3.53611466607286,3.53614671007962),.UNSPECIFIED.);
#980=B_SPLINE_CURVE_WITH_KNOTS('',3,(#23239,#23240,#23241,#23242,#23243,
#23244,#23245,#23246,#23247,#23248,#23249,#23250,#23251,#23252,#23253,#23254,
#23255,#23256,#23257,#23258,#23259,#23260,#23261,#23262,#23263,#23264,#23265,
#23266,#23267,#23268,#23269,#23270,#23271,#23272,#23273,#23274),
 .UNSPECIFIED.,.F.,.F.,(4,2,2,2,2,2,2,2,2,2,2,2,2,2,2,2,2,4),(5.2780716186238,
5.31032777689959,5.38772503008789,5.46217159016254,5.53802704132747,5.61444948332891,
5.68806368752308,5.76500481699161,5.84057024397439,5.91429504124862,5.99197483365645,
6.06667182337488,6.14194300104719,6.21865040734719,6.29248620025837,6.36940465572739,
6.44514197471589,6.49826355601516),.UNSPECIFIED.);
#981=B_SPLINE_CURVE_WITH_KNOTS('',3,(#23280,#23281,#23282,#23283,#23284,
#23285,#23286,#23287,#23288,#23289,#23290,#23291,#23292,#23293,#23294,#23295,
#23296,#23297,#23298,#23299,#23300,#23301,#23302,#23303,#23304,#23305,#23306,
#23307,#23308,#23309,#23310,#23311,#23312,#23313),.UNSPECIFIED.,.F.,.F.,
(4,2,2,2,2,2,2,2,2,2,2,2,2,2,2,2,4),(7.71789566075662,7.72653108483295,
7.803444202419,7.8787707828877,7.95267200276729,8.03009150418741,8.10455689204888,
8.18032097360487,8.25676646520549,8.33039555095692,8.40732916025302,8.48291689208259,
8.5566121945207,8.63431688291413,8.70903510946076,8.76144136305708,8.81578353252107),
 .UNSPECIFIED.);
#982=B_SPLINE_CURVE_WITH_KNOTS('',3,(#23316,#23317,#23318,#23319,#23320,
#23321,#23322,#23323,#23324,#23325,#23326,#23327,#23328,#23329,#23330,#23331,
#23332,#23333,#23334,#23335,#23336,#23337,#23338,#23339,#23340,#23341,#23342,
#23343,#23344,#23345,#23346,#23347),.UNSPECIFIED.,.F.,.F.,(4,2,2,2,2,2,
2,2,2,2,2,2,2,2,2,4),(3.04265160429364E-8,0.069629794184829,0.137949529099366,
0.213754729172367,0.291233561600009,0.365153025689221,0.441960629532807,
0.51671966638024,0.591495500873295,0.668388103887014,0.741907722474407,
0.817526091622261,0.8943888006226,0.96811136566926,1.0446959540121,1.09710239300487),
 .UNSPECIFIED.);
#983=B_SPLINE_CURVE_WITH_KNOTS('',3,(#23349,#23350,#23351,#23352,#23353,
#23354,#23355,#23356,#23357,#23358,#23359,#23360,#23361,#23362,#23363,#23364,
#23365,#23366,#23367,#23368,#23369,#23370,#23371,#23372,#23373,#23374,#23375,
#23376,#23377,#23378,#23379,#23380,#23381,#23382,#23383,#23384),
 .UNSPECIFIED.,.F.,.F.,(4,2,2,2,2,2,2,2,2,2,2,2,2,2,2,2,2,4),(1.09710239300487,
1.12011517711278,1.19470090123193,1.27225761508382,1.34601419186938,1.42146508618074,
1.49836987210414,1.57189808509923,1.64820345609062,1.72425249768454,1.7985949229751,
1.87587698848718,1.94989642538678,2.02509727325677,2.10199260325516,2.17542254085659,
2.25147199531572,2.31659118770536),.UNSPECIFIED.);
#984=B_SPLINE_CURVE_WITH_KNOTS('',3,(#23385,#23386,#23387,#23388,#23389,
#23390,#23391,#23392,#23393,#23394,#23395,#23396,#23397,#23398,#23399,#23400,
#23401,#23402,#23403,#23404,#23405,#23406,#23407,#23408,#23409,#23410,#23411,
#23412,#23413,#23414,#23415,#23416,#23417,#23418,#23419,#23420),
 .UNSPECIFIED.,.F.,.F.,(4,2,2,2,2,2,2,2,2,2,2,2,2,2,2,2,2,4),(6.49826355601516,
6.51867068512192,6.59561216979648,6.67050587384408,6.74516442447251,6.82210014899345,
6.89613760570075,6.97339767877051,7.04933639285787,7.12278074933092,7.1996971518762,
7.27478951608072,7.34901910305193,7.42617920383861,7.50041497326189,7.57687878673137,
7.65305660455958,7.71789566075662),.UNSPECIFIED.);
#985=B_SPLINE_CURVE_WITH_KNOTS('',3,(#23422,#23423,#23424,#23425,#23426,
#23427,#23428,#23429,#23430,#23431,#23432,#23433,#23434,#23435,#23436,#23437,
#23438,#23439,#23440,#23441,#23442,#23443,#23444,#23445,#23446,#23447,#23448,
#23449,#23450,#23451,#23452,#23453,#23454,#23455,#23456,#23457),
 .UNSPECIFIED.,.F.,.F.,(4,2,2,2,2,2,2,2,2,2,2,2,2,2,2,2,2,4),(1.09710239300385,
1.12011517711179,1.19470090123079,1.27225761508249,1.34601419186788,1.42146508617906,
1.49836987210228,1.5718980850972,1.64820345608845,1.72425249768224,1.79859492297267,
1.87587698848456,1.94989642538399,2.02509727325381,2.10199260325204,2.1754225408533,
2.25147199531227,2.31659118770178),.UNSPECIFIED.);
#986=B_SPLINE_CURVE_WITH_KNOTS('',3,(#23458,#23459,#23460,#23461,#23462,
#23463,#23464,#23465,#23466,#23467,#23468,#23469,#23470,#23471,#23472,#23473,
#23474,#23475,#23476,#23477,#23478,#23479,#23480,#23481,#23482,#23483,#23484,
#23485,#23486,#23487,#23488,#23489,#23490,#23491,#23492,#23493),
 .UNSPECIFIED.,.F.,.F.,(4,2,2,2,2,2,2,2,2,2,2,2,2,2,2,2,2,4),(6.49826455965138,
6.5186716887085,6.5956131733735,6.67050687741361,6.74516542802906,6.8221011525425,
6.89613860924244,6.97339868229584,7.04933739637596,7.12278175283993,7.19969815537587,
7.27479051957324,7.34902010653224,7.42618020731174,7.50041597672795,7.57687979018179,
7.65305760800301,7.71789666424489),.UNSPECIFIED.);
#987=B_SPLINE_CURVE_WITH_KNOTS('',3,(#23495,#23496,#23497,#23498,#23499,
#23500,#23501,#23502,#23503,#23504,#23505,#23506,#23507,#23508,#23509,#23510,
#23511,#23512,#23513,#23514,#23515,#23516,#23517,#23518,#23519,#23520,#23521,
#23522,#23523,#23524,#23525,#23526,#23527,#23528,#23529,#23530),
 .UNSPECIFIED.,.F.,.F.,(4,2,2,2,2,2,2,2,2,2,2,2,2,2,2,2,2,4),(1.09710239300462,
1.12011517711253,1.19470090123165,1.27225761508352,1.34601419186906,1.42146508618039,
1.49836987210376,1.57189808509882,1.64820345609019,1.72425249768409,1.79859492297463,
1.87587698848668,1.94989642538625,2.02509727325621,2.10199260325456,2.17542254085595,
2.25147199531503,2.31659118770463),.UNSPECIFIED.);
#988=B_SPLINE_CURVE_WITH_KNOTS('',3,(#23531,#23532,#23533,#23534,#23535,
#23536,#23537,#23538,#23539,#23540,#23541,#23542,#23543,#23544,#23545,#23546,
#23547,#23548,#23549,#23550,#23551,#23552,#23553,#23554,#23555,#23556,#23557,
#23558,#23559,#23560,#23561,#23562,#23563,#23564,#23565,#23566),
 .UNSPECIFIED.,.F.,.F.,(4,2,2,2,2,2,2,2,2,2,2,2,2,2,2,2,2,4),(6.49826355609911,
6.5186706851796,6.59561216985577,6.67050587390597,6.74516442453385,6.82210014905756,
6.89613760576745,6.973397678835,7.04933639292522,7.12278074939984,7.19969715194686,
7.27478951615419,7.34901910312529,7.42617920391494,7.500414973341,7.57687878680861,
7.65305660463983,7.71789566086823),.UNSPECIFIED.);
#989=B_SPLINE_CURVE_WITH_KNOTS('',3,(#23568,#23569,#23570,#23571,#23572,
#23573,#23574,#23575,#23576,#23577,#23578,#23579,#23580,#23581,#23582,#23583,
#23584,#23585,#23586,#23587,#23588,#23589,#23590,#23591,#23592,#23593,#23594,
#23595,#23596,#23597,#23598,#23599,#23600,#23601,#23602,#23603),
 .UNSPECIFIED.,.F.,.F.,(4,2,2,2,2,2,2,2,2,2,2,2,2,2,2,2,2,4),(1.09710239300357,
1.1201151771115,1.19470090123049,1.27225761508217,1.34601419186753,1.42146508617868,
1.49836987210188,1.57189808509679,1.64820345608801,1.72425249768178,1.79859492297218,
1.87587698848406,1.94989642538346,2.02509727325326,2.10199260325146,2.17542254085271,
2.25147199531166,2.31659118770115),.UNSPECIFIED.);
#990=B_SPLINE_CURVE_WITH_KNOTS('',3,(#23604,#23605,#23606,#23607,#23608,
#23609,#23610,#23611,#23612,#23613,#23614,#23615,#23616,#23617,#23618,#23619,
#23620,#23621,#23622,#23623,#23624,#23625,#23626,#23627,#23628,#23629,#23630,
#23631,#23632,#23633,#23634,#23635,#23636,#23637,#23638,#23639),
 .UNSPECIFIED.,.F.,.F.,(4,2,2,2,2,2,2,2,2,2,2,2,2,2,2,2,2,4),(6.49826455965138,
6.5186716887085,6.5956131733735,6.67050687741361,6.74516542802906,6.8221011525425,
6.89613860924244,6.97339868229584,7.04933739637596,7.12278175283993,7.19969815537587,
7.27479051957324,7.34902010653224,7.42618020731174,7.50041597672795,7.57687979018179,
7.65305760800301,7.71789666424489),.UNSPECIFIED.);
#991=B_SPLINE_CURVE_WITH_KNOTS('',3,(#23642,#23643,#23644,#23645,#23646,
#23647,#23648,#23649,#23650,#23651,#23652,#23653,#23654,#23655,#23656,#23657,
#23658,#23659,#23660,#23661,#23662,#23663,#23664,#23665,#23666,#23667,#23668,
#23669,#23670,#23671,#23672,#23673,#23674,#23675,#23676,#23677),
 .UNSPECIFIED.,.F.,.F.,(4,2,2,2,2,2,2,2,2,2,2,2,2,2,2,2,2,4),(21.3148424617523,
21.3353161897489,21.4081377842537,21.4844828604283,21.5591605315819,21.6314755220292,
21.7071973308415,21.7810434185569,21.8542546835973,21.9301267130465,22.0031298277028,
22.0786702152169,22.153570144142,22.2258725023802,22.301583175239,22.3756477399792,
22.417649122091,22.4598825016052),.UNSPECIFIED.);
#992=B_SPLINE_CURVE_WITH_KNOTS('',3,(#23680,#23681,#23682,#23683,#23684,
#23685,#23686,#23687,#23688,#23689,#23690,#23691,#23692,#23693,#23694,#23695,
#23696,#23697,#23698,#23699,#23700,#23701,#23702,#23703,#23704,#23705,#23706,
#23707,#23708,#23709,#23710,#23711),.UNSPECIFIED.,.F.,.F.,(4,2,2,2,2,2,
2,2,2,2,2,2,2,2,2,4),(9.9999999597469E-7,0.0410609715951109,0.0810353625720383,
0.153401243599348,0.228317275003317,0.304123825641722,0.377151035158167,
0.453043725999999,0.526430357230195,0.600301304337368,0.676103842764624,
0.748510230606864,0.823212972034187,0.899001954842751,0.971827250111653,
0.994462254792754),.UNSPECIFIED.);
#993=B_SPLINE_CURVE_WITH_KNOTS('',3,(#23714,#23715,#23716,#23717,#23718,
#23719,#23720,#23721,#23722,#23723,#23724,#23725,#23726,#23727,#23728,#23729,
#23730,#23731,#23732,#23733,#23734,#23735,#23736,#23737,#23738,#23739,#23740,
#23741),.UNSPECIFIED.,.F.,.F.,(4,2,2,2,2,2,2,2,2,2,2,2,2,4),(21.6282084253952,
21.6372441032614,21.7129394368562,21.7870523479308,21.8598087122815,21.9359787394778,
22.0092444905551,22.083867163104,22.1590778009158,22.2315231390981,22.3072372394324,
22.3816054833466,22.4274081248573,22.4730897400475),.UNSPECIFIED.);
#994=B_SPLINE_CURVE_WITH_KNOTS('',3,(#23744,#23745,#23746,#23747,#23748,
#23749,#23750,#23751,#23752,#23753,#23754,#23755,#23756,#23757,#23758,#23759,
#23760,#23761,#23762,#23763,#23764,#23765,#23766,#23767),.UNSPECIFIED.,
 .F.,.F.,(4,2,2,2,2,2,2,2,2,2,2,4),(9.9999999828754E-7,0.0409987765676221,
0.0809155863998274,0.15328123806841,0.228192677104899,0.304015356848976,
0.377038791813246,0.452927204977614,0.526322673925784,0.6001898532434,0.675993042874638,
0.693996851653457),.UNSPECIFIED.);
#995=B_SPLINE_CURVE_WITH_KNOTS('',3,(#23770,#23771,#23772,#23773,#23774,
#23775,#23776,#23777,#23778,#23779,#23780,#23781,#23782,#23783,#23784,#23785,
#23786,#23787,#23788,#23789),.UNSPECIFIED.,.F.,.F.,(4,2,2,2,2,2,2,2,2,4),
(21.9110024905134,21.9219460418809,21.9950982805857,22.0701188260611,22.1451953864536,
22.2175618280791,22.2932793240977,22.3675167787528,22.4116383044439,22.4558211302722),
 .UNSPECIFIED.);
#996=B_SPLINE_CURVE_WITH_KNOTS('',3,(#23792,#23793,#23794,#23795,#23796,
#23797,#23798,#23799,#23800,#23801,#23802,#23803,#23804,#23805,#23806,#23807),
 .UNSPECIFIED.,.F.,.F.,(4,2,2,2,2,2,2,4),(1.00000007208917E-6,0.0398646418385672,
0.0787292474270129,0.15109808491172,0.225926380077501,0.302048834068036,
0.375004296118167,0.393548424805639),.UNSPECIFIED.);
#997=B_SPLINE_CURVE_WITH_KNOTS('',3,(#23810,#23811,#23812,#23813,#23814,
#23815,#23816,#23817,#23818,#23819,#23820,#23821),.UNSPECIFIED.,.F.,.F.,
(4,2,2,2,2,4),(22.2034453162522,22.2090431050947,22.2847987209526,22.3591079335028,
22.4036884637069,22.4482924175264),.UNSPECIFIED.);
#998=B_SPLINE_CURVE_WITH_KNOTS('',3,(#23824,#23825,#23826,#23827,#23828,
#23829,#23830,#23831),.UNSPECIFIED.,.F.,.F.,(4,2,2,4),(9.99999993021828E-7,
0.0391830186935133,0.0774132307502166,0.0931362008875077),.UNSPECIFIED.);
#999=B_SPLINE_CURVE_WITH_KNOTS('',3,(#23856,#23857,#23858,#23859,#23860,
#23861,#23862,#23863,#23864,#23865,#23866,#23867,#23868,#23869,#23870,#23871,
#23872,#23873,#23874,#23875,#23876,#23877,#23878,#23879,#23880,#23881,#23882,
#23883),.UNSPECIFIED.,.F.,.F.,(4,2,2,2,2,2,2,2,2,2,2,2,2,4),(9.99999999757183E-7,
0.0731124278909269,0.166057761117533,0.286367941469741,0.41317168458484,
0.536466369898799,0.671513511979461,0.863012275266548,1.04829331747803,
1.23237898344787,1.40408133486915,1.58846641457555,1.74526991258573,1.84895017902434),
 .UNSPECIFIED.);
#1000=B_SPLINE_CURVE_WITH_KNOTS('',3,(#23885,#23886,#23887,#23888,#23889,
#23890,#23891,#23892,#23893,#23894,#23895,#23896),.UNSPECIFIED.,.F.,.F.,
(4,2,2,2,2,4),(1.00000013382259E-6,0.059650139456479,0.121379110068548,
0.202618081235281,0.282064568203206,0.362961601069192),.UNSPECIFIED.);
#1001=B_SPLINE_CURVE_WITH_KNOTS('',3,(#23899,#23900,#23901,#23902,#23903,
#23904,#23905,#23906,#23907,#23908,#23909,#23910,#23911,#23912),
 .UNSPECIFIED.,.F.,.F.,(4,2,2,2,2,2,4),(1.84895017902434,1.87439516116018,
2.01076363118188,2.16135413763144,2.34266213664141,2.4563787856096,2.57527002953519),
 .UNSPECIFIED.);
#1002=B_SPLINE_CURVE_WITH_KNOTS('',3,(#23918,#23919,#23920,#23921,#23922,
#23923,#23924,#23925,#23926,#23927,#23928,#23929,#23930,#23931,#23932,#23933,
#23934,#23935,#23936,#23937,#23938,#23939,#23940,#23941,#23942,#23943,#23944,
#23945),.UNSPECIFIED.,.F.,.F.,(4,2,2,2,2,2,2,2,2,2,2,2,2,4),(9.99999999927736E-7,
0.0731124278938116,0.166057761124268,0.286367941476178,0.413171684591601,
0.536466369905737,0.671513511989027,0.863012275271149,1.04829331747739,
1.23237898344594,1.40408133486366,1.58846641456642,1.7452699125751,1.84895017900088),
 .UNSPECIFIED.);
#1003=B_SPLINE_CURVE_WITH_KNOTS('',3,(#23947,#23948,#23949,#23950,#23951,
#23952,#23953,#23954,#23955,#23956,#23957,#23958),.UNSPECIFIED.,.F.,.F.,
(4,2,2,2,2,4),(0.,0.0596482959180104,0.121377436598889,0.202616631617369,
0.282063337473005,0.362960593220025),.UNSPECIFIED.);
#1004=B_SPLINE_CURVE_WITH_KNOTS('',3,(#23961,#23962,#23963,#23964,#23965,
#23966,#23967,#23968,#23969,#23970,#23971,#23972,#23973,#23974),
 .UNSPECIFIED.,.F.,.F.,(4,2,2,2,2,2,4),(1.84895017900088,1.87439516115146,
2.01076363117394,2.16135413764315,2.34266213672471,2.45637878572962,2.57527002969303),
 .UNSPECIFIED.);
#1005=B_SPLINE_CURVE_WITH_KNOTS('',3,(#23980,#23981,#23982,#23983,#23984,
#23985,#23986,#23987,#23988,#23989,#23990,#23991,#23992,#23993,#23994,#23995,
#23996,#23997,#23998,#23999,#24000,#24001,#24002,#24003,#24004,#24005,#24006,
#24007),.UNSPECIFIED.,.F.,.F.,(4,2,2,2,2,2,2,2,2,2,2,2,2,4),(9.99999999995091E-7,
0.0731124278961,0.166057761129691,0.286367941481508,0.413171684597363,0.536466369911867,
0.671513511997779,0.863012275276778,1.04829331747967,1.23237898344799,1.40408133486366,
1.58846641456439,1.74526991257199,1.84895017898734),.UNSPECIFIED.);
#1006=B_SPLINE_CURVE_WITH_KNOTS('',3,(#24009,#24010,#24011,#24012,#24013,
#24014,#24015,#24016,#24017,#24018,#24019,#24020),.UNSPECIFIED.,.F.,.F.,
(4,2,2,2,2,4),(1.0000001340625E-6,0.0596501394587982,0.121379110070747,
0.202618081237259,0.282064568204757,0.36296160107052),.UNSPECIFIED.);
#1007=B_SPLINE_CURVE_WITH_KNOTS('',3,(#24023,#24024,#24025,#24026,#24027,
#24028,#24029,#24030,#24031,#24032,#24033,#24034,#24035,#24036),
 .UNSPECIFIED.,.F.,.F.,(4,2,2,2,2,2,4),(1.84895017898734,1.87439516114959,
2.01076363117243,2.16135413765848,2.34266213680017,2.45637878583639,2.57527002983203),
 .UNSPECIFIED.);
#1008=B_SPLINE_CURVE_WITH_KNOTS('',3,(#24042,#24043,#24044,#24045,#24046,
#24047,#24048,#24049,#24050,#24051,#24052,#24053,#24054,#24055,#24056,#24057,
#24058,#24059,#24060,#24061,#24062,#24063,#24064,#24065,#24066,#24067,#24068,
#24069),.UNSPECIFIED.,.F.,.F.,(4,2,2,2,2,2,2,2,2,2,2,2,2,4),(9.99999999927736E-7,
0.0731124278938116,0.166057761124268,0.286367941476178,0.413171684591601,
0.536466369905737,0.671513511989027,0.863012275271149,1.04829331747739,
1.23237898344594,1.40408133486366,1.58846641456642,1.7452699125751,1.84895017900088),
 .UNSPECIFIED.);
#1009=B_SPLINE_CURVE_WITH_KNOTS('',3,(#24071,#24072,#24073,#24074,#24075,
#24076,#24077,#24078,#24079,#24080,#24081,#24082),.UNSPECIFIED.,.F.,.F.,
(4,2,2,2,2,4),(0.,0.0596482959180104,0.121377436598889,0.202616631617369,
0.282063337473005,0.362960593220025),.UNSPECIFIED.);
#1010=B_SPLINE_CURVE_WITH_KNOTS('',3,(#24085,#24086,#24087,#24088,#24089,
#24090,#24091,#24092,#24093,#24094,#24095,#24096,#24097,#24098),
 .UNSPECIFIED.,.F.,.F.,(4,2,2,2,2,2,4),(1.84895017900088,1.87439516115146,
2.01076363117394,2.16135413764315,2.34266213672471,2.45637878572962,2.57527002969303),
 .UNSPECIFIED.);
#1011=B_SPLINE_CURVE_WITH_KNOTS('',3,(#35684,#35685,#35686,#35687,#35688,
#35689,#35690,#35691,#35692,#35693,#35694,#35695,#35696,#35697,#35698,#35699,
#35700,#35701,#35702,#35703,#35704,#35705,#35706,#35707,#35708,#35709,#35710,
#35711,#35712,#35713,#35714,#35715,#35716,#35717),.UNSPECIFIED.,.T.,.F.,
(4,2,2,2,2,2,2,2,2,2,2,2,2,2,2,2,4),(0.,0.0567672348052759,0.113534469610552,
0.170293767345009,0.227053065079465,0.283812362813922,0.340571660548378,
0.397338895353654,0.45410613015893,0.510873364964206,0.567640599769482,
0.624399897503939,0.681159195238396,0.737918492972852,0.794677790707308,
0.851445025512584,0.908212260317861),.UNSPECIFIED.);
#1012=B_SPLINE_CURVE_WITH_KNOTS('',3,(#35720,#35721,#35722,#35723,#35724,
#35725,#35726,#35727,#35728,#35729,#35730,#35731,#35732,#35733,#35734,#35735,
#35736,#35737,#35738,#35739,#35740,#35741,#35742,#35743,#35744,#35745,#35746,
#35747,#35748,#35749,#35750,#35751,#35752,#35753),.UNSPECIFIED.,.T.,.F.,
(4,2,2,2,2,2,2,2,2,2,2,2,2,2,2,2,4),(-0.920290241966758,-0.862711406289492,
-0.805132570612226,-0.747675126043647,-0.690217681475069,-0.632760236906489,
-0.57530279233791,-0.517723956660645,-0.460145120983379,-0.402566285306113,
-0.344987449628848,-0.287530005060268,-0.23007256049169,-0.17261511592311,
-0.115157671354531,-0.0575788356772655,0.),.UNSPECIFIED.);
#1013=B_SPLINE_CURVE_WITH_KNOTS('',3,(#35757,#35758,#35759,#35760,#35761,
#35762,#35763,#35764,#35765,#35766),.UNSPECIFIED.,.F.,.F.,(4,2,2,2,4),(-0.230072560491689,
-0.17261511592311,-0.115157671354531,-0.0575788356772657,0.),
 .UNSPECIFIED.);
#1014=B_SPLINE_CURVE_WITH_KNOTS('',3,(#35768,#35769,#35770,#35771,#35772,
#35773,#35774,#35775,#35776,#35777,#35778,#35779,#35780,#35781,#35782,#35783,
#35784,#35785),.UNSPECIFIED.,.F.,.F.,(4,2,2,2,2,2,2,2,4),(-0.690217681475068,
-0.632760236906489,-0.57530279233791,-0.517723956660645,-0.460145120983379,
-0.402566285306113,-0.344987449628848,-0.287530005060269,-0.230072560491689),
 .UNSPECIFIED.);
#1015=B_SPLINE_CURVE_WITH_KNOTS('',3,(#35786,#35787,#35788,#35789,#35790,
#35791,#35792,#35793,#35794,#35795),.UNSPECIFIED.,.F.,.F.,(4,2,2,2,4),(0.,
0.0575788356772655,0.115157671354531,0.17261511592311,0.230072560491689),
 .UNSPECIFIED.);
#1016=B_SPLINE_CURVE_WITH_KNOTS('',3,(#35799,#35800,#35801,#35802,#35803,
#35804,#35805,#35806,#35807,#35808),.UNSPECIFIED.,.F.,.F.,(4,2,2,2,4),(0.681159195238395,
0.737918492972852,0.794677790707309,0.851445025512584,0.90821226031786),
 .UNSPECIFIED.);
#1017=B_SPLINE_CURVE_WITH_KNOTS('',3,(#35810,#35811,#35812,#35813,#35814,
#35815,#35816,#35817,#35818,#35819,#35820,#35821,#35822,#35823,#35824,#35825,
#35826,#35827),.UNSPECIFIED.,.F.,.F.,(4,2,2,2,2,2,2,2,4),(0.227053065079465,
0.283812362813922,0.340571660548378,0.397338895353654,0.45410613015893,
0.510873364964206,0.567640599769482,0.624399897503939,0.681159195238395),
 .UNSPECIFIED.);
#1018=B_SPLINE_CURVE_WITH_KNOTS('',3,(#35828,#35829,#35830,#35831,#35832,
#35833,#35834,#35835,#35836,#35837),.UNSPECIFIED.,.F.,.F.,(4,2,2,2,4),(0.90821226031786,
0.964979495123137,1.02174672992841,1.07850602766287,1.13526532539733),
 .UNSPECIFIED.);
#1019=TOROIDAL_SURFACE('',#11444,1.905,1.27);
#1020=TOROIDAL_SURFACE('',#11480,1.905,1.27);
#1021=TOROIDAL_SURFACE('',#11516,1.905,1.27);
#1022=TOROIDAL_SURFACE('',#11552,1.905,1.27);
#1023=TOROIDAL_SURFACE('',#11934,5.25,1.21175743903915);
#1024=TOROIDAL_SURFACE('',#11952,5.25,1.21175743903915);
#1025=TOROIDAL_SURFACE('',#11973,5.25,1.21175743903915);
#1026=TOROIDAL_SURFACE('',#12397,2.6505,0.2);
#1027=FACE_OUTER_BOUND('',#1641,.T.);
#1028=FACE_OUTER_BOUND('',#1642,.T.);
#1029=FACE_OUTER_BOUND('',#1643,.T.);
#1030=FACE_OUTER_BOUND('',#1644,.T.);
#1031=FACE_OUTER_BOUND('',#1645,.T.);
#1032=FACE_OUTER_BOUND('',#1646,.T.);
#1033=FACE_OUTER_BOUND('',#1647,.T.);
#1034=FACE_OUTER_BOUND('',#1648,.T.);
#1035=FACE_OUTER_BOUND('',#1649,.T.);
#1036=FACE_OUTER_BOUND('',#1650,.T.);
#1037=FACE_OUTER_BOUND('',#1651,.T.);
#1038=FACE_OUTER_BOUND('',#1652,.T.);
#1039=FACE_OUTER_BOUND('',#1653,.T.);
#1040=FACE_OUTER_BOUND('',#1654,.T.);
#1041=FACE_OUTER_BOUND('',#1655,.T.);
#1042=FACE_OUTER_BOUND('',#1656,.T.);
#1043=FACE_OUTER_BOUND('',#1657,.T.);
#1044=FACE_OUTER_BOUND('',#1658,.T.);
#1045=FACE_OUTER_BOUND('',#1659,.T.);
#1046=FACE_OUTER_BOUND('',#1660,.T.);
#1047=FACE_OUTER_BOUND('',#1661,.T.);
#1048=FACE_OUTER_BOUND('',#1662,.T.);
#1049=FACE_OUTER_BOUND('',#1663,.T.);
#1050=FACE_OUTER_BOUND('',#1664,.T.);
#1051=FACE_OUTER_BOUND('',#1665,.T.);
#1052=FACE_OUTER_BOUND('',#1666,.T.);
#1053=FACE_OUTER_BOUND('',#1667,.T.);
#1054=FACE_OUTER_BOUND('',#1668,.T.);
#1055=FACE_OUTER_BOUND('',#1669,.T.);
#1056=FACE_OUTER_BOUND('',#1670,.T.);
#1057=FACE_OUTER_BOUND('',#1671,.T.);
#1058=FACE_OUTER_BOUND('',#1672,.T.);
#1059=FACE_OUTER_BOUND('',#1673,.T.);
#1060=FACE_OUTER_BOUND('',#1674,.T.);
#1061=FACE_OUTER_BOUND('',#1675,.T.);
#1062=FACE_OUTER_BOUND('',#1676,.T.);
#1063=FACE_OUTER_BOUND('',#1677,.T.);
#1064=FACE_OUTER_BOUND('',#1678,.T.);
#1065=FACE_OUTER_BOUND('',#1679,.T.);
#1066=FACE_OUTER_BOUND('',#1680,.T.);
#1067=FACE_OUTER_BOUND('',#1681,.T.);
#1068=FACE_OUTER_BOUND('',#1682,.T.);
#1069=FACE_OUTER_BOUND('',#1683,.T.);
#1070=FACE_OUTER_BOUND('',#1684,.T.);
#1071=FACE_OUTER_BOUND('',#1685,.T.);
#1072=FACE_OUTER_BOUND('',#1686,.T.);
#1073=FACE_OUTER_BOUND('',#1687,.T.);
#1074=FACE_OUTER_BOUND('',#1688,.T.);
#1075=FACE_OUTER_BOUND('',#1689,.T.);
#1076=FACE_OUTER_BOUND('',#1690,.T.);
#1077=FACE_OUTER_BOUND('',#1691,.T.);
#1078=FACE_OUTER_BOUND('',#1692,.T.);
#1079=FACE_OUTER_BOUND('',#1693,.T.);
#1080=FACE_OUTER_BOUND('',#1694,.T.);
#1081=FACE_OUTER_BOUND('',#1695,.T.);
#1082=FACE_OUTER_BOUND('',#1696,.T.);
#1083=FACE_OUTER_BOUND('',#1697,.T.);
#1084=FACE_OUTER_BOUND('',#1698,.T.);
#1085=FACE_OUTER_BOUND('',#1699,.T.);
#1086=FACE_OUTER_BOUND('',#1700,.T.);
#1087=FACE_OUTER_BOUND('',#1701,.T.);
#1088=FACE_OUTER_BOUND('',#1702,.T.);
#1089=FACE_OUTER_BOUND('',#1703,.T.);
#1090=FACE_OUTER_BOUND('',#1704,.T.);
#1091=FACE_OUTER_BOUND('',#1705,.T.);
#1092=FACE_OUTER_BOUND('',#1706,.T.);
#1093=FACE_OUTER_BOUND('',#1707,.T.);
#1094=FACE_OUTER_BOUND('',#1708,.T.);
#1095=FACE_OUTER_BOUND('',#1709,.T.);
#1096=FACE_OUTER_BOUND('',#1710,.T.);
#1097=FACE_OUTER_BOUND('',#1711,.T.);
#1098=FACE_OUTER_BOUND('',#1712,.T.);
#1099=FACE_OUTER_BOUND('',#1713,.T.);
#1100=FACE_OUTER_BOUND('',#1714,.T.);
#1101=FACE_OUTER_BOUND('',#1715,.T.);
#1102=FACE_OUTER_BOUND('',#1716,.T.);
#1103=FACE_OUTER_BOUND('',#1717,.T.);
#1104=FACE_OUTER_BOUND('',#1718,.T.);
#1105=FACE_OUTER_BOUND('',#1719,.T.);
#1106=FACE_OUTER_BOUND('',#1720,.T.);
#1107=FACE_OUTER_BOUND('',#1721,.T.);
#1108=FACE_OUTER_BOUND('',#1722,.T.);
#1109=FACE_OUTER_BOUND('',#1723,.T.);
#1110=FACE_OUTER_BOUND('',#1724,.T.);
#1111=FACE_OUTER_BOUND('',#1725,.T.);
#1112=FACE_OUTER_BOUND('',#1726,.T.);
#1113=FACE_OUTER_BOUND('',#1727,.T.);
#1114=FACE_OUTER_BOUND('',#1728,.T.);
#1115=FACE_OUTER_BOUND('',#1729,.T.);
#1116=FACE_OUTER_BOUND('',#1730,.T.);
#1117=FACE_OUTER_BOUND('',#1731,.T.);
#1118=FACE_OUTER_BOUND('',#1732,.T.);
#1119=FACE_OUTER_BOUND('',#1733,.T.);
#1120=FACE_OUTER_BOUND('',#1734,.T.);
#1121=FACE_OUTER_BOUND('',#1735,.T.);
#1122=FACE_OUTER_BOUND('',#1736,.T.);
#1123=FACE_OUTER_BOUND('',#1737,.T.);
#1124=FACE_OUTER_BOUND('',#1738,.T.);
#1125=FACE_OUTER_BOUND('',#1739,.T.);
#1126=FACE_OUTER_BOUND('',#1740,.T.);
#1127=FACE_OUTER_BOUND('',#1741,.T.);
#1128=FACE_OUTER_BOUND('',#1742,.T.);
#1129=FACE_OUTER_BOUND('',#1743,.T.);
#1130=FACE_OUTER_BOUND('',#1744,.T.);
#1131=FACE_OUTER_BOUND('',#1745,.T.);
#1132=FACE_OUTER_BOUND('',#1746,.T.);
#1133=FACE_OUTER_BOUND('',#1747,.T.);
#1134=FACE_OUTER_BOUND('',#1748,.T.);
#1135=FACE_OUTER_BOUND('',#1749,.T.);
#1136=FACE_OUTER_BOUND('',#1750,.T.);
#1137=FACE_OUTER_BOUND('',#1751,.T.);
#1138=FACE_OUTER_BOUND('',#1752,.T.);
#1139=FACE_OUTER_BOUND('',#1753,.T.);
#1140=FACE_OUTER_BOUND('',#1754,.T.);
#1141=FACE_OUTER_BOUND('',#1755,.T.);
#1142=FACE_OUTER_BOUND('',#1756,.T.);
#1143=FACE_OUTER_BOUND('',#1757,.T.);
#1144=FACE_OUTER_BOUND('',#1758,.T.);
#1145=FACE_OUTER_BOUND('',#1759,.T.);
#1146=FACE_OUTER_BOUND('',#1760,.T.);
#1147=FACE_OUTER_BOUND('',#1761,.T.);
#1148=FACE_OUTER_BOUND('',#1762,.T.);
#1149=FACE_OUTER_BOUND('',#1763,.T.);
#1150=FACE_OUTER_BOUND('',#1764,.T.);
#1151=FACE_OUTER_BOUND('',#1765,.T.);
#1152=FACE_OUTER_BOUND('',#1766,.T.);
#1153=FACE_OUTER_BOUND('',#1767,.T.);
#1154=FACE_OUTER_BOUND('',#1768,.T.);
#1155=FACE_OUTER_BOUND('',#1769,.T.);
#1156=FACE_OUTER_BOUND('',#1770,.T.);
#1157=FACE_OUTER_BOUND('',#1771,.T.);
#1158=FACE_OUTER_BOUND('',#1772,.T.);
#1159=FACE_OUTER_BOUND('',#1773,.T.);
#1160=FACE_OUTER_BOUND('',#1774,.T.);
#1161=FACE_OUTER_BOUND('',#1775,.T.);
#1162=FACE_OUTER_BOUND('',#1776,.T.);
#1163=FACE_OUTER_BOUND('',#1777,.T.);
#1164=FACE_OUTER_BOUND('',#1778,.T.);
#1165=FACE_OUTER_BOUND('',#1779,.T.);
#1166=FACE_OUTER_BOUND('',#1780,.T.);
#1167=FACE_OUTER_BOUND('',#1781,.T.);
#1168=FACE_OUTER_BOUND('',#1782,.T.);
#1169=FACE_OUTER_BOUND('',#1783,.T.);
#1170=FACE_OUTER_BOUND('',#1784,.T.);
#1171=FACE_OUTER_BOUND('',#1785,.T.);
#1172=FACE_OUTER_BOUND('',#1786,.T.);
#1173=FACE_OUTER_BOUND('',#1787,.T.);
#1174=FACE_OUTER_BOUND('',#1788,.T.);
#1175=FACE_OUTER_BOUND('',#1789,.T.);
#1176=FACE_OUTER_BOUND('',#1790,.T.);
#1177=FACE_OUTER_BOUND('',#1791,.T.);
#1178=FACE_OUTER_BOUND('',#1792,.T.);
#1179=FACE_OUTER_BOUND('',#1793,.T.);
#1180=FACE_OUTER_BOUND('',#1794,.T.);
#1181=FACE_OUTER_BOUND('',#1795,.T.);
#1182=FACE_OUTER_BOUND('',#1796,.T.);
#1183=FACE_OUTER_BOUND('',#1797,.T.);
#1184=FACE_OUTER_BOUND('',#1798,.T.);
#1185=FACE_OUTER_BOUND('',#1799,.T.);
#1186=FACE_OUTER_BOUND('',#1800,.T.);
#1187=FACE_OUTER_BOUND('',#1801,.T.);
#1188=FACE_OUTER_BOUND('',#1802,.T.);
#1189=FACE_OUTER_BOUND('',#1803,.T.);
#1190=FACE_OUTER_BOUND('',#1804,.T.);
#1191=FACE_OUTER_BOUND('',#1805,.T.);
#1192=FACE_OUTER_BOUND('',#1806,.T.);
#1193=FACE_OUTER_BOUND('',#1807,.T.);
#1194=FACE_OUTER_BOUND('',#1808,.T.);
#1195=FACE_OUTER_BOUND('',#1809,.T.);
#1196=FACE_OUTER_BOUND('',#1810,.T.);
#1197=FACE_OUTER_BOUND('',#1811,.T.);
#1198=FACE_OUTER_BOUND('',#1812,.T.);
#1199=FACE_OUTER_BOUND('',#1813,.T.);
#1200=FACE_OUTER_BOUND('',#1814,.T.);
#1201=FACE_OUTER_BOUND('',#1815,.T.);
#1202=FACE_OUTER_BOUND('',#1816,.T.);
#1203=FACE_OUTER_BOUND('',#1817,.T.);
#1204=FACE_OUTER_BOUND('',#1818,.T.);
#1205=FACE_OUTER_BOUND('',#1819,.T.);
#1206=FACE_OUTER_BOUND('',#1820,.T.);
#1207=FACE_OUTER_BOUND('',#1821,.T.);
#1208=FACE_OUTER_BOUND('',#1822,.T.);
#1209=FACE_OUTER_BOUND('',#1823,.T.);
#1210=FACE_OUTER_BOUND('',#1824,.T.);
#1211=FACE_OUTER_BOUND('',#1825,.T.);
#1212=FACE_OUTER_BOUND('',#1826,.T.);
#1213=FACE_OUTER_BOUND('',#1827,.T.);
#1214=FACE_OUTER_BOUND('',#1828,.T.);
#1215=FACE_OUTER_BOUND('',#1829,.T.);
#1216=FACE_OUTER_BOUND('',#1830,.T.);
#1217=FACE_OUTER_BOUND('',#1831,.T.);
#1218=FACE_OUTER_BOUND('',#1832,.T.);
#1219=FACE_OUTER_BOUND('',#1833,.T.);
#1220=FACE_OUTER_BOUND('',#1834,.T.);
#1221=FACE_OUTER_BOUND('',#1835,.T.);
#1222=FACE_OUTER_BOUND('',#1836,.T.);
#1223=FACE_OUTER_BOUND('',#1837,.T.);
#1224=FACE_OUTER_BOUND('',#1838,.T.);
#1225=FACE_OUTER_BOUND('',#1839,.T.);
#1226=FACE_OUTER_BOUND('',#1840,.T.);
#1227=FACE_OUTER_BOUND('',#1841,.T.);
#1228=FACE_OUTER_BOUND('',#1842,.T.);
#1229=FACE_OUTER_BOUND('',#1843,.T.);
#1230=FACE_OUTER_BOUND('',#1844,.T.);
#1231=FACE_OUTER_BOUND('',#1850,.T.);
#1232=FACE_OUTER_BOUND('',#1851,.T.);
#1233=FACE_OUTER_BOUND('',#1852,.T.);
#1234=FACE_OUTER_BOUND('',#1853,.T.);
#1235=FACE_OUTER_BOUND('',#1854,.T.);
#1236=FACE_OUTER_BOUND('',#1855,.T.);
#1237=FACE_OUTER_BOUND('',#1856,.T.);
#1238=FACE_OUTER_BOUND('',#1857,.T.);
#1239=FACE_OUTER_BOUND('',#1858,.T.);
#1240=FACE_OUTER_BOUND('',#1859,.T.);
#1241=FACE_OUTER_BOUND('',#1860,.T.);
#1242=FACE_OUTER_BOUND('',#1861,.T.);
#1243=FACE_OUTER_BOUND('',#1862,.T.);
#1244=FACE_OUTER_BOUND('',#1864,.T.);
#1245=FACE_OUTER_BOUND('',#1866,.T.);
#1246=FACE_OUTER_BOUND('',#1867,.T.);
#1247=FACE_OUTER_BOUND('',#1868,.T.);
#1248=FACE_OUTER_BOUND('',#1869,.T.);
#1249=FACE_OUTER_BOUND('',#1870,.T.);
#1250=FACE_OUTER_BOUND('',#1871,.T.);
#1251=FACE_OUTER_BOUND('',#1872,.T.);
#1252=FACE_OUTER_BOUND('',#1873,.T.);
#1253=FACE_OUTER_BOUND('',#1874,.T.);
#1254=FACE_OUTER_BOUND('',#1875,.T.);
#1255=FACE_OUTER_BOUND('',#1876,.T.);
#1256=FACE_OUTER_BOUND('',#1877,.T.);
#1257=FACE_OUTER_BOUND('',#1878,.T.);
#1258=FACE_OUTER_BOUND('',#1879,.T.);
#1259=FACE_OUTER_BOUND('',#1880,.T.);
#1260=FACE_OUTER_BOUND('',#1881,.T.);
#1261=FACE_OUTER_BOUND('',#1882,.T.);
#1262=FACE_OUTER_BOUND('',#1888,.T.);
#1263=FACE_OUTER_BOUND('',#1889,.T.);
#1264=FACE_OUTER_BOUND('',#1890,.T.);
#1265=FACE_OUTER_BOUND('',#1891,.T.);
#1266=FACE_OUTER_BOUND('',#1892,.T.);
#1267=FACE_OUTER_BOUND('',#1894,.T.);
#1268=FACE_OUTER_BOUND('',#1895,.T.);
#1269=FACE_OUTER_BOUND('',#1896,.T.);
#1270=FACE_OUTER_BOUND('',#1897,.T.);
#1271=FACE_OUTER_BOUND('',#1898,.T.);
#1272=FACE_OUTER_BOUND('',#1899,.T.);
#1273=FACE_OUTER_BOUND('',#1900,.T.);
#1274=FACE_OUTER_BOUND('',#1901,.T.);
#1275=FACE_OUTER_BOUND('',#1902,.T.);
#1276=FACE_OUTER_BOUND('',#1903,.T.);
#1277=FACE_OUTER_BOUND('',#1904,.T.);
#1278=FACE_OUTER_BOUND('',#1905,.T.);
#1279=FACE_OUTER_BOUND('',#1906,.T.);
#1280=FACE_OUTER_BOUND('',#1907,.T.);
#1281=FACE_OUTER_BOUND('',#1908,.T.);
#1282=FACE_OUTER_BOUND('',#1909,.T.);
#1283=FACE_OUTER_BOUND('',#1910,.T.);
#1284=FACE_OUTER_BOUND('',#1911,.T.);
#1285=FACE_OUTER_BOUND('',#1912,.T.);
#1286=FACE_OUTER_BOUND('',#1913,.T.);
#1287=FACE_OUTER_BOUND('',#1914,.T.);
#1288=FACE_OUTER_BOUND('',#1915,.T.);
#1289=FACE_OUTER_BOUND('',#1916,.T.);
#1290=FACE_OUTER_BOUND('',#1918,.T.);
#1291=FACE_OUTER_BOUND('',#1919,.T.);
#1292=FACE_OUTER_BOUND('',#1925,.T.);
#1293=FACE_OUTER_BOUND('',#1926,.T.);
#1294=FACE_OUTER_BOUND('',#1927,.T.);
#1295=FACE_OUTER_BOUND('',#1928,.T.);
#1296=FACE_OUTER_BOUND('',#1929,.T.);
#1297=FACE_OUTER_BOUND('',#1930,.T.);
#1298=FACE_OUTER_BOUND('',#1931,.T.);
#1299=FACE_OUTER_BOUND('',#1932,.T.);
#1300=FACE_OUTER_BOUND('',#1933,.T.);
#1301=FACE_OUTER_BOUND('',#1934,.T.);
#1302=FACE_OUTER_BOUND('',#1935,.T.);
#1303=FACE_OUTER_BOUND('',#1936,.T.);
#1304=FACE_OUTER_BOUND('',#1937,.T.);
#1305=FACE_OUTER_BOUND('',#1938,.T.);
#1306=FACE_OUTER_BOUND('',#1939,.T.);
#1307=FACE_OUTER_BOUND('',#1940,.T.);
#1308=FACE_OUTER_BOUND('',#1941,.T.);
#1309=FACE_OUTER_BOUND('',#1942,.T.);
#1310=FACE_OUTER_BOUND('',#1943,.T.);
#1311=FACE_OUTER_BOUND('',#1944,.T.);
#1312=FACE_OUTER_BOUND('',#1946,.T.);
#1313=FACE_OUTER_BOUND('',#1948,.T.);
#1314=FACE_OUTER_BOUND('',#1949,.T.);
#1315=FACE_OUTER_BOUND('',#1950,.T.);
#1316=FACE_OUTER_BOUND('',#1951,.T.);
#1317=FACE_OUTER_BOUND('',#1952,.T.);
#1318=FACE_OUTER_BOUND('',#1953,.T.);
#1319=FACE_OUTER_BOUND('',#1955,.T.);
#1320=FACE_OUTER_BOUND('',#1961,.T.);
#1321=FACE_OUTER_BOUND('',#1962,.T.);
#1322=FACE_OUTER_BOUND('',#1963,.T.);
#1323=FACE_OUTER_BOUND('',#1964,.T.);
#1324=FACE_OUTER_BOUND('',#1965,.T.);
#1325=FACE_OUTER_BOUND('',#1966,.T.);
#1326=FACE_OUTER_BOUND('',#1967,.T.);
#1327=FACE_OUTER_BOUND('',#1968,.T.);
#1328=FACE_OUTER_BOUND('',#1969,.T.);
#1329=FACE_OUTER_BOUND('',#1970,.T.);
#1330=FACE_OUTER_BOUND('',#1971,.T.);
#1331=FACE_OUTER_BOUND('',#1972,.T.);
#1332=FACE_OUTER_BOUND('',#1973,.T.);
#1333=FACE_OUTER_BOUND('',#1974,.T.);
#1334=FACE_OUTER_BOUND('',#1975,.T.);
#1335=FACE_OUTER_BOUND('',#1977,.T.);
#1336=FACE_OUTER_BOUND('',#1978,.T.);
#1337=FACE_OUTER_BOUND('',#1980,.T.);
#1338=FACE_OUTER_BOUND('',#1981,.T.);
#1339=FACE_OUTER_BOUND('',#1982,.T.);
#1340=FACE_OUTER_BOUND('',#1983,.T.);
#1341=FACE_OUTER_BOUND('',#1985,.T.);
#1342=FACE_OUTER_BOUND('',#1987,.T.);
#1343=FACE_OUTER_BOUND('',#1988,.T.);
#1344=FACE_OUTER_BOUND('',#1989,.T.);
#1345=FACE_OUTER_BOUND('',#1990,.T.);
#1346=FACE_OUTER_BOUND('',#1991,.T.);
#1347=FACE_OUTER_BOUND('',#1992,.T.);
#1348=FACE_OUTER_BOUND('',#1993,.T.);
#1349=FACE_OUTER_BOUND('',#1994,.T.);
#1350=FACE_OUTER_BOUND('',#1995,.T.);
#1351=FACE_OUTER_BOUND('',#1996,.T.);
#1352=FACE_OUTER_BOUND('',#1998,.T.);
#1353=FACE_OUTER_BOUND('',#1999,.T.);
#1354=FACE_OUTER_BOUND('',#2001,.T.);
#1355=FACE_OUTER_BOUND('',#2002,.T.);
#1356=FACE_OUTER_BOUND('',#2003,.T.);
#1357=FACE_OUTER_BOUND('',#2004,.T.);
#1358=FACE_OUTER_BOUND('',#2005,.T.);
#1359=FACE_OUTER_BOUND('',#2006,.T.);
#1360=FACE_OUTER_BOUND('',#2007,.T.);
#1361=FACE_OUTER_BOUND('',#2008,.T.);
#1362=FACE_OUTER_BOUND('',#2010,.T.);
#1363=FACE_OUTER_BOUND('',#2012,.T.);
#1364=FACE_OUTER_BOUND('',#2013,.T.);
#1365=FACE_OUTER_BOUND('',#2014,.T.);
#1366=FACE_OUTER_BOUND('',#2015,.T.);
#1367=FACE_OUTER_BOUND('',#2016,.T.);
#1368=FACE_OUTER_BOUND('',#2018,.T.);
#1369=FACE_OUTER_BOUND('',#2020,.T.);
#1370=FACE_OUTER_BOUND('',#2021,.T.);
#1371=FACE_OUTER_BOUND('',#2022,.T.);
#1372=FACE_OUTER_BOUND('',#2023,.T.);
#1373=FACE_OUTER_BOUND('',#2024,.T.);
#1374=FACE_OUTER_BOUND('',#2025,.T.);
#1375=FACE_OUTER_BOUND('',#2026,.T.);
#1376=FACE_OUTER_BOUND('',#2027,.T.);
#1377=FACE_OUTER_BOUND('',#2029,.T.);
#1378=FACE_OUTER_BOUND('',#2031,.T.);
#1379=FACE_OUTER_BOUND('',#2033,.T.);
#1380=FACE_OUTER_BOUND('',#2034,.T.);
#1381=FACE_OUTER_BOUND('',#2035,.T.);
#1382=FACE_OUTER_BOUND('',#2036,.T.);
#1383=FACE_OUTER_BOUND('',#2037,.T.);
#1384=FACE_OUTER_BOUND('',#2038,.T.);
#1385=FACE_OUTER_BOUND('',#2039,.T.);
#1386=FACE_OUTER_BOUND('',#2040,.T.);
#1387=FACE_OUTER_BOUND('',#2041,.T.);
#1388=FACE_OUTER_BOUND('',#2042,.T.);
#1389=FACE_OUTER_BOUND('',#2043,.T.);
#1390=FACE_OUTER_BOUND('',#2044,.T.);
#1391=FACE_OUTER_BOUND('',#2045,.T.);
#1392=FACE_OUTER_BOUND('',#2046,.T.);
#1393=FACE_OUTER_BOUND('',#2047,.T.);
#1394=FACE_OUTER_BOUND('',#2048,.T.);
#1395=FACE_OUTER_BOUND('',#2049,.T.);
#1396=FACE_OUTER_BOUND('',#2050,.T.);
#1397=FACE_OUTER_BOUND('',#2051,.T.);
#1398=FACE_OUTER_BOUND('',#2052,.T.);
#1399=FACE_OUTER_BOUND('',#2053,.T.);
#1400=FACE_OUTER_BOUND('',#2054,.T.);
#1401=FACE_OUTER_BOUND('',#2055,.T.);
#1402=FACE_OUTER_BOUND('',#2056,.T.);
#1403=FACE_OUTER_BOUND('',#2057,.T.);
#1404=FACE_OUTER_BOUND('',#2058,.T.);
#1405=FACE_OUTER_BOUND('',#2059,.T.);
#1406=FACE_OUTER_BOUND('',#2060,.T.);
#1407=FACE_OUTER_BOUND('',#2061,.T.);
#1408=FACE_OUTER_BOUND('',#2062,.T.);
#1409=FACE_OUTER_BOUND('',#2063,.T.);
#1410=FACE_OUTER_BOUND('',#2064,.T.);
#1411=FACE_OUTER_BOUND('',#2065,.T.);
#1412=FACE_OUTER_BOUND('',#2066,.T.);
#1413=FACE_OUTER_BOUND('',#2067,.T.);
#1414=FACE_OUTER_BOUND('',#2068,.T.);
#1415=FACE_OUTER_BOUND('',#2069,.T.);
#1416=FACE_OUTER_BOUND('',#2070,.T.);
#1417=FACE_OUTER_BOUND('',#2071,.T.);
#1418=FACE_OUTER_BOUND('',#2072,.T.);
#1419=FACE_OUTER_BOUND('',#2073,.T.);
#1420=FACE_OUTER_BOUND('',#2074,.T.);
#1421=FACE_OUTER_BOUND('',#2075,.T.);
#1422=FACE_OUTER_BOUND('',#2076,.T.);
#1423=FACE_OUTER_BOUND('',#2077,.T.);
#1424=FACE_OUTER_BOUND('',#2078,.T.);
#1425=FACE_OUTER_BOUND('',#2079,.T.);
#1426=FACE_OUTER_BOUND('',#2080,.T.);
#1427=FACE_OUTER_BOUND('',#2081,.T.);
#1428=FACE_OUTER_BOUND('',#2082,.T.);
#1429=FACE_OUTER_BOUND('',#2083,.T.);
#1430=FACE_OUTER_BOUND('',#2084,.T.);
#1431=FACE_OUTER_BOUND('',#2085,.T.);
#1432=FACE_OUTER_BOUND('',#2086,.T.);
#1433=FACE_OUTER_BOUND('',#2087,.T.);
#1434=FACE_OUTER_BOUND('',#2088,.T.);
#1435=FACE_OUTER_BOUND('',#2089,.T.);
#1436=FACE_OUTER_BOUND('',#2090,.T.);
#1437=FACE_OUTER_BOUND('',#2094,.T.);
#1438=FACE_OUTER_BOUND('',#2095,.T.);
#1439=FACE_OUTER_BOUND('',#2096,.T.);
#1440=FACE_OUTER_BOUND('',#2097,.T.);
#1441=FACE_OUTER_BOUND('',#2098,.T.);
#1442=FACE_OUTER_BOUND('',#2099,.T.);
#1443=FACE_OUTER_BOUND('',#2100,.T.);
#1444=FACE_OUTER_BOUND('',#2101,.T.);
#1445=FACE_OUTER_BOUND('',#2102,.T.);
#1446=FACE_OUTER_BOUND('',#2103,.T.);
#1447=FACE_OUTER_BOUND('',#2104,.T.);
#1448=FACE_OUTER_BOUND('',#2105,.T.);
#1449=FACE_OUTER_BOUND('',#2106,.T.);
#1450=FACE_OUTER_BOUND('',#2107,.T.);
#1451=FACE_OUTER_BOUND('',#2108,.T.);
#1452=FACE_OUTER_BOUND('',#2109,.T.);
#1453=FACE_OUTER_BOUND('',#2110,.T.);
#1454=FACE_OUTER_BOUND('',#2111,.T.);
#1455=FACE_OUTER_BOUND('',#2112,.T.);
#1456=FACE_OUTER_BOUND('',#2113,.T.);
#1457=FACE_OUTER_BOUND('',#2114,.T.);
#1458=FACE_OUTER_BOUND('',#2115,.T.);
#1459=FACE_OUTER_BOUND('',#2116,.T.);
#1460=FACE_OUTER_BOUND('',#2117,.T.);
#1461=FACE_OUTER_BOUND('',#2118,.T.);
#1462=FACE_OUTER_BOUND('',#2119,.T.);
#1463=FACE_OUTER_BOUND('',#2120,.T.);
#1464=FACE_OUTER_BOUND('',#2121,.T.);
#1465=FACE_OUTER_BOUND('',#2122,.T.);
#1466=FACE_OUTER_BOUND('',#2123,.T.);
#1467=FACE_OUTER_BOUND('',#2124,.T.);
#1468=FACE_OUTER_BOUND('',#2125,.T.);
#1469=FACE_OUTER_BOUND('',#2126,.T.);
#1470=FACE_OUTER_BOUND('',#2127,.T.);
#1471=FACE_OUTER_BOUND('',#2128,.T.);
#1472=FACE_OUTER_BOUND('',#2129,.T.);
#1473=FACE_OUTER_BOUND('',#2130,.T.);
#1474=FACE_OUTER_BOUND('',#2131,.T.);
#1475=FACE_OUTER_BOUND('',#2132,.T.);
#1476=FACE_OUTER_BOUND('',#2133,.T.);
#1477=FACE_OUTER_BOUND('',#2134,.T.);
#1478=FACE_OUTER_BOUND('',#2135,.T.);
#1479=FACE_OUTER_BOUND('',#2136,.T.);
#1480=FACE_OUTER_BOUND('',#2137,.T.);
#1481=FACE_OUTER_BOUND('',#2138,.T.);
#1482=FACE_OUTER_BOUND('',#2139,.T.);
#1483=FACE_OUTER_BOUND('',#2140,.T.);
#1484=FACE_OUTER_BOUND('',#2141,.T.);
#1485=FACE_OUTER_BOUND('',#2145,.T.);
#1486=FACE_OUTER_BOUND('',#2147,.T.);
#1487=FACE_OUTER_BOUND('',#2148,.T.);
#1488=FACE_OUTER_BOUND('',#2150,.T.);
#1489=FACE_OUTER_BOUND('',#2152,.T.);
#1490=FACE_OUTER_BOUND('',#2153,.T.);
#1491=FACE_OUTER_BOUND('',#2154,.T.);
#1492=FACE_OUTER_BOUND('',#2156,.T.);
#1493=FACE_OUTER_BOUND('',#2157,.T.);
#1494=FACE_OUTER_BOUND('',#2158,.T.);
#1495=FACE_OUTER_BOUND('',#2159,.T.);
#1496=FACE_OUTER_BOUND('',#2160,.T.);
#1497=FACE_OUTER_BOUND('',#2161,.T.);
#1498=FACE_OUTER_BOUND('',#2162,.T.);
#1499=FACE_OUTER_BOUND('',#2163,.T.);
#1500=FACE_OUTER_BOUND('',#2164,.T.);
#1501=FACE_OUTER_BOUND('',#2165,.T.);
#1502=FACE_OUTER_BOUND('',#2166,.T.);
#1503=FACE_OUTER_BOUND('',#2167,.T.);
#1504=FACE_OUTER_BOUND('',#2168,.T.);
#1505=FACE_OUTER_BOUND('',#2169,.T.);
#1506=FACE_OUTER_BOUND('',#2170,.T.);
#1507=FACE_OUTER_BOUND('',#2171,.T.);
#1508=FACE_OUTER_BOUND('',#2172,.T.);
#1509=FACE_OUTER_BOUND('',#2173,.T.);
#1510=FACE_OUTER_BOUND('',#2174,.T.);
#1511=FACE_OUTER_BOUND('',#2175,.T.);
#1512=FACE_OUTER_BOUND('',#2176,.T.);
#1513=FACE_OUTER_BOUND('',#2177,.T.);
#1514=FACE_OUTER_BOUND('',#2178,.T.);
#1515=FACE_OUTER_BOUND('',#2179,.T.);
#1516=FACE_OUTER_BOUND('',#2180,.T.);
#1517=FACE_OUTER_BOUND('',#2181,.T.);
#1518=FACE_OUTER_BOUND('',#2182,.T.);
#1519=FACE_OUTER_BOUND('',#2183,.T.);
#1520=FACE_OUTER_BOUND('',#2184,.T.);
#1521=FACE_OUTER_BOUND('',#2185,.T.);
#1522=FACE_OUTER_BOUND('',#2186,.T.);
#1523=FACE_OUTER_BOUND('',#2187,.T.);
#1524=FACE_OUTER_BOUND('',#2188,.T.);
#1525=FACE_OUTER_BOUND('',#2189,.T.);
#1526=FACE_OUTER_BOUND('',#2190,.T.);
#1527=FACE_OUTER_BOUND('',#2199,.T.);
#1528=FACE_OUTER_BOUND('',#2208,.T.);
#1529=FACE_OUTER_BOUND('',#2209,.T.);
#1530=FACE_OUTER_BOUND('',#2210,.T.);
#1531=FACE_OUTER_BOUND('',#2212,.T.);
#1532=FACE_OUTER_BOUND('',#2214,.T.);
#1533=FACE_OUTER_BOUND('',#2216,.T.);
#1534=FACE_OUTER_BOUND('',#2217,.T.);
#1535=FACE_OUTER_BOUND('',#2219,.T.);
#1536=FACE_OUTER_BOUND('',#2220,.T.);
#1537=FACE_OUTER_BOUND('',#2222,.T.);
#1538=FACE_OUTER_BOUND('',#2223,.T.);
#1539=FACE_OUTER_BOUND('',#2225,.T.);
#1540=FACE_OUTER_BOUND('',#2227,.T.);
#1541=FACE_OUTER_BOUND('',#2229,.T.);
#1542=FACE_OUTER_BOUND('',#2230,.T.);
#1543=FACE_OUTER_BOUND('',#2231,.T.);
#1544=FACE_OUTER_BOUND('',#2232,.T.);
#1545=FACE_OUTER_BOUND('',#2233,.T.);
#1546=FACE_OUTER_BOUND('',#2234,.T.);
#1547=FACE_OUTER_BOUND('',#2235,.T.);
#1548=FACE_OUTER_BOUND('',#2236,.T.);
#1549=FACE_OUTER_BOUND('',#2237,.T.);
#1550=FACE_OUTER_BOUND('',#2239,.T.);
#1551=FACE_OUTER_BOUND('',#2240,.T.);
#1552=FACE_OUTER_BOUND('',#2241,.T.);
#1553=FACE_OUTER_BOUND('',#2242,.T.);
#1554=FACE_OUTER_BOUND('',#2243,.T.);
#1555=FACE_OUTER_BOUND('',#2244,.T.);
#1556=FACE_OUTER_BOUND('',#2245,.T.);
#1557=FACE_OUTER_BOUND('',#2246,.T.);
#1558=FACE_OUTER_BOUND('',#2247,.T.);
#1559=FACE_OUTER_BOUND('',#2248,.T.);
#1560=FACE_OUTER_BOUND('',#2249,.T.);
#1561=FACE_OUTER_BOUND('',#2250,.T.);
#1562=FACE_OUTER_BOUND('',#2251,.T.);
#1563=FACE_OUTER_BOUND('',#2252,.T.);
#1564=FACE_OUTER_BOUND('',#2253,.T.);
#1565=FACE_OUTER_BOUND('',#2254,.T.);
#1566=FACE_OUTER_BOUND('',#2255,.T.);
#1567=FACE_OUTER_BOUND('',#2256,.T.);
#1568=FACE_OUTER_BOUND('',#2257,.T.);
#1569=FACE_OUTER_BOUND('',#2258,.T.);
#1570=FACE_OUTER_BOUND('',#2259,.T.);
#1571=FACE_OUTER_BOUND('',#2260,.T.);
#1572=FACE_OUTER_BOUND('',#2261,.T.);
#1573=FACE_OUTER_BOUND('',#2262,.T.);
#1574=FACE_OUTER_BOUND('',#2263,.T.);
#1575=FACE_OUTER_BOUND('',#2264,.T.);
#1576=FACE_OUTER_BOUND('',#2265,.T.);
#1577=FACE_OUTER_BOUND('',#2266,.T.);
#1578=FACE_OUTER_BOUND('',#2267,.T.);
#1579=FACE_OUTER_BOUND('',#2268,.T.);
#1580=FACE_OUTER_BOUND('',#2269,.T.);
#1581=FACE_OUTER_BOUND('',#2270,.T.);
#1582=FACE_OUTER_BOUND('',#2271,.T.);
#1583=FACE_OUTER_BOUND('',#2272,.T.);
#1584=FACE_OUTER_BOUND('',#2273,.T.);
#1585=FACE_OUTER_BOUND('',#2274,.T.);
#1586=FACE_OUTER_BOUND('',#2275,.T.);
#1587=FACE_OUTER_BOUND('',#2276,.T.);
#1588=FACE_OUTER_BOUND('',#2277,.T.);
#1589=FACE_OUTER_BOUND('',#2278,.T.);
#1590=FACE_OUTER_BOUND('',#2279,.T.);
#1591=FACE_OUTER_BOUND('',#2280,.T.);
#1592=FACE_OUTER_BOUND('',#2281,.T.);
#1593=FACE_OUTER_BOUND('',#2282,.T.);
#1594=FACE_OUTER_BOUND('',#2283,.T.);
#1595=FACE_OUTER_BOUND('',#2284,.T.);
#1596=FACE_OUTER_BOUND('',#2285,.T.);
#1597=FACE_OUTER_BOUND('',#2286,.T.);
#1598=FACE_OUTER_BOUND('',#2287,.T.);
#1599=FACE_OUTER_BOUND('',#2288,.T.);
#1600=FACE_OUTER_BOUND('',#2289,.T.);
#1601=FACE_OUTER_BOUND('',#2290,.T.);
#1602=FACE_OUTER_BOUND('',#2291,.T.);
#1603=FACE_OUTER_BOUND('',#2292,.T.);
#1604=FACE_OUTER_BOUND('',#2293,.T.);
#1605=FACE_OUTER_BOUND('',#2294,.T.);
#1606=FACE_OUTER_BOUND('',#2318,.T.);
#1607=FACE_OUTER_BOUND('',#2342,.T.);
#1608=FACE_OUTER_BOUND('',#2343,.T.);
#1609=FACE_OUTER_BOUND('',#2344,.T.);
#1610=FACE_OUTER_BOUND('',#2345,.T.);
#1611=FACE_OUTER_BOUND('',#2346,.T.);
#1612=FACE_OUTER_BOUND('',#2347,.T.);
#1613=FACE_OUTER_BOUND('',#2348,.T.);
#1614=FACE_OUTER_BOUND('',#2349,.T.);
#1615=FACE_OUTER_BOUND('',#2350,.T.);
#1616=FACE_OUTER_BOUND('',#2351,.T.);
#1617=FACE_OUTER_BOUND('',#2352,.T.);
#1618=FACE_OUTER_BOUND('',#2353,.T.);
#1619=FACE_OUTER_BOUND('',#2354,.T.);
#1620=FACE_OUTER_BOUND('',#2355,.T.);
#1621=FACE_OUTER_BOUND('',#2361,.T.);
#1622=FACE_OUTER_BOUND('',#2367,.T.);
#1623=FACE_OUTER_BOUND('',#2368,.T.);
#1624=FACE_OUTER_BOUND('',#2369,.T.);
#1625=FACE_OUTER_BOUND('',#2371,.T.);
#1626=FACE_OUTER_BOUND('',#2372,.T.);
#1627=FACE_OUTER_BOUND('',#2373,.T.);
#1628=FACE_OUTER_BOUND('',#2374,.T.);
#1629=FACE_OUTER_BOUND('',#2375,.T.);
#1630=FACE_OUTER_BOUND('',#2376,.T.);
#1631=FACE_OUTER_BOUND('',#2377,.T.);
#1632=FACE_OUTER_BOUND('',#2378,.T.);
#1633=FACE_OUTER_BOUND('',#2379,.T.);
#1634=FACE_OUTER_BOUND('',#2380,.T.);
#1635=FACE_OUTER_BOUND('',#2381,.T.);
#1636=FACE_OUTER_BOUND('',#2382,.T.);
#1637=FACE_OUTER_BOUND('',#2383,.T.);
#1638=FACE_OUTER_BOUND('',#2384,.T.);
#1639=FACE_OUTER_BOUND('',#2385,.T.);
#1640=FACE_OUTER_BOUND('',#2387,.T.);
#1641=EDGE_LOOP('',(#7238,#7239,#7240,#7241,#7242));
#1642=EDGE_LOOP('',(#7243,#7244,#7245,#7246,#7247,#7248,#7249,#7250,#7251,
#7252,#7253,#7254,#7255,#7256,#7257,#7258,#7259,#7260,#7261,#7262,#7263));
#1643=EDGE_LOOP('',(#7264,#7265,#7266));
#1644=EDGE_LOOP('',(#7267,#7268,#7269));
#1645=EDGE_LOOP('',(#7270,#7271,#7272));
#1646=EDGE_LOOP('',(#7273));
#1647=EDGE_LOOP('',(#7274,#7275,#7276));
#1648=EDGE_LOOP('',(#7277,#7278,#7279,#7280,#7281));
#1649=EDGE_LOOP('',(#7282,#7283,#7284,#7285,#7286));
#1650=EDGE_LOOP('',(#7287,#7288,#7289,#7290,#7291));
#1651=EDGE_LOOP('',(#7292,#7293,#7294,#7295));
#1652=EDGE_LOOP('',(#7296,#7297,#7298,#7299,#7300));
#1653=EDGE_LOOP('',(#7301,#7302,#7303,#7304));
#1654=EDGE_LOOP('',(#7305,#7306,#7307,#7308,#7309,#7310,#7311,#7312,#7313,
#7314,#7315,#7316));
#1655=EDGE_LOOP('',(#7317,#7318,#7319,#7320));
#1656=EDGE_LOOP('',(#7321,#7322,#7323,#7324,#7325));
#1657=EDGE_LOOP('',(#7326,#7327,#7328,#7329,#7330));
#1658=EDGE_LOOP('',(#7331,#7332,#7333,#7334,#7335));
#1659=EDGE_LOOP('',(#7336,#7337,#7338,#7339,#7340));
#1660=EDGE_LOOP('',(#7341,#7342,#7343,#7344,#7345));
#1661=EDGE_LOOP('',(#7346,#7347,#7348,#7349,#7350));
#1662=EDGE_LOOP('',(#7351,#7352,#7353,#7354,#7355,#7356,#7357,#7358,#7359,
#7360,#7361,#7362,#7363,#7364,#7365,#7366,#7367,#7368,#7369,#7370,#7371));
#1663=EDGE_LOOP('',(#7372,#7373,#7374));
#1664=EDGE_LOOP('',(#7375,#7376,#7377));
#1665=EDGE_LOOP('',(#7378,#7379,#7380));
#1666=EDGE_LOOP('',(#7381));
#1667=EDGE_LOOP('',(#7382,#7383,#7384));
#1668=EDGE_LOOP('',(#7385,#7386,#7387,#7388,#7389));
#1669=EDGE_LOOP('',(#7390,#7391,#7392,#7393,#7394));
#1670=EDGE_LOOP('',(#7395,#7396,#7397,#7398,#7399));
#1671=EDGE_LOOP('',(#7400,#7401,#7402,#7403));
#1672=EDGE_LOOP('',(#7404,#7405,#7406,#7407,#7408));
#1673=EDGE_LOOP('',(#7409,#7410,#7411,#7412));
#1674=EDGE_LOOP('',(#7413,#7414,#7415,#7416,#7417,#7418,#7419,#7420,#7421,
#7422,#7423,#7424));
#1675=EDGE_LOOP('',(#7425,#7426,#7427,#7428));
#1676=EDGE_LOOP('',(#7429,#7430,#7431,#7432,#7433));
#1677=EDGE_LOOP('',(#7434,#7435,#7436,#7437,#7438));
#1678=EDGE_LOOP('',(#7439,#7440,#7441,#7442,#7443));
#1679=EDGE_LOOP('',(#7444,#7445,#7446,#7447,#7448));
#1680=EDGE_LOOP('',(#7449,#7450,#7451,#7452,#7453));
#1681=EDGE_LOOP('',(#7454,#7455,#7456,#7457,#7458));
#1682=EDGE_LOOP('',(#7459,#7460,#7461,#7462,#7463,#7464,#7465,#7466,#7467,
#7468,#7469,#7470,#7471,#7472,#7473,#7474,#7475,#7476,#7477,#7478,#7479));
#1683=EDGE_LOOP('',(#7480,#7481,#7482));
#1684=EDGE_LOOP('',(#7483,#7484,#7485));
#1685=EDGE_LOOP('',(#7486,#7487,#7488));
#1686=EDGE_LOOP('',(#7489));
#1687=EDGE_LOOP('',(#7490,#7491,#7492));
#1688=EDGE_LOOP('',(#7493,#7494,#7495,#7496,#7497));
#1689=EDGE_LOOP('',(#7498,#7499,#7500,#7501,#7502));
#1690=EDGE_LOOP('',(#7503,#7504,#7505,#7506,#7507));
#1691=EDGE_LOOP('',(#7508,#7509,#7510,#7511));
#1692=EDGE_LOOP('',(#7512,#7513,#7514,#7515,#7516));
#1693=EDGE_LOOP('',(#7517,#7518,#7519,#7520));
#1694=EDGE_LOOP('',(#7521,#7522,#7523,#7524,#7525,#7526,#7527,#7528,#7529,
#7530,#7531,#7532));
#1695=EDGE_LOOP('',(#7533,#7534,#7535,#7536));
#1696=EDGE_LOOP('',(#7537,#7538,#7539,#7540,#7541));
#1697=EDGE_LOOP('',(#7542,#7543,#7544,#7545,#7546));
#1698=EDGE_LOOP('',(#7547,#7548,#7549,#7550,#7551));
#1699=EDGE_LOOP('',(#7552,#7553,#7554,#7555,#7556));
#1700=EDGE_LOOP('',(#7557,#7558,#7559,#7560,#7561));
#1701=EDGE_LOOP('',(#7562,#7563,#7564,#7565,#7566));
#1702=EDGE_LOOP('',(#7567,#7568,#7569,#7570,#7571,#7572,#7573,#7574,#7575,
#7576,#7577,#7578,#7579,#7580,#7581,#7582,#7583,#7584,#7585,#7586,#7587));
#1703=EDGE_LOOP('',(#7588,#7589,#7590));
#1704=EDGE_LOOP('',(#7591,#7592,#7593));
#1705=EDGE_LOOP('',(#7594,#7595,#7596));
#1706=EDGE_LOOP('',(#7597));
#1707=EDGE_LOOP('',(#7598,#7599,#7600));
#1708=EDGE_LOOP('',(#7601,#7602,#7603,#7604,#7605));
#1709=EDGE_LOOP('',(#7606,#7607,#7608,#7609,#7610));
#1710=EDGE_LOOP('',(#7611,#7612,#7613,#7614,#7615));
#1711=EDGE_LOOP('',(#7616,#7617,#7618,#7619));
#1712=EDGE_LOOP('',(#7620,#7621,#7622,#7623,#7624));
#1713=EDGE_LOOP('',(#7625,#7626,#7627,#7628));
#1714=EDGE_LOOP('',(#7629,#7630,#7631,#7632,#7633,#7634,#7635,#7636,#7637,
#7638,#7639,#7640));
#1715=EDGE_LOOP('',(#7641,#7642,#7643,#7644));
#1716=EDGE_LOOP('',(#7645,#7646,#7647,#7648,#7649));
#1717=EDGE_LOOP('',(#7650,#7651,#7652,#7653,#7654));
#1718=EDGE_LOOP('',(#7655,#7656,#7657,#7658,#7659));
#1719=EDGE_LOOP('',(#7660,#7661,#7662,#7663,#7664));
#1720=EDGE_LOOP('',(#7665,#7666,#7667,#7668,#7669));
#1721=EDGE_LOOP('',(#7670,#7671,#7672,#7673));
#1722=EDGE_LOOP('',(#7674,#7675,#7676,#7677));
#1723=EDGE_LOOP('',(#7678,#7679,#7680,#7681));
#1724=EDGE_LOOP('',(#7682,#7683,#7684,#7685));
#1725=EDGE_LOOP('',(#7686,#7687,#7688,#7689));
#1726=EDGE_LOOP('',(#7690,#7691,#7692,#7693));
#1727=EDGE_LOOP('',(#7694,#7695,#7696,#7697));
#1728=EDGE_LOOP('',(#7698,#7699,#7700,#7701));
#1729=EDGE_LOOP('',(#7702,#7703,#7704,#7705));
#1730=EDGE_LOOP('',(#7706,#7707,#7708,#7709));
#1731=EDGE_LOOP('',(#7710,#7711,#7712,#7713));
#1732=EDGE_LOOP('',(#7714,#7715,#7716,#7717));
#1733=EDGE_LOOP('',(#7718,#7719,#7720,#7721));
#1734=EDGE_LOOP('',(#7722,#7723,#7724,#7725));
#1735=EDGE_LOOP('',(#7726,#7727,#7728,#7729));
#1736=EDGE_LOOP('',(#7730,#7731,#7732,#7733));
#1737=EDGE_LOOP('',(#7734,#7735,#7736,#7737));
#1738=EDGE_LOOP('',(#7738,#7739,#7740,#7741));
#1739=EDGE_LOOP('',(#7742,#7743,#7744,#7745));
#1740=EDGE_LOOP('',(#7746,#7747,#7748,#7749));
#1741=EDGE_LOOP('',(#7750,#7751,#7752,#7753));
#1742=EDGE_LOOP('',(#7754,#7755,#7756,#7757));
#1743=EDGE_LOOP('',(#7758,#7759,#7760,#7761));
#1744=EDGE_LOOP('',(#7762,#7763,#7764,#7765));
#1745=EDGE_LOOP('',(#7766,#7767,#7768,#7769));
#1746=EDGE_LOOP('',(#7770,#7771,#7772,#7773));
#1747=EDGE_LOOP('',(#7774,#7775,#7776,#7777));
#1748=EDGE_LOOP('',(#7778,#7779,#7780,#7781));
#1749=EDGE_LOOP('',(#7782,#7783,#7784,#7785));
#1750=EDGE_LOOP('',(#7786,#7787,#7788,#7789));
#1751=EDGE_LOOP('',(#7790,#7791,#7792,#7793));
#1752=EDGE_LOOP('',(#7794,#7795,#7796,#7797));
#1753=EDGE_LOOP('',(#7798,#7799,#7800,#7801));
#1754=EDGE_LOOP('',(#7802,#7803,#7804,#7805));
#1755=EDGE_LOOP('',(#7806,#7807,#7808,#7809));
#1756=EDGE_LOOP('',(#7810,#7811,#7812,#7813));
#1757=EDGE_LOOP('',(#7814,#7815,#7816,#7817));
#1758=EDGE_LOOP('',(#7818,#7819,#7820,#7821));
#1759=EDGE_LOOP('',(#7822,#7823,#7824));
#1760=EDGE_LOOP('',(#7825,#7826,#7827,#7828));
#1761=EDGE_LOOP('',(#7829,#7830,#7831,#7832));
#1762=EDGE_LOOP('',(#7833,#7834,#7835,#7836));
#1763=EDGE_LOOP('',(#7837,#7838,#7839,#7840));
#1764=EDGE_LOOP('',(#7841,#7842,#7843,#7844));
#1765=EDGE_LOOP('',(#7845,#7846,#7847,#7848));
#1766=EDGE_LOOP('',(#7849,#7850,#7851,#7852));
#1767=EDGE_LOOP('',(#7853,#7854,#7855,#7856));
#1768=EDGE_LOOP('',(#7857,#7858,#7859,#7860));
#1769=EDGE_LOOP('',(#7861,#7862,#7863,#7864));
#1770=EDGE_LOOP('',(#7865,#7866,#7867,#7868));
#1771=EDGE_LOOP('',(#7869,#7870,#7871,#7872));
#1772=EDGE_LOOP('',(#7873,#7874,#7875,#7876));
#1773=EDGE_LOOP('',(#7877,#7878,#7879,#7880));
#1774=EDGE_LOOP('',(#7881,#7882,#7883,#7884));
#1775=EDGE_LOOP('',(#7885,#7886,#7887,#7888));
#1776=EDGE_LOOP('',(#7889,#7890,#7891,#7892));
#1777=EDGE_LOOP('',(#7893,#7894,#7895,#7896));
#1778=EDGE_LOOP('',(#7897,#7898,#7899,#7900));
#1779=EDGE_LOOP('',(#7901,#7902,#7903,#7904));
#1780=EDGE_LOOP('',(#7905,#7906,#7907,#7908));
#1781=EDGE_LOOP('',(#7909,#7910,#7911,#7912));
#1782=EDGE_LOOP('',(#7913,#7914,#7915,#7916));
#1783=EDGE_LOOP('',(#7917,#7918,#7919,#7920));
#1784=EDGE_LOOP('',(#7921,#7922,#7923,#7924));
#1785=EDGE_LOOP('',(#7925,#7926,#7927,#7928));
#1786=EDGE_LOOP('',(#7929,#7930,#7931,#7932));
#1787=EDGE_LOOP('',(#7933,#7934,#7935,#7936));
#1788=EDGE_LOOP('',(#7937,#7938,#7939,#7940));
#1789=EDGE_LOOP('',(#7941,#7942,#7943,#7944));
#1790=EDGE_LOOP('',(#7945,#7946,#7947,#7948));
#1791=EDGE_LOOP('',(#7949,#7950,#7951,#7952));
#1792=EDGE_LOOP('',(#7953,#7954,#7955,#7956));
#1793=EDGE_LOOP('',(#7957,#7958,#7959,#7960));
#1794=EDGE_LOOP('',(#7961,#7962,#7963,#7964));
#1795=EDGE_LOOP('',(#7965,#7966,#7967,#7968));
#1796=EDGE_LOOP('',(#7969,#7970,#7971));
#1797=EDGE_LOOP('',(#7972,#7973,#7974,#7975,#7976));
#1798=EDGE_LOOP('',(#7977,#7978,#7979,#7980));
#1799=EDGE_LOOP('',(#7981,#7982,#7983,#7984));
#1800=EDGE_LOOP('',(#7985,#7986,#7987,#7988));
#1801=EDGE_LOOP('',(#7989,#7990,#7991,#7992));
#1802=EDGE_LOOP('',(#7993,#7994,#7995,#7996));
#1803=EDGE_LOOP('',(#7997,#7998,#7999));
#1804=EDGE_LOOP('',(#8000,#8001,#8002,#8003,#8004));
#1805=EDGE_LOOP('',(#8005,#8006,#8007,#8008));
#1806=EDGE_LOOP('',(#8009,#8010,#8011,#8012));
#1807=EDGE_LOOP('',(#8013,#8014,#8015,#8016));
#1808=EDGE_LOOP('',(#8017,#8018,#8019,#8020));
#1809=EDGE_LOOP('',(#8021,#8022,#8023,#8024));
#1810=EDGE_LOOP('',(#8025,#8026,#8027));
#1811=EDGE_LOOP('',(#8028,#8029,#8030,#8031,#8032));
#1812=EDGE_LOOP('',(#8033,#8034,#8035,#8036));
#1813=EDGE_LOOP('',(#8037,#8038,#8039,#8040));
#1814=EDGE_LOOP('',(#8041,#8042,#8043,#8044));
#1815=EDGE_LOOP('',(#8045,#8046,#8047,#8048));
#1816=EDGE_LOOP('',(#8049,#8050,#8051,#8052));
#1817=EDGE_LOOP('',(#8053,#8054,#8055));
#1818=EDGE_LOOP('',(#8056,#8057,#8058,#8059,#8060));
#1819=EDGE_LOOP('',(#8061,#8062,#8063,#8064));
#1820=EDGE_LOOP('',(#8065,#8066,#8067,#8068));
#1821=EDGE_LOOP('',(#8069,#8070,#8071,#8072));
#1822=EDGE_LOOP('',(#8073,#8074,#8075,#8076));
#1823=EDGE_LOOP('',(#8077,#8078,#8079,#8080));
#1824=EDGE_LOOP('',(#8081,#8082,#8083,#8084));
#1825=EDGE_LOOP('',(#8085,#8086,#8087,#8088));
#1826=EDGE_LOOP('',(#8089,#8090,#8091,#8092));
#1827=EDGE_LOOP('',(#8093,#8094,#8095,#8096));
#1828=EDGE_LOOP('',(#8097,#8098,#8099,#8100));
#1829=EDGE_LOOP('',(#8101,#8102,#8103,#8104));
#1830=EDGE_LOOP('',(#8105,#8106,#8107,#8108));
#1831=EDGE_LOOP('',(#8109,#8110,#8111,#8112));
#1832=EDGE_LOOP('',(#8113,#8114,#8115,#8116));
#1833=EDGE_LOOP('',(#8117,#8118,#8119,#8120));
#1834=EDGE_LOOP('',(#8121,#8122,#8123,#8124));
#1835=EDGE_LOOP('',(#8125,#8126,#8127,#8128));
#1836=EDGE_LOOP('',(#8129,#8130,#8131,#8132,#8133,#8134,#8135,#8136));
#1837=EDGE_LOOP('',(#8137,#8138,#8139,#8140,#8141,#8142,#8143,#8144));
#1838=EDGE_LOOP('',(#8145,#8146,#8147,#8148,#8149,#8150,#8151,#8152));
#1839=EDGE_LOOP('',(#8153,#8154,#8155,#8156,#8157,#8158,#8159,#8160));
#1840=EDGE_LOOP('',(#8161,#8162,#8163,#8164,#8165,#8166,#8167,#8168,#8169,
#8170,#8171,#8172,#8173,#8174,#8175,#8176,#8177,#8178,#8179,#8180,#8181,
#8182,#8183,#8184,#8185,#8186,#8187,#8188,#8189,#8190,#8191,#8192));
#1841=EDGE_LOOP('',(#8193,#8194,#8195,#8196,#8197,#8198,#8199,#8200,#8201,
#8202,#8203,#8204,#8205,#8206,#8207,#8208,#8209,#8210,#8211,#8212,#8213,
#8214,#8215,#8216,#8217,#8218,#8219,#8220,#8221,#8222));
#1842=EDGE_LOOP('',(#8223,#8224,#8225,#8226));
#1843=EDGE_LOOP('',(#8227,#8228,#8229,#8230));
#1844=EDGE_LOOP('',(#8231,#8232,#8233,#8234,#8235,#8236,#8237,#8238));
#1845=EDGE_LOOP('',(#8239));
#1846=EDGE_LOOP('',(#8240,#8241,#8242,#8243,#8244));
#1847=EDGE_LOOP('',(#8245,#8246,#8247,#8248,#8249));
#1848=EDGE_LOOP('',(#8250,#8251,#8252,#8253,#8254));
#1849=EDGE_LOOP('',(#8255,#8256,#8257,#8258,#8259));
#1850=EDGE_LOOP('',(#8260,#8261,#8262,#8263,#8264,#8265,#8266,#8267,#8268,
#8269,#8270,#8271,#8272,#8273,#8274,#8275,#8276,#8277,#8278,#8279,#8280,
#8281,#8282,#8283,#8284,#8285,#8286,#8287,#8288,#8289,#8290,#8291));
#1851=EDGE_LOOP('',(#8292,#8293,#8294,#8295,#8296,#8297,#8298,#8299,#8300,
#8301,#8302,#8303,#8304,#8305,#8306,#8307,#8308,#8309,#8310,#8311,#8312,
#8313,#8314,#8315,#8316,#8317,#8318,#8319,#8320,#8321,#8322));
#1852=EDGE_LOOP('',(#8323,#8324,#8325,#8326));
#1853=EDGE_LOOP('',(#8327,#8328,#8329,#8330));
#1854=EDGE_LOOP('',(#8331,#8332,#8333,#8334,#8335,#8336,#8337,#8338,#8339,
#8340,#8341,#8342,#8343,#8344,#8345,#8346,#8347,#8348,#8349,#8350,#8351,
#8352,#8353,#8354,#8355,#8356,#8357,#8358,#8359,#8360,#8361,#8362,#8363));
#1855=EDGE_LOOP('',(#8364,#8365,#8366,#8367,#8368,#8369,#8370,#8371,#8372,
#8373,#8374,#8375,#8376,#8377,#8378,#8379,#8380,#8381,#8382,#8383,#8384,
#8385,#8386,#8387,#8388,#8389,#8390,#8391,#8392,#8393,#8394));
#1856=EDGE_LOOP('',(#8395,#8396,#8397,#8398));
#1857=EDGE_LOOP('',(#8399,#8400,#8401,#8402));
#1858=EDGE_LOOP('',(#8403,#8404,#8405,#8406,#8407,#8408,#8409,#8410,#8411,
#8412,#8413,#8414,#8415,#8416,#8417,#8418,#8419,#8420,#8421,#8422,#8423,
#8424,#8425,#8426,#8427,#8428,#8429,#8430,#8431,#8432,#8433,#8434,#8435));
#1859=EDGE_LOOP('',(#8436,#8437,#8438,#8439,#8440,#8441,#8442,#8443,#8444,
#8445,#8446,#8447,#8448,#8449,#8450,#8451,#8452,#8453,#8454,#8455,#8456,
#8457,#8458,#8459,#8460,#8461,#8462,#8463,#8464,#8465,#8466));
#1860=EDGE_LOOP('',(#8467,#8468,#8469,#8470));
#1861=EDGE_LOOP('',(#8471,#8472,#8473,#8474));
#1862=EDGE_LOOP('',(#8475));
#1863=EDGE_LOOP('',(#8476));
#1864=EDGE_LOOP('',(#8477));
#1865=EDGE_LOOP('',(#8478));
#1866=EDGE_LOOP('',(#8479,#8480,#8481,#8482));
#1867=EDGE_LOOP('',(#8483,#8484,#8485,#8486));
#1868=EDGE_LOOP('',(#8487,#8488,#8489,#8490));
#1869=EDGE_LOOP('',(#8491,#8492,#8493,#8494));
#1870=EDGE_LOOP('',(#8495,#8496,#8497,#8498));
#1871=EDGE_LOOP('',(#8499,#8500,#8501,#8502));
#1872=EDGE_LOOP('',(#8503,#8504,#8505,#8506));
#1873=EDGE_LOOP('',(#8507,#8508,#8509,#8510));
#1874=EDGE_LOOP('',(#8511,#8512,#8513,#8514));
#1875=EDGE_LOOP('',(#8515,#8516,#8517,#8518));
#1876=EDGE_LOOP('',(#8519,#8520,#8521,#8522));
#1877=EDGE_LOOP('',(#8523,#8524,#8525,#8526));
#1878=EDGE_LOOP('',(#8527,#8528,#8529,#8530));
#1879=EDGE_LOOP('',(#8531,#8532,#8533,#8534));
#1880=EDGE_LOOP('',(#8535,#8536,#8537,#8538));
#1881=EDGE_LOOP('',(#8539,#8540,#8541,#8542));
#1882=EDGE_LOOP('',(#8543,#8544,#8545,#8546,#8547,#8548,#8549,#8550));
#1883=EDGE_LOOP('',(#8551));
#1884=EDGE_LOOP('',(#8552));
#1885=EDGE_LOOP('',(#8553));
#1886=EDGE_LOOP('',(#8554));
#1887=EDGE_LOOP('',(#8555));
#1888=EDGE_LOOP('',(#8556,#8557,#8558,#8559));
#1889=EDGE_LOOP('',(#8560,#8561,#8562,#8563));
#1890=EDGE_LOOP('',(#8564,#8565,#8566));
#1891=EDGE_LOOP('',(#8567,#8568,#8569,#8570,#8571,#8572,#8573,#8574));
#1892=EDGE_LOOP('',(#8575,#8576));
#1893=EDGE_LOOP('',(#8577));
#1894=EDGE_LOOP('',(#8578));
#1895=EDGE_LOOP('',(#8579,#8580));
#1896=EDGE_LOOP('',(#8581,#8582,#8583,#8584,#8585));
#1897=EDGE_LOOP('',(#8586,#8587,#8588,#8589));
#1898=EDGE_LOOP('',(#8590,#8591,#8592,#8593));
#1899=EDGE_LOOP('',(#8594,#8595,#8596,#8597));
#1900=EDGE_LOOP('',(#8598,#8599,#8600,#8601));
#1901=EDGE_LOOP('',(#8602,#8603,#8604,#8605));
#1902=EDGE_LOOP('',(#8606,#8607,#8608,#8609));
#1903=EDGE_LOOP('',(#8610,#8611,#8612,#8613));
#1904=EDGE_LOOP('',(#8614,#8615,#8616,#8617));
#1905=EDGE_LOOP('',(#8618,#8619,#8620,#8621));
#1906=EDGE_LOOP('',(#8622,#8623,#8624,#8625));
#1907=EDGE_LOOP('',(#8626));
#1908=EDGE_LOOP('',(#8627));
#1909=EDGE_LOOP('',(#8628));
#1910=EDGE_LOOP('',(#8629));
#1911=EDGE_LOOP('',(#8630,#8631,#8632,#8633));
#1912=EDGE_LOOP('',(#8634,#8635,#8636,#8637));
#1913=EDGE_LOOP('',(#8638,#8639,#8640,#8641));
#1914=EDGE_LOOP('',(#8642,#8643,#8644,#8645));
#1915=EDGE_LOOP('',(#8646,#8647,#8648,#8649));
#1916=EDGE_LOOP('',(#8650,#8651,#8652,#8653));
#1917=EDGE_LOOP('',(#8654,#8655,#8656,#8657));
#1918=EDGE_LOOP('',(#8658,#8659,#8660,#8661));
#1919=EDGE_LOOP('',(#8662,#8663,#8664,#8665,#8666,#8667,#8668,#8669));
#1920=EDGE_LOOP('',(#8670));
#1921=EDGE_LOOP('',(#8671));
#1922=EDGE_LOOP('',(#8672));
#1923=EDGE_LOOP('',(#8673));
#1924=EDGE_LOOP('',(#8674));
#1925=EDGE_LOOP('',(#8675,#8676,#8677,#8678));
#1926=EDGE_LOOP('',(#8679,#8680,#8681,#8682));
#1927=EDGE_LOOP('',(#8683,#8684,#8685,#8686));
#1928=EDGE_LOOP('',(#8687,#8688,#8689,#8690));
#1929=EDGE_LOOP('',(#8691,#8692,#8693,#8694));
#1930=EDGE_LOOP('',(#8695,#8696,#8697,#8698));
#1931=EDGE_LOOP('',(#8699,#8700,#8701,#8702));
#1932=EDGE_LOOP('',(#8703,#8704,#8705,#8706));
#1933=EDGE_LOOP('',(#8707,#8708,#8709,#8710));
#1934=EDGE_LOOP('',(#8711,#8712,#8713,#8714));
#1935=EDGE_LOOP('',(#8715,#8716,#8717,#8718));
#1936=EDGE_LOOP('',(#8719,#8720,#8721,#8722));
#1937=EDGE_LOOP('',(#8723,#8724,#8725,#8726));
#1938=EDGE_LOOP('',(#8727,#8728,#8729,#8730,#8731));
#1939=EDGE_LOOP('',(#8732,#8733,#8734,#8735));
#1940=EDGE_LOOP('',(#8736,#8737,#8738,#8739,#8740));
#1941=EDGE_LOOP('',(#8741,#8742,#8743,#8744,#8745,#8746,#8747,#8748));
#1942=EDGE_LOOP('',(#8749,#8750,#8751,#8752));
#1943=EDGE_LOOP('',(#8753,#8754,#8755,#8756,#8757,#8758,#8759,#8760));
#1944=EDGE_LOOP('',(#8761,#8762,#8763,#8764,#8765,#8766,#8767,#8768));
#1945=EDGE_LOOP('',(#8769));
#1946=EDGE_LOOP('',(#8770));
#1947=EDGE_LOOP('',(#8771));
#1948=EDGE_LOOP('',(#8772,#8773,#8774,#8775));
#1949=EDGE_LOOP('',(#8776,#8777,#8778,#8779));
#1950=EDGE_LOOP('',(#8780,#8781,#8782,#8783));
#1951=EDGE_LOOP('',(#8784,#8785,#8786,#8787));
#1952=EDGE_LOOP('',(#8788,#8789,#8790,#8791));
#1953=EDGE_LOOP('',(#8792,#8793,#8794,#8795,#8796,#8797,#8798,#8799));
#1954=EDGE_LOOP('',(#8800));
#1955=EDGE_LOOP('',(#8801,#8802,#8803,#8804,#8805,#8806,#8807,#8808));
#1956=EDGE_LOOP('',(#8809));
#1957=EDGE_LOOP('',(#8810));
#1958=EDGE_LOOP('',(#8811));
#1959=EDGE_LOOP('',(#8812));
#1960=EDGE_LOOP('',(#8813));
#1961=EDGE_LOOP('',(#8814,#8815,#8816,#8817));
#1962=EDGE_LOOP('',(#8818,#8819,#8820,#8821));
#1963=EDGE_LOOP('',(#8822,#8823,#8824,#8825));
#1964=EDGE_LOOP('',(#8826,#8827,#8828,#8829));
#1965=EDGE_LOOP('',(#8830,#8831,#8832,#8833));
#1966=EDGE_LOOP('',(#8834,#8835,#8836,#8837));
#1967=EDGE_LOOP('',(#8838,#8839,#8840,#8841));
#1968=EDGE_LOOP('',(#8842,#8843,#8844,#8845));
#1969=EDGE_LOOP('',(#8846));
#1970=EDGE_LOOP('',(#8847));
#1971=EDGE_LOOP('',(#8848));
#1972=EDGE_LOOP('',(#8849));
#1973=EDGE_LOOP('',(#8850,#8851,#8852,#8853));
#1974=EDGE_LOOP('',(#8854,#8855,#8856,#8857));
#1975=EDGE_LOOP('',(#8858));
#1976=EDGE_LOOP('',(#8859));
#1977=EDGE_LOOP('',(#8860,#8861,#8862,#8863));
#1978=EDGE_LOOP('',(#8864));
#1979=EDGE_LOOP('',(#8865));
#1980=EDGE_LOOP('',(#8866,#8867,#8868,#8869));
#1981=EDGE_LOOP('',(#8870,#8871,#8872,#8873));
#1982=EDGE_LOOP('',(#8874,#8875,#8876,#8877));
#1983=EDGE_LOOP('',(#8878));
#1984=EDGE_LOOP('',(#8879));
#1985=EDGE_LOOP('',(#8880));
#1986=EDGE_LOOP('',(#8881));
#1987=EDGE_LOOP('',(#8882,#8883,#8884,#8885));
#1988=EDGE_LOOP('',(#8886,#8887,#8888,#8889));
#1989=EDGE_LOOP('',(#8890,#8891,#8892,#8893));
#1990=EDGE_LOOP('',(#8894,#8895,#8896,#8897));
#1991=EDGE_LOOP('',(#8898,#8899,#8900,#8901,#8902,#8903,#8904,#8905,#8906,
#8907));
#1992=EDGE_LOOP('',(#8908,#8909,#8910,#8911));
#1993=EDGE_LOOP('',(#8912,#8913,#8914,#8915,#8916,#8917));
#1994=EDGE_LOOP('',(#8918,#8919,#8920,#8921));
#1995=EDGE_LOOP('',(#8922,#8923,#8924,#8925));
#1996=EDGE_LOOP('',(#8926));
#1997=EDGE_LOOP('',(#8927));
#1998=EDGE_LOOP('',(#8928,#8929,#8930,#8931,#8932,#8933,#8934,#8935,#8936,
#8937));
#1999=EDGE_LOOP('',(#8938));
#2000=EDGE_LOOP('',(#8939));
#2001=EDGE_LOOP('',(#8940,#8941,#8942,#8943));
#2002=EDGE_LOOP('',(#8944,#8945,#8946,#8947));
#2003=EDGE_LOOP('',(#8948,#8949,#8950,#8951));
#2004=EDGE_LOOP('',(#8952,#8953,#8954,#8955));
#2005=EDGE_LOOP('',(#8956,#8957,#8958,#8959));
#2006=EDGE_LOOP('',(#8960,#8961,#8962,#8963,#8964));
#2007=EDGE_LOOP('',(#8965,#8966,#8967,#8968,#8969));
#2008=EDGE_LOOP('',(#8970));
#2009=EDGE_LOOP('',(#8971));
#2010=EDGE_LOOP('',(#8972));
#2011=EDGE_LOOP('',(#8973));
#2012=EDGE_LOOP('',(#8974,#8975,#8976,#8977));
#2013=EDGE_LOOP('',(#8978,#8979,#8980,#8981));
#2014=EDGE_LOOP('',(#8982,#8983,#8984,#8985));
#2015=EDGE_LOOP('',(#8986,#8987,#8988,#8989));
#2016=EDGE_LOOP('',(#8990));
#2017=EDGE_LOOP('',(#8991));
#2018=EDGE_LOOP('',(#8992));
#2019=EDGE_LOOP('',(#8993));
#2020=EDGE_LOOP('',(#8994,#8995,#8996,#8997));
#2021=EDGE_LOOP('',(#8998,#8999,#9000,#9001,#9002));
#2022=EDGE_LOOP('',(#9003,#9004,#9005,#9006,#9007));
#2023=EDGE_LOOP('',(#9008,#9009,#9010,#9011));
#2024=EDGE_LOOP('',(#9012,#9013,#9014,#9015));
#2025=EDGE_LOOP('',(#9016,#9017,#9018,#9019));
#2026=EDGE_LOOP('',(#9020,#9021,#9022,#9023));
#2027=EDGE_LOOP('',(#9024));
#2028=EDGE_LOOP('',(#9025));
#2029=EDGE_LOOP('',(#9026));
#2030=EDGE_LOOP('',(#9027));
#2031=EDGE_LOOP('',(#9028));
#2032=EDGE_LOOP('',(#9029));
#2033=EDGE_LOOP('',(#9030,#9031));
#2034=EDGE_LOOP('',(#9032,#9033));
#2035=EDGE_LOOP('',(#9034,#9035));
#2036=EDGE_LOOP('',(#9036,#9037));
#2037=EDGE_LOOP('',(#9038,#9039));
#2038=EDGE_LOOP('',(#9040,#9041));
#2039=EDGE_LOOP('',(#9042,#9043));
#2040=EDGE_LOOP('',(#9044,#9045));
#2041=EDGE_LOOP('',(#9046,#9047));
#2042=EDGE_LOOP('',(#9048,#9049));
#2043=EDGE_LOOP('',(#9050,#9051,#9052,#9053));
#2044=EDGE_LOOP('',(#9054,#9055,#9056,#9057));
#2045=EDGE_LOOP('',(#9058,#9059,#9060,#9061));
#2046=EDGE_LOOP('',(#9062,#9063,#9064,#9065));
#2047=EDGE_LOOP('',(#9066,#9067,#9068,#9069));
#2048=EDGE_LOOP('',(#9070,#9071,#9072,#9073));
#2049=EDGE_LOOP('',(#9074,#9075,#9076,#9077));
#2050=EDGE_LOOP('',(#9078,#9079,#9080,#9081));
#2051=EDGE_LOOP('',(#9082,#9083,#9084,#9085));
#2052=EDGE_LOOP('',(#9086,#9087,#9088,#9089));
#2053=EDGE_LOOP('',(#9090,#9091,#9092,#9093));
#2054=EDGE_LOOP('',(#9094,#9095,#9096,#9097));
#2055=EDGE_LOOP('',(#9098,#9099,#9100,#9101));
#2056=EDGE_LOOP('',(#9102,#9103,#9104,#9105));
#2057=EDGE_LOOP('',(#9106,#9107,#9108,#9109));
#2058=EDGE_LOOP('',(#9110,#9111,#9112,#9113));
#2059=EDGE_LOOP('',(#9114,#9115,#9116,#9117));
#2060=EDGE_LOOP('',(#9118,#9119,#9120,#9121));
#2061=EDGE_LOOP('',(#9122,#9123,#9124,#9125));
#2062=EDGE_LOOP('',(#9126,#9127,#9128,#9129));
#2063=EDGE_LOOP('',(#9130,#9131,#9132,#9133));
#2064=EDGE_LOOP('',(#9134,#9135,#9136,#9137));
#2065=EDGE_LOOP('',(#9138,#9139,#9140,#9141));
#2066=EDGE_LOOP('',(#9142,#9143,#9144,#9145));
#2067=EDGE_LOOP('',(#9146,#9147,#9148,#9149));
#2068=EDGE_LOOP('',(#9150,#9151,#9152,#9153));
#2069=EDGE_LOOP('',(#9154,#9155,#9156,#9157));
#2070=EDGE_LOOP('',(#9158,#9159,#9160,#9161));
#2071=EDGE_LOOP('',(#9162,#9163,#9164,#9165));
#2072=EDGE_LOOP('',(#9166,#9167,#9168,#9169));
#2073=EDGE_LOOP('',(#9170,#9171,#9172,#9173));
#2074=EDGE_LOOP('',(#9174,#9175,#9176,#9177));
#2075=EDGE_LOOP('',(#9178,#9179,#9180,#9181));
#2076=EDGE_LOOP('',(#9182,#9183,#9184,#9185));
#2077=EDGE_LOOP('',(#9186,#9187,#9188,#9189));
#2078=EDGE_LOOP('',(#9190,#9191,#9192,#9193));
#2079=EDGE_LOOP('',(#9194,#9195,#9196,#9197));
#2080=EDGE_LOOP('',(#9198,#9199,#9200,#9201));
#2081=EDGE_LOOP('',(#9202,#9203,#9204,#9205));
#2082=EDGE_LOOP('',(#9206,#9207,#9208,#9209));
#2083=EDGE_LOOP('',(#9210,#9211,#9212,#9213));
#2084=EDGE_LOOP('',(#9214,#9215,#9216,#9217));
#2085=EDGE_LOOP('',(#9218,#9219,#9220,#9221));
#2086=EDGE_LOOP('',(#9222,#9223,#9224,#9225));
#2087=EDGE_LOOP('',(#9226,#9227,#9228,#9229));
#2088=EDGE_LOOP('',(#9230,#9231,#9232,#9233));
#2089=EDGE_LOOP('',(#9234,#9235,#9236,#9237));
#2090=EDGE_LOOP('',(#9238,#9239,#9240,#9241,#9242,#9243,#9244,#9245,#9246,
#9247,#9248,#9249,#9250,#9251,#9252,#9253,#9254,#9255,#9256,#9257,#9258,
#9259,#9260,#9261,#9262,#9263,#9264,#9265,#9266,#9267,#9268,#9269,#9270,
#9271,#9272,#9273,#9274,#9275,#9276,#9277,#9278,#9279,#9280,#9281,#9282,
#9283,#9284,#9285,#9286,#9287,#9288,#9289,#9290,#9291,#9292,#9293,#9294,
#9295,#9296,#9297,#9298,#9299,#9300,#9301,#9302,#9303,#9304,#9305,#9306,
#9307,#9308,#9309,#9310,#9311,#9312,#9313,#9314,#9315,#9316,#9317));
#2091=EDGE_LOOP('',(#9318,#9319,#9320,#9321,#9322,#9323,#9324,#9325,#9326,
#9327,#9328,#9329));
#2092=EDGE_LOOP('',(#9330));
#2093=EDGE_LOOP('',(#9331));
#2094=EDGE_LOOP('',(#9332,#9333,#9334,#9335));
#2095=EDGE_LOOP('',(#9336,#9337,#9338,#9339));
#2096=EDGE_LOOP('',(#9340,#9341,#9342,#9343));
#2097=EDGE_LOOP('',(#9344,#9345,#9346,#9347));
#2098=EDGE_LOOP('',(#9348,#9349,#9350,#9351));
#2099=EDGE_LOOP('',(#9352,#9353,#9354,#9355));
#2100=EDGE_LOOP('',(#9356,#9357,#9358,#9359));
#2101=EDGE_LOOP('',(#9360,#9361,#9362,#9363));
#2102=EDGE_LOOP('',(#9364,#9365,#9366,#9367));
#2103=EDGE_LOOP('',(#9368,#9369,#9370,#9371));
#2104=EDGE_LOOP('',(#9372,#9373,#9374,#9375));
#2105=EDGE_LOOP('',(#9376,#9377,#9378,#9379));
#2106=EDGE_LOOP('',(#9380,#9381,#9382,#9383));
#2107=EDGE_LOOP('',(#9384,#9385,#9386,#9387));
#2108=EDGE_LOOP('',(#9388,#9389,#9390,#9391));
#2109=EDGE_LOOP('',(#9392,#9393,#9394,#9395));
#2110=EDGE_LOOP('',(#9396,#9397,#9398,#9399));
#2111=EDGE_LOOP('',(#9400,#9401,#9402,#9403));
#2112=EDGE_LOOP('',(#9404,#9405,#9406,#9407));
#2113=EDGE_LOOP('',(#9408,#9409,#9410,#9411));
#2114=EDGE_LOOP('',(#9412,#9413,#9414,#9415));
#2115=EDGE_LOOP('',(#9416,#9417,#9418,#9419));
#2116=EDGE_LOOP('',(#9420,#9421,#9422,#9423));
#2117=EDGE_LOOP('',(#9424,#9425,#9426,#9427));
#2118=EDGE_LOOP('',(#9428,#9429,#9430,#9431));
#2119=EDGE_LOOP('',(#9432,#9433,#9434,#9435));
#2120=EDGE_LOOP('',(#9436,#9437,#9438,#9439));
#2121=EDGE_LOOP('',(#9440,#9441,#9442,#9443));
#2122=EDGE_LOOP('',(#9444,#9445,#9446,#9447));
#2123=EDGE_LOOP('',(#9448,#9449,#9450,#9451));
#2124=EDGE_LOOP('',(#9452,#9453,#9454,#9455));
#2125=EDGE_LOOP('',(#9456,#9457,#9458,#9459));
#2126=EDGE_LOOP('',(#9460,#9461,#9462,#9463));
#2127=EDGE_LOOP('',(#9464,#9465,#9466,#9467));
#2128=EDGE_LOOP('',(#9468,#9469,#9470,#9471));
#2129=EDGE_LOOP('',(#9472,#9473,#9474,#9475));
#2130=EDGE_LOOP('',(#9476,#9477,#9478,#9479));
#2131=EDGE_LOOP('',(#9480,#9481,#9482,#9483));
#2132=EDGE_LOOP('',(#9484,#9485,#9486,#9487));
#2133=EDGE_LOOP('',(#9488,#9489,#9490,#9491));
#2134=EDGE_LOOP('',(#9492,#9493,#9494,#9495));
#2135=EDGE_LOOP('',(#9496,#9497,#9498,#9499));
#2136=EDGE_LOOP('',(#9500,#9501,#9502,#9503));
#2137=EDGE_LOOP('',(#9504,#9505,#9506,#9507));
#2138=EDGE_LOOP('',(#9508,#9509,#9510,#9511));
#2139=EDGE_LOOP('',(#9512,#9513,#9514,#9515));
#2140=EDGE_LOOP('',(#9516,#9517,#9518,#9519));
#2141=EDGE_LOOP('',(#9520,#9521,#9522,#9523,#9524,#9525,#9526,#9527,#9528,
#9529,#9530,#9531,#9532,#9533,#9534,#9535,#9536,#9537,#9538,#9539,#9540,
#9541,#9542,#9543,#9544,#9545,#9546,#9547,#9548,#9549,#9550,#9551,#9552,
#9553,#9554,#9555,#9556,#9557,#9558,#9559,#9560,#9561,#9562,#9563,#9564,
#9565,#9566,#9567,#9568,#9569,#9570,#9571,#9572,#9573,#9574,#9575,#9576,
#9577,#9578,#9579,#9580,#9581,#9582,#9583,#9584,#9585,#9586,#9587,#9588,
#9589,#9590,#9591,#9592,#9593,#9594,#9595,#9596,#9597,#9598,#9599));
#2142=EDGE_LOOP('',(#9600));
#2143=EDGE_LOOP('',(#9601,#9602,#9603,#9604,#9605,#9606,#9607,#9608,#9609,
#9610,#9611,#9612));
#2144=EDGE_LOOP('',(#9613));
#2145=EDGE_LOOP('',(#9614));
#2146=EDGE_LOOP('',(#9615));
#2147=EDGE_LOOP('',(#9616,#9617,#9618,#9619));
#2148=EDGE_LOOP('',(#9620));
#2149=EDGE_LOOP('',(#9621));
#2150=EDGE_LOOP('',(#9622));
#2151=EDGE_LOOP('',(#9623));
#2152=EDGE_LOOP('',(#9624,#9625,#9626,#9627));
#2153=EDGE_LOOP('',(#9628,#9629,#9630,#9631));
#2154=EDGE_LOOP('',(#9632));
#2155=EDGE_LOOP('',(#9633));
#2156=EDGE_LOOP('',(#9634,#9635,#9636,#9637));
#2157=EDGE_LOOP('',(#9638,#9639,#9640,#9641));
#2158=EDGE_LOOP('',(#9642,#9643,#9644,#9645));
#2159=EDGE_LOOP('',(#9646,#9647,#9648,#9649));
#2160=EDGE_LOOP('',(#9650,#9651,#9652,#9653));
#2161=EDGE_LOOP('',(#9654,#9655,#9656,#9657));
#2162=EDGE_LOOP('',(#9658,#9659,#9660,#9661));
#2163=EDGE_LOOP('',(#9662,#9663,#9664,#9665));
#2164=EDGE_LOOP('',(#9666,#9667,#9668,#9669));
#2165=EDGE_LOOP('',(#9670,#9671,#9672,#9673));
#2166=EDGE_LOOP('',(#9674,#9675,#9676,#9677));
#2167=EDGE_LOOP('',(#9678,#9679,#9680,#9681));
#2168=EDGE_LOOP('',(#9682,#9683,#9684,#9685));
#2169=EDGE_LOOP('',(#9686,#9687,#9688,#9689));
#2170=EDGE_LOOP('',(#9690,#9691,#9692,#9693));
#2171=EDGE_LOOP('',(#9694,#9695,#9696,#9697));
#2172=EDGE_LOOP('',(#9698,#9699,#9700,#9701));
#2173=EDGE_LOOP('',(#9702,#9703,#9704,#9705));
#2174=EDGE_LOOP('',(#9706,#9707,#9708,#9709));
#2175=EDGE_LOOP('',(#9710,#9711,#9712,#9713));
#2176=EDGE_LOOP('',(#9714,#9715,#9716,#9717));
#2177=EDGE_LOOP('',(#9718,#9719,#9720,#9721));
#2178=EDGE_LOOP('',(#9722,#9723,#9724,#9725));
#2179=EDGE_LOOP('',(#9726,#9727,#9728,#9729));
#2180=EDGE_LOOP('',(#9730,#9731,#9732,#9733));
#2181=EDGE_LOOP('',(#9734,#9735,#9736,#9737));
#2182=EDGE_LOOP('',(#9738,#9739,#9740,#9741));
#2183=EDGE_LOOP('',(#9742,#9743,#9744,#9745));
#2184=EDGE_LOOP('',(#9746,#9747,#9748,#9749));
#2185=EDGE_LOOP('',(#9750,#9751,#9752,#9753));
#2186=EDGE_LOOP('',(#9754,#9755,#9756,#9757));
#2187=EDGE_LOOP('',(#9758,#9759,#9760,#9761));
#2188=EDGE_LOOP('',(#9762,#9763,#9764,#9765));
#2189=EDGE_LOOP('',(#9766,#9767,#9768,#9769));
#2190=EDGE_LOOP('',(#9770,#9771,#9772,#9773,#9774,#9775,#9776,#9777,#9778,
#9779,#9780,#9781,#9782,#9783,#9784,#9785));
#2191=EDGE_LOOP('',(#9786));
#2192=EDGE_LOOP('',(#9787));
#2193=EDGE_LOOP('',(#9788,#9789,#9790,#9791));
#2194=EDGE_LOOP('',(#9792));
#2195=EDGE_LOOP('',(#9793));
#2196=EDGE_LOOP('',(#9794,#9795,#9796,#9797));
#2197=EDGE_LOOP('',(#9798,#9799,#9800,#9801));
#2198=EDGE_LOOP('',(#9802));
#2199=EDGE_LOOP('',(#9803,#9804,#9805,#9806,#9807,#9808,#9809,#9810,#9811,
#9812,#9813,#9814,#9815,#9816,#9817,#9818));
#2200=EDGE_LOOP('',(#9819));
#2201=EDGE_LOOP('',(#9820));
#2202=EDGE_LOOP('',(#9821,#9822,#9823,#9824));
#2203=EDGE_LOOP('',(#9825));
#2204=EDGE_LOOP('',(#9826));
#2205=EDGE_LOOP('',(#9827,#9828,#9829,#9830));
#2206=EDGE_LOOP('',(#9831,#9832,#9833,#9834));
#2207=EDGE_LOOP('',(#9835));
#2208=EDGE_LOOP('',(#9836,#9837,#9838,#9839));
#2209=EDGE_LOOP('',(#9840,#9841,#9842,#9843,#9844,#9845,#9846,#9847));
#2210=EDGE_LOOP('',(#9848,#9849,#9850,#9851,#9852,#9853,#9854,#9855,#9856));
#2211=EDGE_LOOP('',(#9857));
#2212=EDGE_LOOP('',(#9858));
#2213=EDGE_LOOP('',(#9859));
#2214=EDGE_LOOP('',(#9860));
#2215=EDGE_LOOP('',(#9861));
#2216=EDGE_LOOP('',(#9862,#9863,#9864,#9865));
#2217=EDGE_LOOP('',(#9866));
#2218=EDGE_LOOP('',(#9867));
#2219=EDGE_LOOP('',(#9868,#9869,#9870,#9871));
#2220=EDGE_LOOP('',(#9872,#9873,#9874,#9875,#9876,#9877,#9878,#9879,#9880));
#2221=EDGE_LOOP('',(#9881));
#2222=EDGE_LOOP('',(#9882,#9883,#9884,#9885));
#2223=EDGE_LOOP('',(#9886));
#2224=EDGE_LOOP('',(#9887));
#2225=EDGE_LOOP('',(#9888));
#2226=EDGE_LOOP('',(#9889));
#2227=EDGE_LOOP('',(#9890,#9891,#9892,#9893));
#2228=EDGE_LOOP('',(#9894,#9895,#9896,#9897));
#2229=EDGE_LOOP('',(#9898,#9899,#9900,#9901));
#2230=EDGE_LOOP('',(#9902,#9903,#9904,#9905));
#2231=EDGE_LOOP('',(#9906,#9907,#9908,#9909));
#2232=EDGE_LOOP('',(#9910,#9911,#9912,#9913));
#2233=EDGE_LOOP('',(#9914,#9915,#9916,#9917));
#2234=EDGE_LOOP('',(#9918,#9919,#9920,#9921));
#2235=EDGE_LOOP('',(#9922,#9923,#9924,#9925));
#2236=EDGE_LOOP('',(#9926,#9927,#9928,#9929));
#2237=EDGE_LOOP('',(#9930,#9931,#9932,#9933));
#2238=EDGE_LOOP('',(#9934,#9935,#9936,#9937));
#2239=EDGE_LOOP('',(#9938,#9939,#9940,#9941));
#2240=EDGE_LOOP('',(#9942,#9943,#9944,#9945));
#2241=EDGE_LOOP('',(#9946,#9947,#9948,#9949));
#2242=EDGE_LOOP('',(#9950,#9951,#9952,#9953));
#2243=EDGE_LOOP('',(#9954,#9955,#9956,#9957));
#2244=EDGE_LOOP('',(#9958,#9959,#9960,#9961));
#2245=EDGE_LOOP('',(#9962,#9963,#9964,#9965));
#2246=EDGE_LOOP('',(#9966,#9967,#9968,#9969));
#2247=EDGE_LOOP('',(#9970,#9971,#9972,#9973));
#2248=EDGE_LOOP('',(#9974,#9975,#9976,#9977));
#2249=EDGE_LOOP('',(#9978,#9979,#9980,#9981));
#2250=EDGE_LOOP('',(#9982,#9983,#9984,#9985));
#2251=EDGE_LOOP('',(#9986,#9987,#9988,#9989));
#2252=EDGE_LOOP('',(#9990,#9991,#9992,#9993));
#2253=EDGE_LOOP('',(#9994,#9995,#9996,#9997));
#2254=EDGE_LOOP('',(#9998,#9999,#10000,#10001));
#2255=EDGE_LOOP('',(#10002,#10003,#10004,#10005));
#2256=EDGE_LOOP('',(#10006,#10007,#10008,#10009));
#2257=EDGE_LOOP('',(#10010,#10011,#10012,#10013));
#2258=EDGE_LOOP('',(#10014,#10015,#10016,#10017));
#2259=EDGE_LOOP('',(#10018,#10019,#10020,#10021));
#2260=EDGE_LOOP('',(#10022,#10023,#10024,#10025));
#2261=EDGE_LOOP('',(#10026,#10027,#10028,#10029));
#2262=EDGE_LOOP('',(#10030,#10031,#10032,#10033));
#2263=EDGE_LOOP('',(#10034,#10035,#10036,#10037));
#2264=EDGE_LOOP('',(#10038,#10039,#10040,#10041));
#2265=EDGE_LOOP('',(#10042,#10043,#10044,#10045));
#2266=EDGE_LOOP('',(#10046,#10047,#10048,#10049));
#2267=EDGE_LOOP('',(#10050,#10051,#10052,#10053));
#2268=EDGE_LOOP('',(#10054,#10055,#10056,#10057));
#2269=EDGE_LOOP('',(#10058,#10059,#10060,#10061));
#2270=EDGE_LOOP('',(#10062,#10063,#10064,#10065));
#2271=EDGE_LOOP('',(#10066,#10067,#10068,#10069));
#2272=EDGE_LOOP('',(#10070,#10071,#10072,#10073));
#2273=EDGE_LOOP('',(#10074,#10075,#10076,#10077));
#2274=EDGE_LOOP('',(#10078,#10079,#10080,#10081));
#2275=EDGE_LOOP('',(#10082,#10083,#10084,#10085));
#2276=EDGE_LOOP('',(#10086,#10087,#10088,#10089));
#2277=EDGE_LOOP('',(#10090,#10091,#10092,#10093));
#2278=EDGE_LOOP('',(#10094,#10095,#10096,#10097));
#2279=EDGE_LOOP('',(#10098,#10099,#10100,#10101));
#2280=EDGE_LOOP('',(#10102,#10103,#10104,#10105));
#2281=EDGE_LOOP('',(#10106,#10107,#10108,#10109));
#2282=EDGE_LOOP('',(#10110,#10111,#10112,#10113));
#2283=EDGE_LOOP('',(#10114,#10115,#10116,#10117));
#2284=EDGE_LOOP('',(#10118,#10119,#10120,#10121));
#2285=EDGE_LOOP('',(#10122,#10123,#10124,#10125));
#2286=EDGE_LOOP('',(#10126,#10127,#10128,#10129));
#2287=EDGE_LOOP('',(#10130,#10131,#10132,#10133));
#2288=EDGE_LOOP('',(#10134,#10135,#10136,#10137));
#2289=EDGE_LOOP('',(#10138,#10139,#10140,#10141));
#2290=EDGE_LOOP('',(#10142,#10143,#10144,#10145));
#2291=EDGE_LOOP('',(#10146,#10147,#10148,#10149));
#2292=EDGE_LOOP('',(#10150,#10151,#10152,#10153));
#2293=EDGE_LOOP('',(#10154,#10155,#10156,#10157));
#2294=EDGE_LOOP('',(#10158,#10159,#10160,#10161,#10162,#10163,#10164,#10165));
#2295=EDGE_LOOP('',(#10166));
#2296=EDGE_LOOP('',(#10167));
#2297=EDGE_LOOP('',(#10168,#10169,#10170,#10171));
#2298=EDGE_LOOP('',(#10172,#10173,#10174,#10175));
#2299=EDGE_LOOP('',(#10176,#10177,#10178,#10179));
#2300=EDGE_LOOP('',(#10180,#10181,#10182,#10183));
#2301=EDGE_LOOP('',(#10184));
#2302=EDGE_LOOP('',(#10185));
#2303=EDGE_LOOP('',(#10186,#10187,#10188,#10189));
#2304=EDGE_LOOP('',(#10190));
#2305=EDGE_LOOP('',(#10191));
#2306=EDGE_LOOP('',(#10192));
#2307=EDGE_LOOP('',(#10193));
#2308=EDGE_LOOP('',(#10194));
#2309=EDGE_LOOP('',(#10195,#10196,#10197,#10198));
#2310=EDGE_LOOP('',(#10199,#10200,#10201,#10202));
#2311=EDGE_LOOP('',(#10203));
#2312=EDGE_LOOP('',(#10204));
#2313=EDGE_LOOP('',(#10205));
#2314=EDGE_LOOP('',(#10206));
#2315=EDGE_LOOP('',(#10207));
#2316=EDGE_LOOP('',(#10208,#10209,#10210,#10211));
#2317=EDGE_LOOP('',(#10212));
#2318=EDGE_LOOP('',(#10213,#10214,#10215,#10216,#10217,#10218,#10219,#10220));
#2319=EDGE_LOOP('',(#10221));
#2320=EDGE_LOOP('',(#10222));
#2321=EDGE_LOOP('',(#10223,#10224,#10225,#10226));
#2322=EDGE_LOOP('',(#10227,#10228,#10229,#10230));
#2323=EDGE_LOOP('',(#10231,#10232,#10233,#10234));
#2324=EDGE_LOOP('',(#10235,#10236,#10237,#10238));
#2325=EDGE_LOOP('',(#10239));
#2326=EDGE_LOOP('',(#10240));
#2327=EDGE_LOOP('',(#10241,#10242,#10243,#10244));
#2328=EDGE_LOOP('',(#10245));
#2329=EDGE_LOOP('',(#10246));
#2330=EDGE_LOOP('',(#10247));
#2331=EDGE_LOOP('',(#10248));
#2332=EDGE_LOOP('',(#10249));
#2333=EDGE_LOOP('',(#10250,#10251,#10252,#10253));
#2334=EDGE_LOOP('',(#10254,#10255,#10256,#10257));
#2335=EDGE_LOOP('',(#10258));
#2336=EDGE_LOOP('',(#10259));
#2337=EDGE_LOOP('',(#10260));
#2338=EDGE_LOOP('',(#10261));
#2339=EDGE_LOOP('',(#10262));
#2340=EDGE_LOOP('',(#10263,#10264,#10265,#10266));
#2341=EDGE_LOOP('',(#10267));
#2342=EDGE_LOOP('',(#10268,#10269,#10270,#10271));
#2343=EDGE_LOOP('',(#10272,#10273,#10274,#10275));
#2344=EDGE_LOOP('',(#10276,#10277,#10278,#10279));
#2345=EDGE_LOOP('',(#10280,#10281,#10282,#10283));
#2346=EDGE_LOOP('',(#10284,#10285,#10286,#10287));
#2347=EDGE_LOOP('',(#10288,#10289,#10290,#10291));
#2348=EDGE_LOOP('',(#10292,#10293,#10294,#10295));
#2349=EDGE_LOOP('',(#10296,#10297,#10298,#10299));
#2350=EDGE_LOOP('',(#10300,#10301,#10302,#10303));
#2351=EDGE_LOOP('',(#10304,#10305,#10306,#10307));
#2352=EDGE_LOOP('',(#10308,#10309,#10310,#10311));
#2353=EDGE_LOOP('',(#10312,#10313,#10314,#10315));
#2354=EDGE_LOOP('',(#10316,#10317,#10318,#10319));
#2355=EDGE_LOOP('',(#10320,#10321,#10322,#10323,#10324,#10325,#10326,#10327));
#2356=EDGE_LOOP('',(#10328));
#2357=EDGE_LOOP('',(#10329));
#2358=EDGE_LOOP('',(#10330));
#2359=EDGE_LOOP('',(#10331));
#2360=EDGE_LOOP('',(#10332));
#2361=EDGE_LOOP('',(#10333,#10334,#10335,#10336,#10337,#10338,#10339,#10340));
#2362=EDGE_LOOP('',(#10341));
#2363=EDGE_LOOP('',(#10342));
#2364=EDGE_LOOP('',(#10343));
#2365=EDGE_LOOP('',(#10344));
#2366=EDGE_LOOP('',(#10345));
#2367=EDGE_LOOP('',(#10346,#10347,#10348,#10349));
#2368=EDGE_LOOP('',(#10350,#10351,#10352,#10353));
#2369=EDGE_LOOP('',(#10354));
#2370=EDGE_LOOP('',(#10355));
#2371=EDGE_LOOP('',(#10356,#10357,#10358,#10359));
#2372=EDGE_LOOP('',(#10360,#10361,#10362));
#2373=EDGE_LOOP('',(#10363,#10364,#10365));
#2374=EDGE_LOOP('',(#10366,#10367,#10368));
#2375=EDGE_LOOP('',(#10369,#10370,#10371));
#2376=EDGE_LOOP('',(#10372,#10373,#10374));
#2377=EDGE_LOOP('',(#10375,#10376,#10377));
#2378=EDGE_LOOP('',(#10378,#10379,#10380,#10381));
#2379=EDGE_LOOP('',(#10382,#10383,#10384,#10385));
#2380=EDGE_LOOP('',(#10386,#10387,#10388,#10389));
#2381=EDGE_LOOP('',(#10390,#10391,#10392,#10393));
#2382=EDGE_LOOP('',(#10394,#10395,#10396,#10397));
#2383=EDGE_LOOP('',(#10398,#10399,#10400,#10401));
#2384=EDGE_LOOP('',(#10402));
#2385=EDGE_LOOP('',(#10403));
#2386=EDGE_LOOP('',(#10404,#10405,#10406,#10407,#10408,#10409));
#2387=EDGE_LOOP('',(#10410,#10411,#10412,#10413));
#2388=LINE('',#15387,#3334);
#2389=LINE('',#15450,#3335);
#2390=LINE('',#15451,#3336);
#2391=LINE('',#15454,#3337);
#2392=LINE('',#15455,#3338);
#2393=LINE('',#15458,#3339);
#2394=LINE('',#15459,#3340);
#2395=LINE('',#15463,#3341);
#2396=LINE('',#15464,#3342);
#2397=LINE('',#15467,#3343);
#2398=LINE('',#15469,#3344);
#2399=LINE('',#15470,#3345);
#2400=LINE('',#15473,#3346);
#2401=LINE('',#15475,#3347);
#2402=LINE('',#15476,#3348);
#2403=LINE('',#15479,#3349);
#2404=LINE('',#15481,#3350);
#2405=LINE('',#15482,#3351);
#2406=LINE('',#15484,#3352);
#2407=LINE('',#15487,#3353);
#2408=LINE('',#15489,#3354);
#2409=LINE('',#15490,#3355);
#2410=LINE('',#15492,#3356);
#2411=LINE('',#15495,#3357);
#2412=LINE('',#15497,#3358);
#2413=LINE('',#15498,#3359);
#2414=LINE('',#15500,#3360);
#2415=LINE('',#15502,#3361);
#2416=LINE('',#15503,#3362);
#2417=LINE('',#15505,#3363);
#2418=LINE('',#15506,#3364);
#2419=LINE('',#15510,#3365);
#2420=LINE('',#15512,#3366);
#2421=LINE('',#15518,#3367);
#2422=LINE('',#15581,#3368);
#2423=LINE('',#15582,#3369);
#2424=LINE('',#15585,#3370);
#2425=LINE('',#15586,#3371);
#2426=LINE('',#15589,#3372);
#2427=LINE('',#15590,#3373);
#2428=LINE('',#15594,#3374);
#2429=LINE('',#15595,#3375);
#2430=LINE('',#15598,#3376);
#2431=LINE('',#15600,#3377);
#2432=LINE('',#15601,#3378);
#2433=LINE('',#15604,#3379);
#2434=LINE('',#15606,#3380);
#2435=LINE('',#15607,#3381);
#2436=LINE('',#15610,#3382);
#2437=LINE('',#15612,#3383);
#2438=LINE('',#15613,#3384);
#2439=LINE('',#15615,#3385);
#2440=LINE('',#15618,#3386);
#2441=LINE('',#15620,#3387);
#2442=LINE('',#15621,#3388);
#2443=LINE('',#15623,#3389);
#2444=LINE('',#15626,#3390);
#2445=LINE('',#15628,#3391);
#2446=LINE('',#15629,#3392);
#2447=LINE('',#15631,#3393);
#2448=LINE('',#15633,#3394);
#2449=LINE('',#15634,#3395);
#2450=LINE('',#15636,#3396);
#2451=LINE('',#15637,#3397);
#2452=LINE('',#15641,#3398);
#2453=LINE('',#15643,#3399);
#2454=LINE('',#15649,#3400);
#2455=LINE('',#15712,#3401);
#2456=LINE('',#15713,#3402);
#2457=LINE('',#15716,#3403);
#2458=LINE('',#15717,#3404);
#2459=LINE('',#15720,#3405);
#2460=LINE('',#15721,#3406);
#2461=LINE('',#15725,#3407);
#2462=LINE('',#15726,#3408);
#2463=LINE('',#15729,#3409);
#2464=LINE('',#15731,#3410);
#2465=LINE('',#15732,#3411);
#2466=LINE('',#15735,#3412);
#2467=LINE('',#15737,#3413);
#2468=LINE('',#15738,#3414);
#2469=LINE('',#15741,#3415);
#2470=LINE('',#15743,#3416);
#2471=LINE('',#15744,#3417);
#2472=LINE('',#15746,#3418);
#2473=LINE('',#15749,#3419);
#2474=LINE('',#15751,#3420);
#2475=LINE('',#15752,#3421);
#2476=LINE('',#15754,#3422);
#2477=LINE('',#15757,#3423);
#2478=LINE('',#15759,#3424);
#2479=LINE('',#15760,#3425);
#2480=LINE('',#15762,#3426);
#2481=LINE('',#15764,#3427);
#2482=LINE('',#15765,#3428);
#2483=LINE('',#15767,#3429);
#2484=LINE('',#15768,#3430);
#2485=LINE('',#15772,#3431);
#2486=LINE('',#15774,#3432);
#2487=LINE('',#15780,#3433);
#2488=LINE('',#15843,#3434);
#2489=LINE('',#15844,#3435);
#2490=LINE('',#15847,#3436);
#2491=LINE('',#15848,#3437);
#2492=LINE('',#15851,#3438);
#2493=LINE('',#15852,#3439);
#2494=LINE('',#15856,#3440);
#2495=LINE('',#15857,#3441);
#2496=LINE('',#15860,#3442);
#2497=LINE('',#15862,#3443);
#2498=LINE('',#15863,#3444);
#2499=LINE('',#15866,#3445);
#2500=LINE('',#15868,#3446);
#2501=LINE('',#15869,#3447);
#2502=LINE('',#15872,#3448);
#2503=LINE('',#15874,#3449);
#2504=LINE('',#15875,#3450);
#2505=LINE('',#15877,#3451);
#2506=LINE('',#15880,#3452);
#2507=LINE('',#15882,#3453);
#2508=LINE('',#15883,#3454);
#2509=LINE('',#15885,#3455);
#2510=LINE('',#15888,#3456);
#2511=LINE('',#15890,#3457);
#2512=LINE('',#15891,#3458);
#2513=LINE('',#15893,#3459);
#2514=LINE('',#15895,#3460);
#2515=LINE('',#15896,#3461);
#2516=LINE('',#15898,#3462);
#2517=LINE('',#15899,#3463);
#2518=LINE('',#15903,#3464);
#2519=LINE('',#15905,#3465);
#2520=LINE('',#15910,#3466);
#2521=LINE('',#15961,#3467);
#2522=LINE('',#16039,#3468);
#2523=LINE('',#16115,#3469);
#2524=LINE('',#16191,#3470);
#2525=LINE('',#16267,#3471);
#2526=LINE('',#16343,#3472);
#2527=LINE('',#16421,#3473);
#2528=LINE('',#16499,#3474);
#2529=LINE('',#16575,#3475);
#2530=LINE('',#16651,#3476);
#2531=LINE('',#16727,#3477);
#2532=LINE('',#16803,#3478);
#2533=LINE('',#16879,#3479);
#2534=LINE('',#16957,#3480);
#2535=LINE('',#17035,#3481);
#2536=LINE('',#17111,#3482);
#2537=LINE('',#17187,#3483);
#2538=LINE('',#17263,#3484);
#2539=LINE('',#17339,#3485);
#2540=LINE('',#17374,#3486);
#2541=LINE('',#17452,#3487);
#2542=LINE('',#17528,#3488);
#2543=LINE('',#17604,#3489);
#2544=LINE('',#17680,#3490);
#2545=LINE('',#17756,#3491);
#2546=LINE('',#17832,#3492);
#2547=LINE('',#17912,#3493);
#2548=LINE('',#17988,#3494);
#2549=LINE('',#18064,#3495);
#2550=LINE('',#18140,#3496);
#2551=LINE('',#18216,#3497);
#2552=LINE('',#18292,#3498);
#2553=LINE('',#18370,#3499);
#2554=LINE('',#18448,#3500);
#2555=LINE('',#18524,#3501);
#2556=LINE('',#18600,#3502);
#2557=LINE('',#18676,#3503);
#2558=LINE('',#18752,#3504);
#2559=LINE('',#18766,#3505);
#2560=LINE('',#18844,#3506);
#2561=LINE('',#18920,#3507);
#2562=LINE('',#18996,#3508);
#2563=LINE('',#19072,#3509);
#2564=LINE('',#19148,#3510);
#2565=LINE('',#19224,#3511);
#2566=LINE('',#19302,#3512);
#2567=LINE('',#19380,#3513);
#2568=LINE('',#19456,#3514);
#2569=LINE('',#19532,#3515);
#2570=LINE('',#19608,#3516);
#2571=LINE('',#19684,#3517);
#2572=LINE('',#19762,#3518);
#2573=LINE('',#19840,#3519);
#2574=LINE('',#19916,#3520);
#2575=LINE('',#19992,#3521);
#2576=LINE('',#20068,#3522);
#2577=LINE('',#20144,#3523);
#2578=LINE('',#20215,#3524);
#2579=LINE('',#20291,#3525);
#2580=LINE('',#20367,#3526);
#2581=LINE('',#20443,#3527);
#2582=LINE('',#20519,#3528);
#2583=LINE('',#20595,#3529);
#2584=LINE('',#20673,#3530);
#2585=LINE('',#20751,#3531);
#2586=LINE('',#20827,#3532);
#2587=LINE('',#20903,#3533);
#2588=LINE('',#20979,#3534);
#2589=LINE('',#21055,#3535);
#2590=LINE('',#21131,#3536);
#2591=LINE('',#21211,#3537);
#2592=LINE('',#21287,#3538);
#2593=LINE('',#21363,#3539);
#2594=LINE('',#21439,#3540);
#2595=LINE('',#21515,#3541);
#2596=LINE('',#21535,#3542);
#2597=LINE('',#21595,#3543);
#2598=LINE('',#21671,#3544);
#2599=LINE('',#21747,#3545);
#2600=LINE('',#21823,#3546);
#2601=LINE('',#21901,#3547);
#2602=LINE('',#21938,#3548);
#2603=LINE('',#21974,#3549);
#2604=LINE('',#21994,#3550);
#2605=LINE('',#22054,#3551);
#2606=LINE('',#22130,#3552);
#2607=LINE('',#22206,#3553);
#2608=LINE('',#22282,#3554);
#2609=LINE('',#22360,#3555);
#2610=LINE('',#22397,#3556);
#2611=LINE('',#22433,#3557);
#2612=LINE('',#22453,#3558);
#2613=LINE('',#22513,#3559);
#2614=LINE('',#22589,#3560);
#2615=LINE('',#22665,#3561);
#2616=LINE('',#22741,#3562);
#2617=LINE('',#22819,#3563);
#2618=LINE('',#22856,#3564);
#2619=LINE('',#22892,#3565);
#2620=LINE('',#22912,#3566);
#2621=LINE('',#22972,#3567);
#2622=LINE('',#23048,#3568);
#2623=LINE('',#23124,#3569);
#2624=LINE('',#23200,#3570);
#2625=LINE('',#23278,#3571);
#2626=LINE('',#23315,#3572);
#2627=LINE('',#23836,#3573);
#2628=LINE('',#23842,#3574);
#2629=LINE('',#23848,#3575);
#2630=LINE('',#23852,#3576);
#2631=LINE('',#23914,#3577);
#2632=LINE('',#23976,#3578);
#2633=LINE('',#24038,#3579);
#2634=LINE('',#24100,#3580);
#2635=LINE('',#25043,#3581);
#2636=LINE('',#25684,#3582);
#2637=LINE('',#25987,#3583);
#2638=LINE('',#26633,#3584);
#2639=LINE('',#26635,#3585);
#2640=LINE('',#26637,#3586);
#2641=LINE('',#26639,#3587);
#2642=LINE('',#26641,#3588);
#2643=LINE('',#26643,#3589);
#2644=LINE('',#26645,#3590);
#2645=LINE('',#26646,#3591);
#2646=LINE('',#27593,#3592);
#2647=LINE('',#28233,#3593);
#2648=LINE('',#28536,#3594);
#2649=LINE('',#30119,#3595);
#2650=LINE('',#30759,#3596);
#2651=LINE('',#31062,#3597);
#2652=LINE('',#32645,#3598);
#2653=LINE('',#33285,#3599);
#2654=LINE('',#33588,#3600);
#2655=LINE('',#34235,#3601);
#2656=LINE('',#34237,#3602);
#2657=LINE('',#34238,#3603);
#2658=LINE('',#34241,#3604);
#2659=LINE('',#34242,#3605);
#2660=LINE('',#34247,#3606);
#2661=LINE('',#34251,#3607);
#2662=LINE('',#34252,#3608);
#2663=LINE('',#34255,#3609);
#2664=LINE('',#34256,#3610);
#2665=LINE('',#34260,#3611);
#2666=LINE('',#34263,#3612);
#2667=LINE('',#34264,#3613);
#2668=LINE('',#34268,#3614);
#2669=LINE('',#34271,#3615);
#2670=LINE('',#34272,#3616);
#2671=LINE('',#34276,#3617);
#2672=LINE('',#34279,#3618);
#2673=LINE('',#34280,#3619);
#2674=LINE('',#34284,#3620);
#2675=LINE('',#34286,#3621);
#2676=LINE('',#34290,#3622);
#2677=LINE('',#34294,#3623);
#2678=LINE('',#34296,#3624);
#2679=LINE('',#34301,#3625);
#2680=LINE('',#34319,#3626);
#2681=LINE('',#34324,#3627);
#2682=LINE('',#34326,#3628);
#2683=LINE('',#34329,#3629);
#2684=LINE('',#34333,#3630);
#2685=LINE('',#34339,#3631);
#2686=LINE('',#34345,#3632);
#2687=LINE('',#34351,#3633);
#2688=LINE('',#34357,#3634);
#2689=LINE('',#34363,#3635);
#2690=LINE('',#34368,#3636);
#2691=LINE('',#34372,#3637);
#2692=LINE('',#34376,#3638);
#2693=LINE('',#34380,#3639);
#2694=LINE('',#34385,#3640);
#2695=LINE('',#34394,#3641);
#2696=LINE('',#34396,#3642);
#2697=LINE('',#34398,#3643);
#2698=LINE('',#34399,#3644);
#2699=LINE('',#34403,#3645);
#2700=LINE('',#34404,#3646);
#2701=LINE('',#34405,#3647);
#2702=LINE('',#34408,#3648);
#2703=LINE('',#34409,#3649);
#2704=LINE('',#34412,#3650);
#2705=LINE('',#34413,#3651);
#2706=LINE('',#34415,#3652);
#2707=LINE('',#34419,#3653);
#2708=LINE('',#34421,#3654);
#2709=LINE('',#34423,#3655);
#2710=LINE('',#34424,#3656);
#2711=LINE('',#34427,#3657);
#2712=LINE('',#34429,#3658);
#2713=LINE('',#34430,#3659);
#2714=LINE('',#34434,#3660);
#2715=LINE('',#34436,#3661);
#2716=LINE('',#34438,#3662);
#2717=LINE('',#34440,#3663);
#2718=LINE('',#34442,#3664);
#2719=LINE('',#34444,#3665);
#2720=LINE('',#34446,#3666);
#2721=LINE('',#34447,#3667);
#2722=LINE('',#34453,#3668);
#2723=LINE('',#34457,#3669);
#2724=LINE('',#34461,#3670);
#2725=LINE('',#34464,#3671);
#2726=LINE('',#34466,#3672);
#2727=LINE('',#34467,#3673);
#2728=LINE('',#34471,#3674);
#2729=LINE('',#34474,#3675);
#2730=LINE('',#34475,#3676);
#2731=LINE('',#34479,#3677);
#2732=LINE('',#34482,#3678);
#2733=LINE('',#34483,#3679);
#2734=LINE('',#34487,#3680);
#2735=LINE('',#34490,#3681);
#2736=LINE('',#34491,#3682);
#2737=LINE('',#34495,#3683);
#2738=LINE('',#34498,#3684);
#2739=LINE('',#34499,#3685);
#2740=LINE('',#34502,#3686);
#2741=LINE('',#34503,#3687);
#2742=LINE('',#34508,#3688);
#2743=LINE('',#34509,#3689);
#2744=LINE('',#34512,#3690);
#2745=LINE('',#34513,#3691);
#2746=LINE('',#34516,#3692);
#2747=LINE('',#34519,#3693);
#2748=LINE('',#34520,#3694);
#2749=LINE('',#34523,#3695);
#2750=LINE('',#34524,#3696);
#2751=LINE('',#34526,#3697);
#2752=LINE('',#34533,#3698);
#2753=LINE('',#34539,#3699);
#2754=LINE('',#34545,#3700);
#2755=LINE('',#34551,#3701);
#2756=LINE('',#34557,#3702);
#2757=LINE('',#34562,#3703);
#2758=LINE('',#34564,#3704);
#2759=LINE('',#34566,#3705);
#2760=LINE('',#34568,#3706);
#2761=LINE('',#34570,#3707);
#2762=LINE('',#34572,#3708);
#2763=LINE('',#34574,#3709);
#2764=LINE('',#34575,#3710);
#2765=LINE('',#34579,#3711);
#2766=LINE('',#34581,#3712);
#2767=LINE('',#34583,#3713);
#2768=LINE('',#34585,#3714);
#2769=LINE('',#34587,#3715);
#2770=LINE('',#34589,#3716);
#2771=LINE('',#34591,#3717);
#2772=LINE('',#34592,#3718);
#2773=LINE('',#34594,#3719);
#2774=LINE('',#34595,#3720);
#2775=LINE('',#34597,#3721);
#2776=LINE('',#34599,#3722);
#2777=LINE('',#34601,#3723);
#2778=LINE('',#34602,#3724);
#2779=LINE('',#34604,#3725);
#2780=LINE('',#34605,#3726);
#2781=LINE('',#34619,#3727);
#2782=LINE('',#34624,#3728);
#2783=LINE('',#34630,#3729);
#2784=LINE('',#34636,#3730);
#2785=LINE('',#34642,#3731);
#2786=LINE('',#34648,#3732);
#2787=LINE('',#34657,#3733);
#2788=LINE('',#34663,#3734);
#2789=LINE('',#34668,#3735);
#2790=LINE('',#34674,#3736);
#2791=LINE('',#34684,#3737);
#2792=LINE('',#34695,#3738);
#2793=LINE('',#34716,#3739);
#2794=LINE('',#34726,#3740);
#2795=LINE('',#34732,#3741);
#2796=LINE('',#34741,#3742);
#2797=LINE('',#34744,#3743);
#2798=LINE('',#34750,#3744);
#2799=LINE('',#34759,#3745);
#2800=LINE('',#34764,#3746);
#2801=LINE('',#34771,#3747);
#2802=LINE('',#34774,#3748);
#2803=LINE('',#34782,#3749);
#2804=LINE('',#34792,#3750);
#2805=LINE('',#34796,#3751);
#2806=LINE('',#34804,#3752);
#2807=LINE('',#34811,#3753);
#2808=LINE('',#34814,#3754);
#2809=LINE('',#34820,#3755);
#2810=LINE('',#34830,#3756);
#2811=LINE('',#34835,#3757);
#2812=LINE('',#34888,#3758);
#2813=LINE('',#34890,#3759);
#2814=LINE('',#34892,#3760);
#2815=LINE('',#34893,#3761);
#2816=LINE('',#34897,#3762);
#2817=LINE('',#34899,#3763);
#2818=LINE('',#34901,#3764);
#2819=LINE('',#34902,#3765);
#2820=LINE('',#34906,#3766);
#2821=LINE('',#34908,#3767);
#2822=LINE('',#34910,#3768);
#2823=LINE('',#34911,#3769);
#2824=LINE('',#34915,#3770);
#2825=LINE('',#34917,#3771);
#2826=LINE('',#34919,#3772);
#2827=LINE('',#34920,#3773);
#2828=LINE('',#34924,#3774);
#2829=LINE('',#34926,#3775);
#2830=LINE('',#34928,#3776);
#2831=LINE('',#34929,#3777);
#2832=LINE('',#34934,#3778);
#2833=LINE('',#34939,#3779);
#2834=LINE('',#34941,#3780);
#2835=LINE('',#34943,#3781);
#2836=LINE('',#34944,#3782);
#2837=LINE('',#34948,#3783);
#2838=LINE('',#34950,#3784);
#2839=LINE('',#34952,#3785);
#2840=LINE('',#34953,#3786);
#2841=LINE('',#34955,#3787);
#2842=LINE('',#34956,#3788);
#2843=LINE('',#34959,#3789);
#2844=LINE('',#34961,#3790);
#2845=LINE('',#34962,#3791);
#2846=LINE('',#34965,#3792);
#2847=LINE('',#34967,#3793);
#2848=LINE('',#34968,#3794);
#2849=LINE('',#34971,#3795);
#2850=LINE('',#34973,#3796);
#2851=LINE('',#34974,#3797);
#2852=LINE('',#34977,#3798);
#2853=LINE('',#34979,#3799);
#2854=LINE('',#34980,#3800);
#2855=LINE('',#34983,#3801);
#2856=LINE('',#34985,#3802);
#2857=LINE('',#34986,#3803);
#2858=LINE('',#34989,#3804);
#2859=LINE('',#34991,#3805);
#2860=LINE('',#34992,#3806);
#2861=LINE('',#34997,#3807);
#2862=LINE('',#35001,#3808);
#2863=LINE('',#35003,#3809);
#2864=LINE('',#35004,#3810);
#2865=LINE('',#35007,#3811);
#2866=LINE('',#35009,#3812);
#2867=LINE('',#35010,#3813);
#2868=LINE('',#35013,#3814);
#2869=LINE('',#35015,#3815);
#2870=LINE('',#35016,#3816);
#2871=LINE('',#35018,#3817);
#2872=LINE('',#35019,#3818);
#2873=LINE('',#35023,#3819);
#2874=LINE('',#35025,#3820);
#2875=LINE('',#35027,#3821);
#2876=LINE('',#35028,#3822);
#2877=LINE('',#35030,#3823);
#2878=LINE('',#35031,#3824);
#2879=LINE('',#35033,#3825);
#2880=LINE('',#35034,#3826);
#2881=LINE('',#35038,#3827);
#2882=LINE('',#35040,#3828);
#2883=LINE('',#35042,#3829);
#2884=LINE('',#35043,#3830);
#2885=LINE('',#35046,#3831);
#2886=LINE('',#35048,#3832);
#2887=LINE('',#35049,#3833);
#2888=LINE('',#35051,#3834);
#2889=LINE('',#35052,#3835);
#2890=LINE('',#35056,#3836);
#2891=LINE('',#35058,#3837);
#2892=LINE('',#35060,#3838);
#2893=LINE('',#35061,#3839);
#2894=LINE('',#35063,#3840);
#2895=LINE('',#35064,#3841);
#2896=LINE('',#35067,#3842);
#2897=LINE('',#35069,#3843);
#2898=LINE('',#35070,#3844);
#2899=LINE('',#35073,#3845);
#2900=LINE('',#35075,#3846);
#2901=LINE('',#35076,#3847);
#2902=LINE('',#35079,#3848);
#2903=LINE('',#35081,#3849);
#2904=LINE('',#35082,#3850);
#2905=LINE('',#35085,#3851);
#2906=LINE('',#35087,#3852);
#2907=LINE('',#35088,#3853);
#2908=LINE('',#35091,#3854);
#2909=LINE('',#35093,#3855);
#2910=LINE('',#35094,#3856);
#2911=LINE('',#35097,#3857);
#2912=LINE('',#35099,#3858);
#2913=LINE('',#35100,#3859);
#2914=LINE('',#35105,#3860);
#2915=LINE('',#35109,#3861);
#2916=LINE('',#35111,#3862);
#2917=LINE('',#35112,#3863);
#2918=LINE('',#35115,#3864);
#2919=LINE('',#35117,#3865);
#2920=LINE('',#35118,#3866);
#2921=LINE('',#35121,#3867);
#2922=LINE('',#35123,#3868);
#2923=LINE('',#35124,#3869);
#2924=LINE('',#35126,#3870);
#2925=LINE('',#35127,#3871);
#2926=LINE('',#35129,#3872);
#2927=LINE('',#35130,#3873);
#2928=LINE('',#35133,#3874);
#2929=LINE('',#35135,#3875);
#2930=LINE('',#35136,#3876);
#2931=LINE('',#35139,#3877);
#2932=LINE('',#35141,#3878);
#2933=LINE('',#35142,#3879);
#2934=LINE('',#35145,#3880);
#2935=LINE('',#35147,#3881);
#2936=LINE('',#35148,#3882);
#2937=LINE('',#35151,#3883);
#2938=LINE('',#35153,#3884);
#2939=LINE('',#35154,#3885);
#2940=LINE('',#35157,#3886);
#2941=LINE('',#35159,#3887);
#2942=LINE('',#35160,#3888);
#2943=LINE('',#35163,#3889);
#2944=LINE('',#35165,#3890);
#2945=LINE('',#35166,#3891);
#2946=LINE('',#35169,#3892);
#2947=LINE('',#35171,#3893);
#2948=LINE('',#35172,#3894);
#2949=LINE('',#35175,#3895);
#2950=LINE('',#35177,#3896);
#2951=LINE('',#35179,#3897);
#2952=LINE('',#35181,#3898);
#2953=LINE('',#35183,#3899);
#2954=LINE('',#35185,#3900);
#2955=LINE('',#35187,#3901);
#2956=LINE('',#35189,#3902);
#2957=LINE('',#35191,#3903);
#2958=LINE('',#35193,#3904);
#2959=LINE('',#35195,#3905);
#2960=LINE('',#35197,#3906);
#2961=LINE('',#35199,#3907);
#2962=LINE('',#35201,#3908);
#2963=LINE('',#35205,#3909);
#2964=LINE('',#35207,#3910);
#2965=LINE('',#35209,#3911);
#2966=LINE('',#35211,#3912);
#2967=LINE('',#35213,#3913);
#2968=LINE('',#35215,#3914);
#2969=LINE('',#35217,#3915);
#2970=LINE('',#35219,#3916);
#2971=LINE('',#35221,#3917);
#2972=LINE('',#35223,#3918);
#2973=LINE('',#35225,#3919);
#2974=LINE('',#35227,#3920);
#2975=LINE('',#35229,#3921);
#2976=LINE('',#35233,#3922);
#2977=LINE('',#35235,#3923);
#2978=LINE('',#35237,#3924);
#2979=LINE('',#35239,#3925);
#2980=LINE('',#35241,#3926);
#2981=LINE('',#35243,#3927);
#2982=LINE('',#35245,#3928);
#2983=LINE('',#35247,#3929);
#2984=LINE('',#35249,#3930);
#2985=LINE('',#35251,#3931);
#2986=LINE('',#35253,#3932);
#2987=LINE('',#35254,#3933);
#2988=LINE('',#35256,#3934);
#2989=LINE('',#35258,#3935);
#2990=LINE('',#35260,#3936);
#2991=LINE('',#35262,#3937);
#2992=LINE('',#35263,#3938);
#2993=LINE('',#35268,#3939);
#2994=LINE('',#35269,#3940);
#2995=LINE('',#35272,#3941);
#2996=LINE('',#35273,#3942);
#2997=LINE('',#35276,#3943);
#2998=LINE('',#35278,#3944);
#2999=LINE('',#35279,#3945);
#3000=LINE('',#35282,#3946);
#3001=LINE('',#35284,#3947);
#3002=LINE('',#35285,#3948);
#3003=LINE('',#35288,#3949);
#3004=LINE('',#35290,#3950);
#3005=LINE('',#35291,#3951);
#3006=LINE('',#35294,#3952);
#3007=LINE('',#35298,#3953);
#3008=LINE('',#35300,#3954);
#3009=LINE('',#35301,#3955);
#3010=LINE('',#35304,#3956);
#3011=LINE('',#35306,#3957);
#3012=LINE('',#35307,#3958);
#3013=LINE('',#35309,#3959);
#3014=LINE('',#35312,#3960);
#3015=LINE('',#35313,#3961);
#3016=LINE('',#35316,#3962);
#3017=LINE('',#35317,#3963);
#3018=LINE('',#35320,#3964);
#3019=LINE('',#35321,#3965);
#3020=LINE('',#35324,#3966);
#3021=LINE('',#35325,#3967);
#3022=LINE('',#35328,#3968);
#3023=LINE('',#35329,#3969);
#3024=LINE('',#35332,#3970);
#3025=LINE('',#35333,#3971);
#3026=LINE('',#35337,#3972);
#3027=LINE('',#35340,#3973);
#3028=LINE('',#35341,#3974);
#3029=LINE('',#35344,#3975);
#3030=LINE('',#35345,#3976);
#3031=LINE('',#35348,#3977);
#3032=LINE('',#35349,#3978);
#3033=LINE('',#35351,#3979);
#3034=LINE('',#35354,#3980);
#3035=LINE('',#35356,#3981);
#3036=LINE('',#35357,#3982);
#3037=LINE('',#35359,#3983);
#3038=LINE('',#35361,#3984);
#3039=LINE('',#35364,#3985);
#3040=LINE('',#35365,#3986);
#3041=LINE('',#35368,#3987);
#3042=LINE('',#35369,#3988);
#3043=LINE('',#35372,#3989);
#3044=LINE('',#35373,#3990);
#3045=LINE('',#35375,#3991);
#3046=LINE('',#35378,#3992);
#3047=LINE('',#35380,#3993);
#3048=LINE('',#35381,#3994);
#3049=LINE('',#35383,#3995);
#3050=LINE('',#35386,#3996);
#3051=LINE('',#35387,#3997);
#3052=LINE('',#35390,#3998);
#3053=LINE('',#35391,#3999);
#3054=LINE('',#35394,#4000);
#3055=LINE('',#35395,#4001);
#3056=LINE('',#35398,#4002);
#3057=LINE('',#35399,#4003);
#3058=LINE('',#35402,#4004);
#3059=LINE('',#35403,#4005);
#3060=LINE('',#35406,#4006);
#3061=LINE('',#35407,#4007);
#3062=LINE('',#35411,#4008);
#3063=LINE('',#35414,#4009);
#3064=LINE('',#35415,#4010);
#3065=LINE('',#35418,#4011);
#3066=LINE('',#35419,#4012);
#3067=LINE('',#35422,#4013);
#3068=LINE('',#35423,#4014);
#3069=LINE('',#35425,#4015);
#3070=LINE('',#35427,#4016);
#3071=LINE('',#35430,#4017);
#3072=LINE('',#35431,#4018);
#3073=LINE('',#35434,#4019);
#3074=LINE('',#35435,#4020);
#3075=LINE('',#35438,#4021);
#3076=LINE('',#35439,#4022);
#3077=LINE('',#35442,#4023);
#3078=LINE('',#35443,#4024);
#3079=LINE('',#35446,#4025);
#3080=LINE('',#35447,#4026);
#3081=LINE('',#35449,#4027);
#3082=LINE('',#35461,#4028);
#3083=LINE('',#35471,#4029);
#3084=LINE('',#35474,#4030);
#3085=LINE('',#35479,#4031);
#3086=LINE('',#35485,#4032);
#3087=LINE('',#35490,#4033);
#3088=LINE('',#35492,#4034);
#3089=LINE('',#35494,#4035);
#3090=LINE('',#35495,#4036);
#3091=LINE('',#35498,#4037);
#3092=LINE('',#35500,#4038);
#3093=LINE('',#35501,#4039);
#3094=LINE('',#35504,#4040);
#3095=LINE('',#35506,#4041);
#3096=LINE('',#35507,#4042);
#3097=LINE('',#35509,#4043);
#3098=LINE('',#35510,#4044);
#3099=LINE('',#35514,#4045);
#3100=LINE('',#35516,#4046);
#3101=LINE('',#35518,#4047);
#3102=LINE('',#35519,#4048);
#3103=LINE('',#35522,#4049);
#3104=LINE('',#35524,#4050);
#3105=LINE('',#35525,#4051);
#3106=LINE('',#35528,#4052);
#3107=LINE('',#35530,#4053);
#3108=LINE('',#35531,#4054);
#3109=LINE('',#35533,#4055);
#3110=LINE('',#35534,#4056);
#3111=LINE('',#35539,#4057);
#3112=LINE('',#35545,#4058);
#3113=LINE('',#35550,#4059);
#3114=LINE('',#35552,#4060);
#3115=LINE('',#35554,#4061);
#3116=LINE('',#35555,#4062);
#3117=LINE('',#35558,#4063);
#3118=LINE('',#35560,#4064);
#3119=LINE('',#35561,#4065);
#3120=LINE('',#35564,#4066);
#3121=LINE('',#35566,#4067);
#3122=LINE('',#35567,#4068);
#3123=LINE('',#35569,#4069);
#3124=LINE('',#35570,#4070);
#3125=LINE('',#35575,#4071);
#3126=LINE('',#35581,#4072);
#3127=LINE('',#35586,#4073);
#3128=LINE('',#35588,#4074);
#3129=LINE('',#35590,#4075);
#3130=LINE('',#35591,#4076);
#3131=LINE('',#35594,#4077);
#3132=LINE('',#35596,#4078);
#3133=LINE('',#35597,#4079);
#3134=LINE('',#35600,#4080);
#3135=LINE('',#35602,#4081);
#3136=LINE('',#35603,#4082);
#3137=LINE('',#35606,#4083);
#3138=LINE('',#35608,#4084);
#3139=LINE('',#35609,#4085);
#3140=LINE('',#35612,#4086);
#3141=LINE('',#35614,#4087);
#3142=LINE('',#35615,#4088);
#3143=LINE('',#35618,#4089);
#3144=LINE('',#35620,#4090);
#3145=LINE('',#35621,#4091);
#3146=LINE('',#35624,#4092);
#3147=LINE('',#35626,#4093);
#3148=LINE('',#35627,#4094);
#3149=LINE('',#35630,#4095);
#3150=LINE('',#35632,#4096);
#3151=LINE('',#35633,#4097);
#3152=LINE('',#35636,#4098);
#3153=LINE('',#35638,#4099);
#3154=LINE('',#35639,#4100);
#3155=LINE('',#35645,#4101);
#3156=LINE('',#35648,#4102);
#3157=LINE('',#35650,#4103);
#3158=LINE('',#35651,#4104);
#3159=LINE('',#35657,#4105);
#3160=LINE('',#35660,#4106);
#3161=LINE('',#35662,#4107);
#3162=LINE('',#35663,#4108);
#3163=LINE('',#35669,#4109);
#3164=LINE('',#35672,#4110);
#3165=LINE('',#35674,#4111);
#3166=LINE('',#35675,#4112);
#3167=LINE('',#35719,#4113);
#3168=LINE('',#35797,#4114);
#3169=LINE('',#35841,#4115);
#3170=LINE('',#35843,#4116);
#3171=LINE('',#35856,#4117);
#3172=LINE('',#35860,#4118);
#3173=LINE('',#35865,#4119);
#3174=LINE('',#35866,#4120);
#3175=LINE('',#35871,#4121);
#3176=LINE('',#35881,#4122);
#3177=LINE('',#35884,#4123);
#3178=LINE('',#35889,#4124);
#3179=LINE('',#35892,#4125);
#3180=LINE('',#35895,#4126);
#3181=LINE('',#35897,#4127);
#3182=LINE('',#35898,#4128);
#3183=LINE('',#35902,#4129);
#3184=LINE('',#35905,#4130);
#3185=LINE('',#35906,#4131);
#3186=LINE('',#35911,#4132);
#3187=LINE('',#35913,#4133);
#3188=LINE('',#35914,#4134);
#3189=LINE('',#35918,#4135);
#3190=LINE('',#35921,#4136);
#3191=LINE('',#35922,#4137);
#3192=LINE('',#35931,#4138);
#3193=LINE('',#35936,#4139);
#3194=LINE('',#35938,#4140);
#3195=LINE('',#35940,#4141);
#3196=LINE('',#35941,#4142);
#3197=LINE('',#35947,#4143);
#3198=LINE('',#35950,#4144);
#3199=LINE('',#35952,#4145);
#3200=LINE('',#35953,#4146);
#3201=LINE('',#35961,#4147);
#3202=LINE('',#35967,#4148);
#3203=LINE('',#35973,#4149);
#3204=LINE('',#35979,#4150);
#3205=LINE('',#35985,#4151);
#3206=LINE('',#35990,#4152);
#3207=LINE('',#35992,#4153);
#3208=LINE('',#35994,#4154);
#3209=LINE('',#35995,#4155);
#3210=LINE('',#36001,#4156);
#3211=LINE('',#36004,#4157);
#3212=LINE('',#36006,#4158);
#3213=LINE('',#36007,#4159);
#3214=LINE('',#36014,#4160);
#3215=LINE('',#36016,#4161);
#3216=LINE('',#36018,#4162);
#3217=LINE('',#36019,#4163);
#3218=LINE('',#36025,#4164);
#3219=LINE('',#36028,#4165);
#3220=LINE('',#36030,#4166);
#3221=LINE('',#36031,#4167);
#3222=LINE('',#36039,#4168);
#3223=LINE('',#36045,#4169);
#3224=LINE('',#36051,#4170);
#3225=LINE('',#36057,#4171);
#3226=LINE('',#36063,#4172);
#3227=LINE('',#36068,#4173);
#3228=LINE('',#36070,#4174);
#3229=LINE('',#36072,#4175);
#3230=LINE('',#36073,#4176);
#3231=LINE('',#36079,#4177);
#3232=LINE('',#36082,#4178);
#3233=LINE('',#36084,#4179);
#3234=LINE('',#36085,#4180);
#3235=LINE('',#36093,#4181);
#3236=LINE('',#36099,#4182);
#3237=LINE('',#36104,#4183);
#3238=LINE('',#36106,#4184);
#3239=LINE('',#36108,#4185);
#3240=LINE('',#36109,#4186);
#3241=LINE('',#36115,#4187);
#3242=LINE('',#36118,#4188);
#3243=LINE('',#36120,#4189);
#3244=LINE('',#36121,#4190);
#3245=LINE('',#36128,#4191);
#3246=LINE('',#36130,#4192);
#3247=LINE('',#36132,#4193);
#3248=LINE('',#36133,#4194);
#3249=LINE('',#36139,#4195);
#3250=LINE('',#36142,#4196);
#3251=LINE('',#36144,#4197);
#3252=LINE('',#36145,#4198);
#3253=LINE('',#36152,#4199);
#3254=LINE('',#36154,#4200);
#3255=LINE('',#36156,#4201);
#3256=LINE('',#36157,#4202);
#3257=LINE('',#36163,#4203);
#3258=LINE('',#36166,#4204);
#3259=LINE('',#36168,#4205);
#3260=LINE('',#36169,#4206);
#3261=LINE('',#36176,#4207);
#3262=LINE('',#36178,#4208);
#3263=LINE('',#36180,#4209);
#3264=LINE('',#36181,#4210);
#3265=LINE('',#36187,#4211);
#3266=LINE('',#36190,#4212);
#3267=LINE('',#36192,#4213);
#3268=LINE('',#36193,#4214);
#3269=LINE('',#36201,#4215);
#3270=LINE('',#36207,#4216);
#3271=LINE('',#36212,#4217);
#3272=LINE('',#36214,#4218);
#3273=LINE('',#36216,#4219);
#3274=LINE('',#36217,#4220);
#3275=LINE('',#36223,#4221);
#3276=LINE('',#36226,#4222);
#3277=LINE('',#36228,#4223);
#3278=LINE('',#36229,#4224);
#3279=LINE('',#36235,#4225);
#3280=LINE('',#36238,#4226);
#3281=LINE('',#36240,#4227);
#3282=LINE('',#36241,#4228);
#3283=LINE('',#36247,#4229);
#3284=LINE('',#36250,#4230);
#3285=LINE('',#36252,#4231);
#3286=LINE('',#36253,#4232);
#3287=LINE('',#36264,#4233);
#3288=LINE('',#36270,#4234);
#3289=LINE('',#36276,#4235);
#3290=LINE('',#36282,#4236);
#3291=LINE('',#36288,#4237);
#3292=LINE('',#36295,#4238);
#3293=LINE('',#36298,#4239);
#3294=LINE('',#36301,#4240);
#3295=LINE('',#36303,#4241);
#3296=LINE('',#36304,#4242);
#3297=LINE('',#36310,#4243);
#3298=LINE('',#36313,#4244);
#3299=LINE('',#36315,#4245);
#3300=LINE('',#36316,#4246);
#3301=LINE('',#36322,#4247);
#3302=LINE('',#36325,#4248);
#3303=LINE('',#36327,#4249);
#3304=LINE('',#36328,#4250);
#3305=LINE('',#36334,#4251);
#3306=LINE('',#36336,#4252);
#3307=LINE('',#36337,#4253);
#3308=LINE('',#36345,#4254);
#3309=LINE('',#36357,#4255);
#3310=LINE('',#36361,#4256);
#3311=LINE('',#36363,#4257);
#3312=LINE('',#36364,#4258);
#3313=LINE('',#36367,#4259);
#3314=LINE('',#36368,#4260);
#3315=LINE('',#36371,#4261);
#3316=LINE('',#36372,#4262);
#3317=LINE('',#36375,#4263);
#3318=LINE('',#36376,#4264);
#3319=LINE('',#36379,#4265);
#3320=LINE('',#36380,#4266);
#3321=LINE('',#36382,#4267);
#3322=LINE('',#36386,#4268);
#3323=LINE('',#36387,#4269);
#3324=LINE('',#36388,#4270);
#3325=LINE('',#36391,#4271);
#3326=LINE('',#36392,#4272);
#3327=LINE('',#36395,#4273);
#3328=LINE('',#36396,#4274);
#3329=LINE('',#36399,#4275);
#3330=LINE('',#36400,#4276);
#3331=LINE('',#36403,#4277);
#3332=LINE('',#36404,#4278);
#3333=LINE('',#36406,#4279);
#3334=VECTOR('',#12445,3.175);
#3335=VECTOR('',#12480,1000.);
#3336=VECTOR('',#12481,1000.);
#3337=VECTOR('',#12484,1000.);
#3338=VECTOR('',#12485,1000.);
#3339=VECTOR('',#12488,1000.);
#3340=VECTOR('',#12489,1000.);
#3341=VECTOR('',#12494,1000.);
#3342=VECTOR('',#12495,1000.);
#3343=VECTOR('',#12498,1000.);
#3344=VECTOR('',#12499,1000.);
#3345=VECTOR('',#12500,1000.);
#3346=VECTOR('',#12503,1000.);
#3347=VECTOR('',#12504,1000.);
#3348=VECTOR('',#12505,1000.);
#3349=VECTOR('',#12508,1000.);
#3350=VECTOR('',#12509,1000.);
#3351=VECTOR('',#12510,1000.);
#3352=VECTOR('',#12513,1000.);
#3353=VECTOR('',#12516,1000.);
#3354=VECTOR('',#12517,1000.);
#3355=VECTOR('',#12518,1000.);
#3356=VECTOR('',#12521,1000.);
#3357=VECTOR('',#12524,1000.);
#3358=VECTOR('',#12525,1000.);
#3359=VECTOR('',#12526,1000.);
#3360=VECTOR('',#12527,1000.);
#3361=VECTOR('',#12528,1000.);
#3362=VECTOR('',#12529,1000.);
#3363=VECTOR('',#12532,1000.);
#3364=VECTOR('',#12533,1000.);
#3365=VECTOR('',#12540,1000.);
#3366=VECTOR('',#12543,1000.);
#3367=VECTOR('',#12550,3.175);
#3368=VECTOR('',#12585,1000.);
#3369=VECTOR('',#12586,1000.);
#3370=VECTOR('',#12589,1000.);
#3371=VECTOR('',#12590,1000.);
#3372=VECTOR('',#12593,1000.);
#3373=VECTOR('',#12594,1000.);
#3374=VECTOR('',#12599,1000.);
#3375=VECTOR('',#12600,1000.);
#3376=VECTOR('',#12603,1000.);
#3377=VECTOR('',#12604,1000.);
#3378=VECTOR('',#12605,1000.);
#3379=VECTOR('',#12608,1000.);
#3380=VECTOR('',#12609,1000.);
#3381=VECTOR('',#12610,1000.);
#3382=VECTOR('',#12613,1000.);
#3383=VECTOR('',#12614,1000.);
#3384=VECTOR('',#12615,1000.);
#3385=VECTOR('',#12618,1000.);
#3386=VECTOR('',#12621,1000.);
#3387=VECTOR('',#12622,1000.);
#3388=VECTOR('',#12623,1000.);
#3389=VECTOR('',#12626,1000.);
#3390=VECTOR('',#12629,1000.);
#3391=VECTOR('',#12630,1000.);
#3392=VECTOR('',#12631,1000.);
#3393=VECTOR('',#12632,1000.);
#3394=VECTOR('',#12633,1000.);
#3395=VECTOR('',#12634,1000.);
#3396=VECTOR('',#12637,1000.);
#3397=VECTOR('',#12638,1000.);
#3398=VECTOR('',#12645,1000.);
#3399=VECTOR('',#12648,1000.);
#3400=VECTOR('',#12655,3.175);
#3401=VECTOR('',#12690,1000.);
#3402=VECTOR('',#12691,1000.);
#3403=VECTOR('',#12694,1000.);
#3404=VECTOR('',#12695,1000.);
#3405=VECTOR('',#12698,1000.);
#3406=VECTOR('',#12699,1000.);
#3407=VECTOR('',#12704,1000.);
#3408=VECTOR('',#12705,1000.);
#3409=VECTOR('',#12708,1000.);
#3410=VECTOR('',#12709,1000.);
#3411=VECTOR('',#12710,1000.);
#3412=VECTOR('',#12713,1000.);
#3413=VECTOR('',#12714,1000.);
#3414=VECTOR('',#12715,1000.);
#3415=VECTOR('',#12718,1000.);
#3416=VECTOR('',#12719,1000.);
#3417=VECTOR('',#12720,1000.);
#3418=VECTOR('',#12723,1000.);
#3419=VECTOR('',#12726,1000.);
#3420=VECTOR('',#12727,1000.);
#3421=VECTOR('',#12728,1000.);
#3422=VECTOR('',#12731,1000.);
#3423=VECTOR('',#12734,1000.);
#3424=VECTOR('',#12735,1000.);
#3425=VECTOR('',#12736,1000.);
#3426=VECTOR('',#12737,1000.);
#3427=VECTOR('',#12738,1000.);
#3428=VECTOR('',#12739,1000.);
#3429=VECTOR('',#12742,1000.);
#3430=VECTOR('',#12743,1000.);
#3431=VECTOR('',#12750,1000.);
#3432=VECTOR('',#12753,1000.);
#3433=VECTOR('',#12760,3.175);
#3434=VECTOR('',#12795,1000.);
#3435=VECTOR('',#12796,1000.);
#3436=VECTOR('',#12799,1000.);
#3437=VECTOR('',#12800,1000.);
#3438=VECTOR('',#12803,1000.);
#3439=VECTOR('',#12804,1000.);
#3440=VECTOR('',#12809,1000.);
#3441=VECTOR('',#12810,1000.);
#3442=VECTOR('',#12813,1000.);
#3443=VECTOR('',#12814,1000.);
#3444=VECTOR('',#12815,1000.);
#3445=VECTOR('',#12818,1000.);
#3446=VECTOR('',#12819,1000.);
#3447=VECTOR('',#12820,1000.);
#3448=VECTOR('',#12823,1000.);
#3449=VECTOR('',#12824,1000.);
#3450=VECTOR('',#12825,1000.);
#3451=VECTOR('',#12828,1000.);
#3452=VECTOR('',#12831,1000.);
#3453=VECTOR('',#12832,1000.);
#3454=VECTOR('',#12833,1000.);
#3455=VECTOR('',#12836,1000.);
#3456=VECTOR('',#12839,1000.);
#3457=VECTOR('',#12840,1000.);
#3458=VECTOR('',#12841,1000.);
#3459=VECTOR('',#12842,1000.);
#3460=VECTOR('',#12843,1000.);
#3461=VECTOR('',#12844,1000.);
#3462=VECTOR('',#12847,1000.);
#3463=VECTOR('',#12848,1000.);
#3464=VECTOR('',#12855,1000.);
#3465=VECTOR('',#12858,1000.);
#3466=VECTOR('',#12863,1.905);
#3467=VECTOR('',#12868,1.905);
#3468=VECTOR('',#12871,1.905);
#3469=VECTOR('',#12874,1.905);
#3470=VECTOR('',#12877,1.905);
#3471=VECTOR('',#12880,1.905);
#3472=VECTOR('',#12883,1.905);
#3473=VECTOR('',#12886,1.905);
#3474=VECTOR('',#12889,1.905);
#3475=VECTOR('',#12892,1.905);
#3476=VECTOR('',#12895,1.905);
#3477=VECTOR('',#12898,1.905);
#3478=VECTOR('',#12901,1.905);
#3479=VECTOR('',#12904,1.905);
#3480=VECTOR('',#12907,1.905);
#3481=VECTOR('',#12910,1.905);
#3482=VECTOR('',#12913,1.905);
#3483=VECTOR('',#12916,1.905);
#3484=VECTOR('',#12919,1.905);
#3485=VECTOR('',#12922,1.905);
#3486=VECTOR('',#12927,1.905);
#3487=VECTOR('',#12930,1.905);
#3488=VECTOR('',#12933,1.905);
#3489=VECTOR('',#12936,1.905);
#3490=VECTOR('',#12939,1.905);
#3491=VECTOR('',#12942,1.905);
#3492=VECTOR('',#12945,1.905);
#3493=VECTOR('',#12948,1.905);
#3494=VECTOR('',#12951,1.905);
#3495=VECTOR('',#12954,1.905);
#3496=VECTOR('',#12957,1.905);
#3497=VECTOR('',#12960,1.905);
#3498=VECTOR('',#12963,1.905);
#3499=VECTOR('',#12966,1.905);
#3500=VECTOR('',#12969,1.905);
#3501=VECTOR('',#12972,1.905);
#3502=VECTOR('',#12975,1.905);
#3503=VECTOR('',#12978,1.905);
#3504=VECTOR('',#12981,1.905);
#3505=VECTOR('',#12986,1.905);
#3506=VECTOR('',#12989,1.905);
#3507=VECTOR('',#12992,1.905);
#3508=VECTOR('',#12995,1.905);
#3509=VECTOR('',#12998,1.905);
#3510=VECTOR('',#13001,1.905);
#3511=VECTOR('',#13004,1.905);
#3512=VECTOR('',#13007,1.905);
#3513=VECTOR('',#13010,1.905);
#3514=VECTOR('',#13013,1.905);
#3515=VECTOR('',#13016,1.905);
#3516=VECTOR('',#13019,1.905);
#3517=VECTOR('',#13022,1.905);
#3518=VECTOR('',#13025,1.905);
#3519=VECTOR('',#13028,1.905);
#3520=VECTOR('',#13031,1.905);
#3521=VECTOR('',#13034,1.905);
#3522=VECTOR('',#13037,1.905);
#3523=VECTOR('',#13040,1.905);
#3524=VECTOR('',#13045,1.905);
#3525=VECTOR('',#13048,1.905);
#3526=VECTOR('',#13051,1.905);
#3527=VECTOR('',#13054,1.905);
#3528=VECTOR('',#13057,1.905);
#3529=VECTOR('',#13060,1.905);
#3530=VECTOR('',#13063,1.905);
#3531=VECTOR('',#13066,1.905);
#3532=VECTOR('',#13069,1.905);
#3533=VECTOR('',#13072,1.905);
#3534=VECTOR('',#13075,1.905);
#3535=VECTOR('',#13078,1.905);
#3536=VECTOR('',#13081,1.905);
#3537=VECTOR('',#13084,1.905);
#3538=VECTOR('',#13087,1.905);
#3539=VECTOR('',#13090,1.905);
#3540=VECTOR('',#13093,1.905);
#3541=VECTOR('',#13096,1.93206329386826);
#3542=VECTOR('',#13101,1.93206329386826);
#3543=VECTOR('',#13106,1.93206329386826);
#3544=VECTOR('',#13109,1.93206329386826);
#3545=VECTOR('',#13112,1.93206329386826);
#3546=VECTOR('',#13115,1.93206329386826);
#3547=VECTOR('',#13118,1.93206329386826);
#3548=VECTOR('',#13119,10.);
#3549=VECTOR('',#13122,1.93206329386825);
#3550=VECTOR('',#13127,1.93206329386825);
#3551=VECTOR('',#13132,1.93206329386825);
#3552=VECTOR('',#13135,1.93206329386825);
#3553=VECTOR('',#13138,1.93206329386825);
#3554=VECTOR('',#13141,1.93206329386825);
#3555=VECTOR('',#13144,1.93206329386825);
#3556=VECTOR('',#13145,10.);
#3557=VECTOR('',#13148,1.93206329386826);
#3558=VECTOR('',#13153,1.93206329386826);
#3559=VECTOR('',#13158,1.93206329386826);
#3560=VECTOR('',#13161,1.93206329386826);
#3561=VECTOR('',#13164,1.93206329386826);
#3562=VECTOR('',#13167,1.93206329386826);
#3563=VECTOR('',#13170,1.93206329386826);
#3564=VECTOR('',#13171,10.);
#3565=VECTOR('',#13174,1.93206329386822);
#3566=VECTOR('',#13179,1.93206329386822);
#3567=VECTOR('',#13184,1.93206329386822);
#3568=VECTOR('',#13187,1.93206329386822);
#3569=VECTOR('',#13190,1.93206329386822);
#3570=VECTOR('',#13193,1.93206329386822);
#3571=VECTOR('',#13196,1.93206329386822);
#3572=VECTOR('',#13197,10.);
#3573=VECTOR('',#13226,2.62699999999999);
#3574=VECTOR('',#13233,3.76999999999999);
#3575=VECTOR('',#13240,10.985);
#3576=VECTOR('',#13245,10.985);
#3577=VECTOR('',#13252,2.155);
#3578=VECTOR('',#13259,2.155);
#3579=VECTOR('',#13266,2.155);
#3580=VECTOR('',#13273,2.155);
#3581=VECTOR('',#13278,10.);
#3582=VECTOR('',#13281,10.);
#3583=VECTOR('',#13284,10.);
#3584=VECTOR('',#13287,1000.);
#3585=VECTOR('',#13288,1000.);
#3586=VECTOR('',#13289,1000.);
#3587=VECTOR('',#13290,1000.);
#3588=VECTOR('',#13291,1000.);
#3589=VECTOR('',#13292,1000.);
#3590=VECTOR('',#13293,1000.);
#3591=VECTOR('',#13294,1000.);
#3592=VECTOR('',#13307,9.99999999999999);
#3593=VECTOR('',#13308,10.);
#3594=VECTOR('',#13311,10.);
#3595=VECTOR('',#13312,10.);
#3596=VECTOR('',#13313,10.);
#3597=VECTOR('',#13316,10.);
#3598=VECTOR('',#13317,9.99999999999999);
#3599=VECTOR('',#13318,10.);
#3600=VECTOR('',#13321,10.);
#3601=VECTOR('',#13328,1000.);
#3602=VECTOR('',#13329,1000.);
#3603=VECTOR('',#13330,1000.);
#3604=VECTOR('',#13333,1000.);
#3605=VECTOR('',#13334,1000.);
#3606=VECTOR('',#13339,1000.);
#3607=VECTOR('',#13344,1000.);
#3608=VECTOR('',#13345,1000.);
#3609=VECTOR('',#13348,1000.);
#3610=VECTOR('',#13349,1000.);
#3611=VECTOR('',#13354,1000.);
#3612=VECTOR('',#13357,1000.);
#3613=VECTOR('',#13358,1000.);
#3614=VECTOR('',#13363,1000.);
#3615=VECTOR('',#13366,1000.);
#3616=VECTOR('',#13367,1000.);
#3617=VECTOR('',#13372,1000.);
#3618=VECTOR('',#13375,1000.);
#3619=VECTOR('',#13376,1000.);
#3620=VECTOR('',#13381,1000.);
#3621=VECTOR('',#13384,1000.);
#3622=VECTOR('',#13389,1000.);
#3623=VECTOR('',#13394,1000.);
#3624=VECTOR('',#13397,1000.);
#3625=VECTOR('',#13402,1.99200000000004);
#3626=VECTOR('',#13415,0.975999999999995);
#3627=VECTOR('',#13422,2.5);
#3628=VECTOR('',#13423,1000.);
#3629=VECTOR('',#13426,1000.);
#3630=VECTOR('',#13433,1000.);
#3631=VECTOR('',#13440,5.16699999999999);
#3632=VECTOR('',#13447,3.175);
#3633=VECTOR('',#13454,3.175);
#3634=VECTOR('',#13461,3.175);
#3635=VECTOR('',#13468,3.175);
#3636=VECTOR('',#13475,3.175);
#3637=VECTOR('',#13480,3.175);
#3638=VECTOR('',#13485,3.175);
#3639=VECTOR('',#13490,3.175);
#3640=VECTOR('',#13495,2.62699999999999);
#3641=VECTOR('',#13508,1000.);
#3642=VECTOR('',#13509,1000.);
#3643=VECTOR('',#13510,1000.);
#3644=VECTOR('',#13511,1000.);
#3645=VECTOR('',#13514,1000.);
#3646=VECTOR('',#13515,1000.);
#3647=VECTOR('',#13516,1000.);
#3648=VECTOR('',#13519,1000.);
#3649=VECTOR('',#13520,1000.);
#3650=VECTOR('',#13523,1000.);
#3651=VECTOR('',#13524,1000.);
#3652=VECTOR('',#13527,1000.);
#3653=VECTOR('',#13530,1000.);
#3654=VECTOR('',#13531,1000.);
#3655=VECTOR('',#13532,1000.);
#3656=VECTOR('',#13533,1000.);
#3657=VECTOR('',#13536,1000.);
#3658=VECTOR('',#13537,1000.);
#3659=VECTOR('',#13538,1000.);
#3660=VECTOR('',#13541,1000.);
#3661=VECTOR('',#13542,1000.);
#3662=VECTOR('',#13543,1000.);
#3663=VECTOR('',#13544,1000.);
#3664=VECTOR('',#13545,1000.);
#3665=VECTOR('',#13546,1000.);
#3666=VECTOR('',#13547,1000.);
#3667=VECTOR('',#13548,1000.);
#3668=VECTOR('',#13555,1000.);
#3669=VECTOR('',#13560,1000.);
#3670=VECTOR('',#13565,1000.);
#3671=VECTOR('',#13568,1000.);
#3672=VECTOR('',#13569,1000.);
#3673=VECTOR('',#13570,1000.);
#3674=VECTOR('',#13575,1000.);
#3675=VECTOR('',#13578,1000.);
#3676=VECTOR('',#13579,1000.);
#3677=VECTOR('',#13584,1000.);
#3678=VECTOR('',#13587,1000.);
#3679=VECTOR('',#13588,1000.);
#3680=VECTOR('',#13593,1000.);
#3681=VECTOR('',#13596,1000.);
#3682=VECTOR('',#13597,1000.);
#3683=VECTOR('',#13602,1000.);
#3684=VECTOR('',#13605,1000.);
#3685=VECTOR('',#13606,1000.);
#3686=VECTOR('',#13609,1000.);
#3687=VECTOR('',#13610,1000.);
#3688=VECTOR('',#13615,1000.);
#3689=VECTOR('',#13616,1000.);
#3690=VECTOR('',#13619,1000.);
#3691=VECTOR('',#13620,1000.);
#3692=VECTOR('',#13623,1000.);
#3693=VECTOR('',#13628,1000.);
#3694=VECTOR('',#13629,1000.);
#3695=VECTOR('',#13632,1000.);
#3696=VECTOR('',#13633,1000.);
#3697=VECTOR('',#13636,1000.);
#3698=VECTOR('',#13645,2.62699999999999);
#3699=VECTOR('',#13652,1.905);
#3700=VECTOR('',#13659,1.905);
#3701=VECTOR('',#13666,1.905);
#3702=VECTOR('',#13673,1.905);
#3703=VECTOR('',#13678,1000.);
#3704=VECTOR('',#13679,1000.);
#3705=VECTOR('',#13680,1000.);
#3706=VECTOR('',#13681,1000.);
#3707=VECTOR('',#13682,1000.);
#3708=VECTOR('',#13683,1000.);
#3709=VECTOR('',#13684,1000.);
#3710=VECTOR('',#13685,1000.);
#3711=VECTOR('',#13688,1000.);
#3712=VECTOR('',#13689,1000.);
#3713=VECTOR('',#13690,1000.);
#3714=VECTOR('',#13691,1000.);
#3715=VECTOR('',#13692,1000.);
#3716=VECTOR('',#13693,1000.);
#3717=VECTOR('',#13694,1000.);
#3718=VECTOR('',#13695,1000.);
#3719=VECTOR('',#13698,1000.);
#3720=VECTOR('',#13699,1000.);
#3721=VECTOR('',#13702,1000.);
#3722=VECTOR('',#13705,1000.);
#3723=VECTOR('',#13708,1000.);
#3724=VECTOR('',#13709,1000.);
#3725=VECTOR('',#13712,1000.);
#3726=VECTOR('',#13713,1000.);
#3727=VECTOR('',#13736,10.9505);
#3728=VECTOR('',#13743,11.9505);
#3729=VECTOR('',#13750,10.9505);
#3730=VECTOR('',#13759,8.00000000000001);
#3731=VECTOR('',#13766,2.5);
#3732=VECTOR('',#13773,4.49999999999999);
#3733=VECTOR('',#13786,2.110288568297);
#3734=VECTOR('',#13793,2.110288568297);
#3735=VECTOR('',#13798,10.);
#3736=VECTOR('',#13799,10.);
#3737=VECTOR('',#13802,10.);
#3738=VECTOR('',#13805,4.27);
#3739=VECTOR('',#13810,10.);
#3740=VECTOR('',#13813,10.);
#3741=VECTOR('',#13816,10.);
#3742=VECTOR('',#13825,4.27);
#3743=VECTOR('',#13830,2.117);
#3744=VECTOR('',#13837,5.73351648351648);
#3745=VECTOR('',#13850,5.73351648351648);
#3746=VECTOR('',#13855,7.75);
#3747=VECTOR('',#13864,8.);
#3748=VECTOR('',#13867,8.);
#3749=VECTOR('',#13878,4.76648351648352);
#3750=VECTOR('',#13891,3.26912128048043);
#3751=VECTOR('',#13896,4.01780239848197);
#3752=VECTOR('',#13907,3.26912128048043);
#3753=VECTOR('',#13916,2.5);
#3754=VECTOR('',#13919,2.5);
#3755=VECTOR('',#13926,4.76648351648352);
#3756=VECTOR('',#13939,3.26912128048043);
#3757=VECTOR('',#13946,3.26912128048043);
#3758=VECTOR('',#14007,10.);
#3759=VECTOR('',#14008,10.);
#3760=VECTOR('',#14009,10.);
#3761=VECTOR('',#14010,10.);
#3762=VECTOR('',#14013,10.);
#3763=VECTOR('',#14014,10.);
#3764=VECTOR('',#14015,10.);
#3765=VECTOR('',#14016,10.);
#3766=VECTOR('',#14019,10.);
#3767=VECTOR('',#14020,10.);
#3768=VECTOR('',#14021,10.);
#3769=VECTOR('',#14022,10.);
#3770=VECTOR('',#14025,10.);
#3771=VECTOR('',#14026,10.);
#3772=VECTOR('',#14027,10.);
#3773=VECTOR('',#14028,10.);
#3774=VECTOR('',#14031,10.);
#3775=VECTOR('',#14032,10.);
#3776=VECTOR('',#14033,10.);
#3777=VECTOR('',#14034,10.);
#3778=VECTOR('',#14039,2.1);
#3779=VECTOR('',#14044,10.);
#3780=VECTOR('',#14045,10.);
#3781=VECTOR('',#14046,10.);
#3782=VECTOR('',#14047,10.);
#3783=VECTOR('',#14050,10.);
#3784=VECTOR('',#14051,10.);
#3785=VECTOR('',#14052,10.);
#3786=VECTOR('',#14053,10.);
#3787=VECTOR('',#14056,10.);
#3788=VECTOR('',#14057,10.);
#3789=VECTOR('',#14060,10.);
#3790=VECTOR('',#14061,10.);
#3791=VECTOR('',#14062,10.);
#3792=VECTOR('',#14065,10.);
#3793=VECTOR('',#14066,10.);
#3794=VECTOR('',#14067,10.);
#3795=VECTOR('',#14070,10.);
#3796=VECTOR('',#14071,10.);
#3797=VECTOR('',#14072,10.);
#3798=VECTOR('',#14075,10.);
#3799=VECTOR('',#14076,10.);
#3800=VECTOR('',#14077,10.);
#3801=VECTOR('',#14080,10.);
#3802=VECTOR('',#14081,10.);
#3803=VECTOR('',#14082,10.);
#3804=VECTOR('',#14085,10.);
#3805=VECTOR('',#14086,10.);
#3806=VECTOR('',#14087,10.);
#3807=VECTOR('',#14092,10.);
#3808=VECTOR('',#14097,10.);
#3809=VECTOR('',#14098,10.);
#3810=VECTOR('',#14099,10.);
#3811=VECTOR('',#14102,10.);
#3812=VECTOR('',#14103,10.);
#3813=VECTOR('',#14104,10.);
#3814=VECTOR('',#14107,10.);
#3815=VECTOR('',#14108,10.);
#3816=VECTOR('',#14109,10.);
#3817=VECTOR('',#14112,10.);
#3818=VECTOR('',#14113,10.);
#3819=VECTOR('',#14116,10.);
#3820=VECTOR('',#14117,10.);
#3821=VECTOR('',#14118,10.);
#3822=VECTOR('',#14119,10.);
#3823=VECTOR('',#14122,10.);
#3824=VECTOR('',#14123,10.);
#3825=VECTOR('',#14126,10.);
#3826=VECTOR('',#14127,10.);
#3827=VECTOR('',#14130,10.);
#3828=VECTOR('',#14131,10.);
#3829=VECTOR('',#14132,10.);
#3830=VECTOR('',#14133,10.);
#3831=VECTOR('',#14136,10.);
#3832=VECTOR('',#14137,10.);
#3833=VECTOR('',#14138,10.);
#3834=VECTOR('',#14141,10.);
#3835=VECTOR('',#14142,10.);
#3836=VECTOR('',#14145,10.);
#3837=VECTOR('',#14146,10.);
#3838=VECTOR('',#14147,10.);
#3839=VECTOR('',#14148,10.);
#3840=VECTOR('',#14151,10.);
#3841=VECTOR('',#14152,10.);
#3842=VECTOR('',#14155,10.);
#3843=VECTOR('',#14156,10.);
#3844=VECTOR('',#14157,10.);
#3845=VECTOR('',#14160,10.);
#3846=VECTOR('',#14161,10.);
#3847=VECTOR('',#14162,10.);
#3848=VECTOR('',#14165,10.);
#3849=VECTOR('',#14166,10.);
#3850=VECTOR('',#14167,10.);
#3851=VECTOR('',#14170,10.);
#3852=VECTOR('',#14171,10.);
#3853=VECTOR('',#14172,10.);
#3854=VECTOR('',#14175,10.);
#3855=VECTOR('',#14176,10.);
#3856=VECTOR('',#14177,10.);
#3857=VECTOR('',#14180,10.);
#3858=VECTOR('',#14181,10.);
#3859=VECTOR('',#14182,10.);
#3860=VECTOR('',#14187,10.);
#3861=VECTOR('',#14192,10.);
#3862=VECTOR('',#14193,10.);
#3863=VECTOR('',#14194,10.);
#3864=VECTOR('',#14197,10.);
#3865=VECTOR('',#14198,10.);
#3866=VECTOR('',#14199,10.);
#3867=VECTOR('',#14202,10.);
#3868=VECTOR('',#14203,10.);
#3869=VECTOR('',#14204,10.);
#3870=VECTOR('',#14207,10.);
#3871=VECTOR('',#14208,10.);
#3872=VECTOR('',#14211,10.);
#3873=VECTOR('',#14212,10.);
#3874=VECTOR('',#14215,10.);
#3875=VECTOR('',#14216,10.);
#3876=VECTOR('',#14217,10.);
#3877=VECTOR('',#14220,10.);
#3878=VECTOR('',#14221,10.);
#3879=VECTOR('',#14222,10.);
#3880=VECTOR('',#14225,10.);
#3881=VECTOR('',#14226,10.);
#3882=VECTOR('',#14227,10.);
#3883=VECTOR('',#14230,10.);
#3884=VECTOR('',#14231,10.);
#3885=VECTOR('',#14232,10.);
#3886=VECTOR('',#14235,10.);
#3887=VECTOR('',#14236,10.);
#3888=VECTOR('',#14237,10.);
#3889=VECTOR('',#14240,10.);
#3890=VECTOR('',#14241,10.);
#3891=VECTOR('',#14242,10.);
#3892=VECTOR('',#14245,10.);
#3893=VECTOR('',#14246,10.);
#3894=VECTOR('',#14247,10.);
#3895=VECTOR('',#14250,10.);
#3896=VECTOR('',#14251,10.);
#3897=VECTOR('',#14252,10.);
#3898=VECTOR('',#14253,10.);
#3899=VECTOR('',#14254,10.);
#3900=VECTOR('',#14255,10.);
#3901=VECTOR('',#14256,10.);
#3902=VECTOR('',#14257,10.);
#3903=VECTOR('',#14258,10.);
#3904=VECTOR('',#14259,10.);
#3905=VECTOR('',#14260,10.);
#3906=VECTOR('',#14261,10.);
#3907=VECTOR('',#14262,10.);
#3908=VECTOR('',#14263,10.);
#3909=VECTOR('',#14266,10.);
#3910=VECTOR('',#14267,10.);
#3911=VECTOR('',#14268,10.);
#3912=VECTOR('',#14269,10.);
#3913=VECTOR('',#14270,10.);
#3914=VECTOR('',#14271,10.);
#3915=VECTOR('',#14272,10.);
#3916=VECTOR('',#14273,10.);
#3917=VECTOR('',#14274,10.);
#3918=VECTOR('',#14275,10.);
#3919=VECTOR('',#14276,10.);
#3920=VECTOR('',#14277,10.);
#3921=VECTOR('',#14278,10.);
#3922=VECTOR('',#14281,10.);
#3923=VECTOR('',#14282,10.);
#3924=VECTOR('',#14283,10.);
#3925=VECTOR('',#14284,10.);
#3926=VECTOR('',#14285,10.);
#3927=VECTOR('',#14286,10.);
#3928=VECTOR('',#14287,10.);
#3929=VECTOR('',#14288,10.);
#3930=VECTOR('',#14289,10.);
#3931=VECTOR('',#14290,10.);
#3932=VECTOR('',#14291,10.);
#3933=VECTOR('',#14292,10.);
#3934=VECTOR('',#14293,10.);
#3935=VECTOR('',#14294,10.);
#3936=VECTOR('',#14295,10.);
#3937=VECTOR('',#14296,10.);
#3938=VECTOR('',#14297,10.);
#3939=VECTOR('',#14302,10.);
#3940=VECTOR('',#14303,10.);
#3941=VECTOR('',#14306,10.);
#3942=VECTOR('',#14307,10.);
#3943=VECTOR('',#14310,10.);
#3944=VECTOR('',#14311,10.);
#3945=VECTOR('',#14312,10.);
#3946=VECTOR('',#14315,10.);
#3947=VECTOR('',#14316,10.);
#3948=VECTOR('',#14317,10.);
#3949=VECTOR('',#14320,10.);
#3950=VECTOR('',#14321,10.);
#3951=VECTOR('',#14322,10.);
#3952=VECTOR('',#14325,2.1);
#3953=VECTOR('',#14330,10.);
#3954=VECTOR('',#14331,10.);
#3955=VECTOR('',#14332,10.);
#3956=VECTOR('',#14335,10.);
#3957=VECTOR('',#14336,10.);
#3958=VECTOR('',#14337,10.);
#3959=VECTOR('',#14340,10.);
#3960=VECTOR('',#14343,10.);
#3961=VECTOR('',#14344,10.);
#3962=VECTOR('',#14347,10.);
#3963=VECTOR('',#14348,10.);
#3964=VECTOR('',#14351,10.);
#3965=VECTOR('',#14352,10.);
#3966=VECTOR('',#14355,10.);
#3967=VECTOR('',#14356,10.);
#3968=VECTOR('',#14359,10.);
#3969=VECTOR('',#14360,10.);
#3970=VECTOR('',#14363,10.);
#3971=VECTOR('',#14364,10.);
#3972=VECTOR('',#14369,10.);
#3973=VECTOR('',#14372,10.);
#3974=VECTOR('',#14373,10.);
#3975=VECTOR('',#14376,10.);
#3976=VECTOR('',#14377,10.);
#3977=VECTOR('',#14380,10.);
#3978=VECTOR('',#14381,10.);
#3979=VECTOR('',#14384,10.);
#3980=VECTOR('',#14387,10.);
#3981=VECTOR('',#14388,10.);
#3982=VECTOR('',#14389,10.);
#3983=VECTOR('',#14392,10.);
#3984=VECTOR('',#14395,10.);
#3985=VECTOR('',#14398,10.);
#3986=VECTOR('',#14399,10.);
#3987=VECTOR('',#14402,10.);
#3988=VECTOR('',#14403,10.);
#3989=VECTOR('',#14406,10.);
#3990=VECTOR('',#14407,10.);
#3991=VECTOR('',#14410,10.);
#3992=VECTOR('',#14413,10.);
#3993=VECTOR('',#14414,10.);
#3994=VECTOR('',#14415,10.);
#3995=VECTOR('',#14418,10.);
#3996=VECTOR('',#14421,10.);
#3997=VECTOR('',#14422,10.);
#3998=VECTOR('',#14425,10.);
#3999=VECTOR('',#14426,10.);
#4000=VECTOR('',#14429,10.);
#4001=VECTOR('',#14430,10.);
#4002=VECTOR('',#14433,10.);
#4003=VECTOR('',#14434,10.);
#4004=VECTOR('',#14437,10.);
#4005=VECTOR('',#14438,10.);
#4006=VECTOR('',#14441,10.);
#4007=VECTOR('',#14442,10.);
#4008=VECTOR('',#14447,10.);
#4009=VECTOR('',#14450,10.);
#4010=VECTOR('',#14451,10.);
#4011=VECTOR('',#14454,10.);
#4012=VECTOR('',#14455,10.);
#4013=VECTOR('',#14458,10.);
#4014=VECTOR('',#14459,10.);
#4015=VECTOR('',#14462,10.);
#4016=VECTOR('',#14465,10.);
#4017=VECTOR('',#14468,10.);
#4018=VECTOR('',#14469,10.);
#4019=VECTOR('',#14472,10.);
#4020=VECTOR('',#14473,10.);
#4021=VECTOR('',#14476,10.);
#4022=VECTOR('',#14477,10.);
#4023=VECTOR('',#14480,10.);
#4024=VECTOR('',#14481,10.);
#4025=VECTOR('',#14484,10.);
#4026=VECTOR('',#14485,10.);
#4027=VECTOR('',#14488,10.);
#4028=VECTOR('',#14503,9.15);
#4029=VECTOR('',#14516,10.75);
#4030=VECTOR('',#14521,10.75);
#4031=VECTOR('',#14528,3.17500000000003);
#4032=VECTOR('',#14535,2.155);
#4033=VECTOR('',#14540,10.);
#4034=VECTOR('',#14541,10.);
#4035=VECTOR('',#14542,10.);
#4036=VECTOR('',#14543,10.);
#4037=VECTOR('',#14546,10.);
#4038=VECTOR('',#14547,10.);
#4039=VECTOR('',#14548,10.);
#4040=VECTOR('',#14551,10.);
#4041=VECTOR('',#14552,10.);
#4042=VECTOR('',#14553,10.);
#4043=VECTOR('',#14556,10.);
#4044=VECTOR('',#14557,10.);
#4045=VECTOR('',#14560,10.);
#4046=VECTOR('',#14561,10.);
#4047=VECTOR('',#14562,10.);
#4048=VECTOR('',#14563,10.);
#4049=VECTOR('',#14566,10.);
#4050=VECTOR('',#14567,10.);
#4051=VECTOR('',#14568,10.);
#4052=VECTOR('',#14571,10.);
#4053=VECTOR('',#14572,10.);
#4054=VECTOR('',#14573,10.);
#4055=VECTOR('',#14576,10.);
#4056=VECTOR('',#14577,10.);
#4057=VECTOR('',#14582,2.155);
#4058=VECTOR('',#14589,2.155);
#4059=VECTOR('',#14594,10.);
#4060=VECTOR('',#14595,10.);
#4061=VECTOR('',#14596,10.);
#4062=VECTOR('',#14597,10.);
#4063=VECTOR('',#14600,10.);
#4064=VECTOR('',#14601,10.);
#4065=VECTOR('',#14602,10.);
#4066=VECTOR('',#14605,10.);
#4067=VECTOR('',#14606,10.);
#4068=VECTOR('',#14607,10.);
#4069=VECTOR('',#14610,10.);
#4070=VECTOR('',#14611,10.);
#4071=VECTOR('',#14616,11.493);
#4072=VECTOR('',#14623,2.155);
#4073=VECTOR('',#14628,10.);
#4074=VECTOR('',#14629,10.);
#4075=VECTOR('',#14630,10.);
#4076=VECTOR('',#14631,10.);
#4077=VECTOR('',#14634,10.);
#4078=VECTOR('',#14635,10.);
#4079=VECTOR('',#14636,10.);
#4080=VECTOR('',#14639,10.);
#4081=VECTOR('',#14640,10.);
#4082=VECTOR('',#14641,10.);
#4083=VECTOR('',#14644,10.);
#4084=VECTOR('',#14645,10.);
#4085=VECTOR('',#14646,10.);
#4086=VECTOR('',#14649,10.);
#4087=VECTOR('',#14650,10.);
#4088=VECTOR('',#14651,10.);
#4089=VECTOR('',#14654,10.);
#4090=VECTOR('',#14655,10.);
#4091=VECTOR('',#14656,10.);
#4092=VECTOR('',#14659,10.);
#4093=VECTOR('',#14660,10.);
#4094=VECTOR('',#14661,10.);
#4095=VECTOR('',#14664,10.);
#4096=VECTOR('',#14665,10.);
#4097=VECTOR('',#14666,10.);
#4098=VECTOR('',#14669,10.);
#4099=VECTOR('',#14670,10.);
#4100=VECTOR('',#14671,10.);
#4101=VECTOR('',#14678,10.);
#4102=VECTOR('',#14681,10.);
#4103=VECTOR('',#14682,10.);
#4104=VECTOR('',#14683,10.);
#4105=VECTOR('',#14690,10.);
#4106=VECTOR('',#14693,10.);
#4107=VECTOR('',#14694,10.);
#4108=VECTOR('',#14695,10.);
#4109=VECTOR('',#14702,10.);
#4110=VECTOR('',#14705,10.);
#4111=VECTOR('',#14706,10.);
#4112=VECTOR('',#14707,10.);
#4113=VECTOR('',#14722,1.5);
#4114=VECTOR('',#14725,1.5);
#4115=VECTOR('',#14730,6.00000000000002);
#4116=VECTOR('',#14731,6.00000000000002);
#4117=VECTOR('',#14748,10.75);
#4118=VECTOR('',#14753,9.15);
#4119=VECTOR('',#14760,3.17500000000003);
#4120=VECTOR('',#14761,3.17500000000003);
#4121=VECTOR('',#14766,10.75);
#4122=VECTOR('',#14779,10.);
#4123=VECTOR('',#14782,10.);
#4124=VECTOR('',#14785,10.);
#4125=VECTOR('',#14788,10.);
#4126=VECTOR('',#14791,10.);
#4127=VECTOR('',#14792,10.);
#4128=VECTOR('',#14793,10.);
#4129=VECTOR('',#14798,10.);
#4130=VECTOR('',#14801,10.);
#4131=VECTOR('',#14802,10.);
#4132=VECTOR('',#14809,10.);
#4133=VECTOR('',#14810,10.);
#4134=VECTOR('',#14811,10.);
#4135=VECTOR('',#14816,10.);
#4136=VECTOR('',#14819,10.);
#4137=VECTOR('',#14820,10.);
#4138=VECTOR('',#14833,2.5);
#4139=VECTOR('',#14838,10.);
#4140=VECTOR('',#14839,10.);
#4141=VECTOR('',#14840,10.);
#4142=VECTOR('',#14841,10.);
#4143=VECTOR('',#14848,10.);
#4144=VECTOR('',#14851,10.);
#4145=VECTOR('',#14852,10.);
#4146=VECTOR('',#14853,10.);
#4147=VECTOR('',#14864,2.46675107308807);
#4148=VECTOR('',#14871,2.46675107308807);
#4149=VECTOR('',#14878,2.46675107308807);
#4150=VECTOR('',#14885,2.46675107308807);
#4151=VECTOR('',#14892,2.46675107308807);
#4152=VECTOR('',#14897,10.);
#4153=VECTOR('',#14898,10.);
#4154=VECTOR('',#14899,10.);
#4155=VECTOR('',#14900,10.);
#4156=VECTOR('',#14907,10.);
#4157=VECTOR('',#14910,10.);
#4158=VECTOR('',#14911,10.);
#4159=VECTOR('',#14912,10.);
#4160=VECTOR('',#14921,10.);
#4161=VECTOR('',#14922,10.);
#4162=VECTOR('',#14923,10.);
#4163=VECTOR('',#14924,10.);
#4164=VECTOR('',#14931,10.);
#4165=VECTOR('',#14934,10.);
#4166=VECTOR('',#14935,10.);
#4167=VECTOR('',#14936,10.);
#4168=VECTOR('',#14947,2.5);
#4169=VECTOR('',#14954,2.46675107308807);
#4170=VECTOR('',#14961,2.5);
#4171=VECTOR('',#14968,2.46675107308807);
#4172=VECTOR('',#14975,2.46675107308807);
#4173=VECTOR('',#14980,10.);
#4174=VECTOR('',#14981,10.);
#4175=VECTOR('',#14982,10.);
#4176=VECTOR('',#14983,10.);
#4177=VECTOR('',#14990,10.);
#4178=VECTOR('',#14993,10.);
#4179=VECTOR('',#14994,10.);
#4180=VECTOR('',#14995,10.);
#4181=VECTOR('',#15006,2.5);
#4182=VECTOR('',#15013,2.46675107308807);
#4183=VECTOR('',#15018,10.);
#4184=VECTOR('',#15019,10.);
#4185=VECTOR('',#15020,10.);
#4186=VECTOR('',#15021,10.);
#4187=VECTOR('',#15028,10.);
#4188=VECTOR('',#15031,10.);
#4189=VECTOR('',#15032,10.);
#4190=VECTOR('',#15033,10.);
#4191=VECTOR('',#15042,10.);
#4192=VECTOR('',#15043,10.);
#4193=VECTOR('',#15044,10.);
#4194=VECTOR('',#15045,10.);
#4195=VECTOR('',#15052,10.);
#4196=VECTOR('',#15055,10.);
#4197=VECTOR('',#15056,10.);
#4198=VECTOR('',#15057,10.);
#4199=VECTOR('',#15066,10.);
#4200=VECTOR('',#15067,10.);
#4201=VECTOR('',#15068,10.);
#4202=VECTOR('',#15069,10.);
#4203=VECTOR('',#15076,10.);
#4204=VECTOR('',#15079,10.);
#4205=VECTOR('',#15080,10.);
#4206=VECTOR('',#15081,10.);
#4207=VECTOR('',#15090,10.);
#4208=VECTOR('',#15091,10.);
#4209=VECTOR('',#15092,10.);
#4210=VECTOR('',#15093,10.);
#4211=VECTOR('',#15100,10.);
#4212=VECTOR('',#15103,10.);
#4213=VECTOR('',#15104,10.);
#4214=VECTOR('',#15105,10.);
#4215=VECTOR('',#15116,2.46675107308807);
#4216=VECTOR('',#15123,2.46675107308807);
#4217=VECTOR('',#15128,10.);
#4218=VECTOR('',#15129,10.);
#4219=VECTOR('',#15130,10.);
#4220=VECTOR('',#15131,10.);
#4221=VECTOR('',#15138,10.);
#4222=VECTOR('',#15141,10.);
#4223=VECTOR('',#15142,10.);
#4224=VECTOR('',#15143,10.);
#4225=VECTOR('',#15150,10.);
#4226=VECTOR('',#15153,10.);
#4227=VECTOR('',#15154,10.);
#4228=VECTOR('',#15155,10.);
#4229=VECTOR('',#15162,10.);
#4230=VECTOR('',#15165,10.);
#4231=VECTOR('',#15166,10.);
#4232=VECTOR('',#15167,10.);
#4233=VECTOR('',#15184,2.50000000000001);
#4234=VECTOR('',#15191,2.50000000000001);
#4235=VECTOR('',#15198,3.17500000000003);
#4236=VECTOR('',#15205,2.50000000000001);
#4237=VECTOR('',#15212,2.50000000000001);
#4238=VECTOR('',#15219,10.);
#4239=VECTOR('',#15222,10.);
#4240=VECTOR('',#15225,10.);
#4241=VECTOR('',#15226,10.);
#4242=VECTOR('',#15227,10.);
#4243=VECTOR('',#15234,10.);
#4244=VECTOR('',#15237,10.);
#4245=VECTOR('',#15238,10.);
#4246=VECTOR('',#15239,10.);
#4247=VECTOR('',#15246,10.);
#4248=VECTOR('',#15249,10.);
#4249=VECTOR('',#15250,10.);
#4250=VECTOR('',#15251,10.);
#4251=VECTOR('',#15258,10.);
#4252=VECTOR('',#15261,10.);
#4253=VECTOR('',#15262,10.);
#4254=VECTOR('',#15273,2.27961999999998);
#4255=VECTOR('',#15290,2.4505);
#4256=VECTOR('',#15293,9.99999999999999);
#4257=VECTOR('',#15294,10.);
#4258=VECTOR('',#15295,10.);
#4259=VECTOR('',#15298,10.);
#4260=VECTOR('',#15299,10.);
#4261=VECTOR('',#15302,10.);
#4262=VECTOR('',#15303,9.99999999999999);
#4263=VECTOR('',#15306,10.);
#4264=VECTOR('',#15307,10.);
#4265=VECTOR('',#15310,10.);
#4266=VECTOR('',#15311,10.);
#4267=VECTOR('',#15314,10.);
#4268=VECTOR('',#15317,10.);
#4269=VECTOR('',#15318,10.);
#4270=VECTOR('',#15319,10.);
#4271=VECTOR('',#15322,10.);
#4272=VECTOR('',#15323,10.);
#4273=VECTOR('',#15326,10.);
#4274=VECTOR('',#15327,10.);
#4275=VECTOR('',#15330,10.);
#4276=VECTOR('',#15331,10.);
#4277=VECTOR('',#15334,10.);
#4278=VECTOR('',#15335,10.);
#4279=VECTOR('',#15338,10.);
#4280=CIRCLE('',#11441,3.175);
#4281=CIRCLE('',#11442,3.175);
#4282=CIRCLE('',#11443,3.175);
#4283=CIRCLE('',#11445,1.27);
#4284=CIRCLE('',#11447,1.905);
#4285=CIRCLE('',#11450,1.905);
#4286=CIRCLE('',#11453,1.905);
#4287=CIRCLE('',#11456,1.905);
#4288=CIRCLE('',#11477,3.175);
#4289=CIRCLE('',#11478,3.175);
#4290=CIRCLE('',#11479,3.175);
#4291=CIRCLE('',#11481,1.27);
#4292=CIRCLE('',#11483,1.905);
#4293=CIRCLE('',#11486,1.905);
#4294=CIRCLE('',#11489,1.905);
#4295=CIRCLE('',#11492,1.905);
#4296=CIRCLE('',#11513,3.175);
#4297=CIRCLE('',#11514,3.175);
#4298=CIRCLE('',#11515,3.175);
#4299=CIRCLE('',#11517,1.27);
#4300=CIRCLE('',#11519,1.905);
#4301=CIRCLE('',#11522,1.905);
#4302=CIRCLE('',#11525,1.905);
#4303=CIRCLE('',#11528,1.905);
#4304=CIRCLE('',#11549,3.175);
#4305=CIRCLE('',#11550,3.175);
#4306=CIRCLE('',#11551,3.175);
#4307=CIRCLE('',#11553,1.27);
#4308=CIRCLE('',#11555,1.905);
#4309=CIRCLE('',#11558,1.905);
#4310=CIRCLE('',#11561,1.905);
#4311=CIRCLE('',#11564,1.905);
#4312=CIRCLE('',#11585,1.905);
#4313=CIRCLE('',#11605,1.905);
#4314=CIRCLE('',#11625,1.905);
#4315=CIRCLE('',#11645,1.905);
#4316=CIRCLE('',#11664,1.93206329386826);
#4317=CIRCLE('',#11666,1.93206329386826);
#4318=CIRCLE('',#11673,1.93206329386825);
#4319=CIRCLE('',#11675,1.93206329386825);
#4320=CIRCLE('',#11682,1.93206329386826);
#4321=CIRCLE('',#11684,1.93206329386826);
#4322=CIRCLE('',#11691,1.93206329386822);
#4323=CIRCLE('',#11693,1.93206329386822);
#4324=CIRCLE('',#11704,1.905);
#4325=CIRCLE('',#11706,1.905);
#4326=CIRCLE('',#11708,1.905);
#4327=CIRCLE('',#11710,1.905);
#4328=CIRCLE('',#11712,2.62699999999999);
#4329=CIRCLE('',#11713,2.62699999999999);
#4330=CIRCLE('',#11715,3.76999999999999);
#4331=CIRCLE('',#11716,3.76999999999999);
#4332=CIRCLE('',#11718,11.493);
#4333=CIRCLE('',#11719,10.985);
#4334=CIRCLE('',#11721,10.985);
#4335=CIRCLE('',#11723,1.58024047358085);
#4336=CIRCLE('',#11724,2.155);
#4337=CIRCLE('',#11726,1.58024047358083);
#4338=CIRCLE('',#11727,2.155);
#4339=CIRCLE('',#11729,1.58024047358085);
#4340=CIRCLE('',#11730,2.155);
#4341=CIRCLE('',#11732,1.58024047358083);
#4342=CIRCLE('',#11733,2.155);
#4343=CIRCLE('',#11734,1.86136507718219);
#4344=CIRCLE('',#11735,1.90494743284919);
#4345=CIRCLE('',#11738,1.86136507718315);
#4346=CIRCLE('',#11739,1.9049474328492);
#4347=CIRCLE('',#11740,1.86136507718391);
#4348=CIRCLE('',#11741,1.90494743284917);
#4349=CIRCLE('',#11742,1.86136507718316);
#4350=CIRCLE('',#11743,1.90494743284856);
#4351=CIRCLE('',#11775,2.5);
#4352=CIRCLE('',#11776,1.99200000000004);
#4353=CIRCLE('',#11778,1.99200000000004);
#4354=CIRCLE('',#11779,2.5);
#4355=CIRCLE('',#11781,0.975999999999995);
#4356=CIRCLE('',#11783,2.5);
#4357=CIRCLE('',#11784,2.5);
#4358=CIRCLE('',#11790,5.16699999999999);
#4359=CIRCLE('',#11791,5.16699999999999);
#4360=CIRCLE('',#11793,3.175);
#4361=CIRCLE('',#11794,3.429);
#4362=CIRCLE('',#11796,3.175);
#4363=CIRCLE('',#11797,3.429);
#4364=CIRCLE('',#11799,3.175);
#4365=CIRCLE('',#11800,3.429);
#4366=CIRCLE('',#11802,3.175);
#4367=CIRCLE('',#11803,3.429);
#4368=CIRCLE('',#11805,3.175);
#4369=CIRCLE('',#11807,3.175);
#4370=CIRCLE('',#11809,3.175);
#4371=CIRCLE('',#11811,3.175);
#4372=CIRCLE('',#11813,2.62699999999999);
#4373=CIRCLE('',#11814,2.62699999999999);
#4374=CIRCLE('',#11849,0.761999999999999);
#4375=CIRCLE('',#11852,0.761999999999999);
#4376=CIRCLE('',#11859,2.62699999999999);
#4377=CIRCLE('',#11860,2.62699999999999);
#4378=CIRCLE('',#11862,1.905);
#4379=CIRCLE('',#11863,1.905);
#4380=CIRCLE('',#11865,1.905);
#4381=CIRCLE('',#11866,1.905);
#4382=CIRCLE('',#11868,1.905);
#4383=CIRCLE('',#11869,1.905);
#4384=CIRCLE('',#11871,1.905);
#4385=CIRCLE('',#11872,1.905);
#4386=CIRCLE('',#11890,11.9505);
#4387=CIRCLE('',#11891,9.95049999999999);
#4388=CIRCLE('',#11893,11.9505);
#4389=CIRCLE('',#11895,8.00000000000001);
#4390=CIRCLE('',#11897,9.95049999999999);
#4391=CIRCLE('',#11899,8.00000000000001);
#4392=CIRCLE('',#11903,2.5);
#4393=CIRCLE('',#11904,2.5);
#4394=CIRCLE('',#11906,4.49999999999999);
#4395=CIRCLE('',#11907,4.49999999999999);
#4396=CIRCLE('',#11912,2.117);
#4397=CIRCLE('',#11913,2.5);
#4398=CIRCLE('',#11915,2.117);
#4399=CIRCLE('',#11916,2.5);
#4400=CIRCLE('',#11920,3.92);
#4401=CIRCLE('',#11926,3.92);
#4402=CIRCLE('',#11932,5.73351648351648);
#4403=CIRCLE('',#11933,5.73351648351648);
#4404=CIRCLE('',#11935,5.73351648351648);
#4405=CIRCLE('',#11936,1.21175743903915);
#4406=CIRCLE('',#11938,5.73351648351648);
#4407=CIRCLE('',#11940,8.);
#4408=CIRCLE('',#11941,7.75);
#4409=CIRCLE('',#11943,8.);
#4410=CIRCLE('',#11944,8.);
#4411=CIRCLE('',#11946,7.75);
#4412=CIRCLE('',#11950,4.76648351648352);
#4413=CIRCLE('',#11951,4.76648351648352);
#4414=CIRCLE('',#11953,1.21175743903915);
#4415=CIRCLE('',#11954,4.03824256096085);
#4416=CIRCLE('',#11956,3.26912128048043);
#4417=CIRCLE('',#11957,3.26912128048043);
#4418=CIRCLE('',#11959,4.01780239848197);
#4419=CIRCLE('',#11963,2.5);
#4420=CIRCLE('',#11964,3.26912128048043);
#4421=CIRCLE('',#11966,2.5);
#4422=CIRCLE('',#11967,2.5);
#4423=CIRCLE('',#11969,2.75);
#4424=CIRCLE('',#11971,4.76648351648352);
#4425=CIRCLE('',#11972,4.76648351648352);
#4426=CIRCLE('',#11974,4.03824256096085);
#4427=CIRCLE('',#11975,1.21175743903915);
#4428=CIRCLE('',#11977,3.26912128048043);
#4429=CIRCLE('',#11978,3.26912128048043);
#4430=CIRCLE('',#11980,4.01780239848197);
#4431=CIRCLE('',#11985,1.21175743903915);
#4432=CIRCLE('',#11987,1.21175743903915);
#4433=CIRCLE('',#11989,1.21175743903915);
#4434=CIRCLE('',#11991,1.21175743903915);
#4435=CIRCLE('',#11993,1.21175743903915);
#4436=CIRCLE('',#11995,1.21175743903915);
#4437=CIRCLE('',#11997,1.21175743903915);
#4438=CIRCLE('',#11999,1.21175743903915);
#4439=CIRCLE('',#12001,1.21175743903915);
#4440=CIRCLE('',#12003,1.21175743903915);
#4441=CIRCLE('',#12016,2.1);
#4442=CIRCLE('',#12017,2.1);
#4443=CIRCLE('',#12028,0.500000000000003);
#4444=CIRCLE('',#12029,0.500000000000003);
#4445=CIRCLE('',#12049,0.500000000000003);
#4446=CIRCLE('',#12050,0.500000000000003);
#4447=CIRCLE('',#12064,0.500000000000003);
#4448=CIRCLE('',#12065,0.500000000000003);
#4449=CIRCLE('',#12066,2.1);
#4450=CIRCLE('',#12073,2.1);
#4451=CIRCLE('',#12084,0.500000000000003);
#4452=CIRCLE('',#12105,0.500000000000003);
#4453=CIRCLE('',#12120,10.75);
#4454=CIRCLE('',#12121,3.17500000000003);
#4455=CIRCLE('',#12123,9.15);
#4456=CIRCLE('',#12124,9.15);
#4457=CIRCLE('',#12126,10.75);
#4458=CIRCLE('',#12128,10.75);
#4459=CIRCLE('',#12130,10.75);
#4460=CIRCLE('',#12133,3.17500000000003);
#4461=CIRCLE('',#12137,2.155);
#4462=CIRCLE('',#12138,2.155);
#4463=CIRCLE('',#12148,2.155);
#4464=CIRCLE('',#12149,2.155);
#4465=CIRCLE('',#12151,2.155);
#4466=CIRCLE('',#12152,2.155);
#4467=CIRCLE('',#12158,11.493);
#4468=CIRCLE('',#12159,11.493);
#4469=CIRCLE('',#12161,2.155);
#4470=CIRCLE('',#12162,2.155);
#4471=CIRCLE('',#12173,5.);
#4472=CIRCLE('',#12174,5.);
#4473=CIRCLE('',#12177,5.00000000000002);
#4474=CIRCLE('',#12178,5.00000000000002);
#4475=CIRCLE('',#12181,5.);
#4476=CIRCLE('',#12182,5.);
#4477=CIRCLE('',#12185,4.99999999999999);
#4478=CIRCLE('',#12186,4.99999999999999);
#4479=CIRCLE('',#12193,6.00000000000002);
#4480=CIRCLE('',#12194,6.00000000000002);
#4481=CIRCLE('',#12196,3.17500000000003);
#4482=CIRCLE('',#12198,10.75);
#4483=CIRCLE('',#12199,9.15);
#4484=CIRCLE('',#12201,10.75);
#4485=CIRCLE('',#12204,9.15);
#4486=CIRCLE('',#12206,3.17500000000003);
#4487=CIRCLE('',#12208,10.75);
#4488=CIRCLE('',#12209,10.75);
#4489=CIRCLE('',#12214,11.5);
#4490=CIRCLE('',#12215,11.5);
#4491=CIRCLE('',#12216,9.5);
#4492=CIRCLE('',#12217,9.5);
#4493=CIRCLE('',#12220,9.5);
#4494=CIRCLE('',#12223,9.5);
#4495=CIRCLE('',#12226,11.5);
#4496=CIRCLE('',#12229,11.5);
#4497=CIRCLE('',#12233,2.5);
#4498=CIRCLE('',#12234,2.5);
#4499=CIRCLE('',#12237,1.3925055570925);
#4500=CIRCLE('',#12238,1.3925055570925);
#4501=CIRCLE('',#12241,1.3925055570925);
#4502=CIRCLE('',#12242,1.3925055570925);
#4503=CIRCLE('',#12244,2.46675107308807);
#4504=CIRCLE('',#12245,2.46675107308807);
#4505=CIRCLE('',#12247,2.46675107308807);
#4506=CIRCLE('',#12248,2.46675107308807);
#4507=CIRCLE('',#12250,2.46675107308807);
#4508=CIRCLE('',#12251,2.46675107308807);
#4509=CIRCLE('',#12253,2.46675107308807);
#4510=CIRCLE('',#12254,2.46675107308807);
#4511=CIRCLE('',#12256,2.46675107308807);
#4512=CIRCLE('',#12257,2.46675107308807);
#4513=CIRCLE('',#12260,2.69990459756453);
#4514=CIRCLE('',#12261,2.69990459756453);
#4515=CIRCLE('',#12264,2.69990459756453);
#4516=CIRCLE('',#12265,2.69990459756453);
#4517=CIRCLE('',#12268,1.3925055570925);
#4518=CIRCLE('',#12269,1.3925055570925);
#4519=CIRCLE('',#12272,1.3925055570925);
#4520=CIRCLE('',#12273,1.3925055570925);
#4521=CIRCLE('',#12275,2.5);
#4522=CIRCLE('',#12276,2.5);
#4523=CIRCLE('',#12278,2.46675107308807);
#4524=CIRCLE('',#12279,2.46675107308807);
#4525=CIRCLE('',#12281,2.5);
#4526=CIRCLE('',#12282,2.5);
#4527=CIRCLE('',#12284,2.46675107308807);
#4528=CIRCLE('',#12285,2.46675107308807);
#4529=CIRCLE('',#12287,2.46675107308807);
#4530=CIRCLE('',#12288,2.46675107308807);
#4531=CIRCLE('',#12291,1.3925055570925);
#4532=CIRCLE('',#12292,1.3925055570925);
#4533=CIRCLE('',#12295,1.3925055570925);
#4534=CIRCLE('',#12296,1.3925055570925);
#4535=CIRCLE('',#12298,2.5);
#4536=CIRCLE('',#12299,2.5);
#4537=CIRCLE('',#12301,2.46675107308807);
#4538=CIRCLE('',#12302,2.46675107308807);
#4539=CIRCLE('',#12305,1.3925055570925);
#4540=CIRCLE('',#12306,1.3925055570925);
#4541=CIRCLE('',#12309,1.3925055570925);
#4542=CIRCLE('',#12310,1.3925055570925);
#4543=CIRCLE('',#12313,1.3925055570925);
#4544=CIRCLE('',#12314,1.3925055570925);
#4545=CIRCLE('',#12317,1.3925055570925);
#4546=CIRCLE('',#12318,1.3925055570925);
#4547=CIRCLE('',#12321,1.3925055570925);
#4548=CIRCLE('',#12322,1.3925055570925);
#4549=CIRCLE('',#12325,1.3925055570925);
#4550=CIRCLE('',#12326,1.3925055570925);
#4551=CIRCLE('',#12329,2.69990459756453);
#4552=CIRCLE('',#12330,2.69990459756453);
#4553=CIRCLE('',#12333,2.69990459756453);
#4554=CIRCLE('',#12334,2.69990459756453);
#4555=CIRCLE('',#12336,2.46675107308807);
#4556=CIRCLE('',#12337,2.46675107308807);
#4557=CIRCLE('',#12339,2.46675107308807);
#4558=CIRCLE('',#12340,2.46675107308807);
#4559=CIRCLE('',#12343,3.00000000000004);
#4560=CIRCLE('',#12344,3.00000000000004);
#4561=CIRCLE('',#12347,3.00000000000003);
#4562=CIRCLE('',#12348,3.00000000000003);
#4563=CIRCLE('',#12351,3.00000000000004);
#4564=CIRCLE('',#12352,3.00000000000004);
#4565=CIRCLE('',#12355,3.00000000000004);
#4566=CIRCLE('',#12356,3.00000000000004);
#4567=CIRCLE('',#12361,2.50000000000001);
#4568=CIRCLE('',#12362,2.50000000000001);
#4569=CIRCLE('',#12364,2.50000000000001);
#4570=CIRCLE('',#12365,2.50000000000001);
#4571=CIRCLE('',#12367,3.17500000000003);
#4572=CIRCLE('',#12368,3.17500000000003);
#4573=CIRCLE('',#12370,2.50000000000001);
#4574=CIRCLE('',#12371,2.50000000000001);
#4575=CIRCLE('',#12373,2.50000000000001);
#4576=CIRCLE('',#12374,2.50000000000001);
#4577=CIRCLE('',#12376,4.99999999999993);
#4578=CIRCLE('',#12377,4.99999999999993);
#4579=CIRCLE('',#12380,4.99999999999993);
#4580=CIRCLE('',#12381,4.99999999999993);
#4581=CIRCLE('',#12384,5.);
#4582=CIRCLE('',#12385,5.);
#4583=CIRCLE('',#12388,5.);
#4584=CIRCLE('',#12389,5.);
#4585=CIRCLE('',#12395,2.4505);
#4586=CIRCLE('',#12396,2.00924000000001);
#4587=CIRCLE('',#12398,2.4505);
#4588=CIRCLE('',#12399,0.2);
#4589=CIRCLE('',#12400,2.6505);
#4590=CIRCLE('',#12402,4.75);
#4591=CIRCLE('',#12418,1.95);
#4592=CIRCLE('',#12420,5.16792277674902);
#4593=VERTEX_POINT('',#15384);
#4594=VERTEX_POINT('',#15386);
#4595=VERTEX_POINT('',#15388);
#4596=VERTEX_POINT('',#15392);
#4597=VERTEX_POINT('',#15393);
#4598=VERTEX_POINT('',#15399);
#4599=VERTEX_POINT('',#15404);
#4600=VERTEX_POINT('',#15406);
#4601=VERTEX_POINT('',#15408);
#4602=VERTEX_POINT('',#15410);
#4603=VERTEX_POINT('',#15417);
#4604=VERTEX_POINT('',#15419);
#4605=VERTEX_POINT('',#15421);
#4606=VERTEX_POINT('',#15423);
#4607=VERTEX_POINT('',#15430);
#4608=VERTEX_POINT('',#15432);
#4609=VERTEX_POINT('',#15434);
#4610=VERTEX_POINT('',#15436);
#4611=VERTEX_POINT('',#15443);
#4612=VERTEX_POINT('',#15445);
#4613=VERTEX_POINT('',#15449);
#4614=VERTEX_POINT('',#15453);
#4615=VERTEX_POINT('',#15457);
#4616=VERTEX_POINT('',#15462);
#4617=VERTEX_POINT('',#15466);
#4618=VERTEX_POINT('',#15468);
#4619=VERTEX_POINT('',#15472);
#4620=VERTEX_POINT('',#15474);
#4621=VERTEX_POINT('',#15478);
#4622=VERTEX_POINT('',#15480);
#4623=VERTEX_POINT('',#15486);
#4624=VERTEX_POINT('',#15488);
#4625=VERTEX_POINT('',#15494);
#4626=VERTEX_POINT('',#15496);
#4627=VERTEX_POINT('',#15499);
#4628=VERTEX_POINT('',#15501);
#4629=VERTEX_POINT('',#15515);
#4630=VERTEX_POINT('',#15517);
#4631=VERTEX_POINT('',#15519);
#4632=VERTEX_POINT('',#15523);
#4633=VERTEX_POINT('',#15524);
#4634=VERTEX_POINT('',#15530);
#4635=VERTEX_POINT('',#15535);
#4636=VERTEX_POINT('',#15537);
#4637=VERTEX_POINT('',#15539);
#4638=VERTEX_POINT('',#15541);
#4639=VERTEX_POINT('',#15548);
#4640=VERTEX_POINT('',#15550);
#4641=VERTEX_POINT('',#15552);
#4642=VERTEX_POINT('',#15554);
#4643=VERTEX_POINT('',#15561);
#4644=VERTEX_POINT('',#15563);
#4645=VERTEX_POINT('',#15565);
#4646=VERTEX_POINT('',#15567);
#4647=VERTEX_POINT('',#15574);
#4648=VERTEX_POINT('',#15576);
#4649=VERTEX_POINT('',#15580);
#4650=VERTEX_POINT('',#15584);
#4651=VERTEX_POINT('',#15588);
#4652=VERTEX_POINT('',#15593);
#4653=VERTEX_POINT('',#15597);
#4654=VERTEX_POINT('',#15599);
#4655=VERTEX_POINT('',#15603);
#4656=VERTEX_POINT('',#15605);
#4657=VERTEX_POINT('',#15609);
#4658=VERTEX_POINT('',#15611);
#4659=VERTEX_POINT('',#15617);
#4660=VERTEX_POINT('',#15619);
#4661=VERTEX_POINT('',#15625);
#4662=VERTEX_POINT('',#15627);
#4663=VERTEX_POINT('',#15630);
#4664=VERTEX_POINT('',#15632);
#4665=VERTEX_POINT('',#15646);
#4666=VERTEX_POINT('',#15648);
#4667=VERTEX_POINT('',#15650);
#4668=VERTEX_POINT('',#15654);
#4669=VERTEX_POINT('',#15655);
#4670=VERTEX_POINT('',#15661);
#4671=VERTEX_POINT('',#15666);
#4672=VERTEX_POINT('',#15668);
#4673=VERTEX_POINT('',#15670);
#4674=VERTEX_POINT('',#15672);
#4675=VERTEX_POINT('',#15679);
#4676=VERTEX_POINT('',#15681);
#4677=VERTEX_POINT('',#15683);
#4678=VERTEX_POINT('',#15685);
#4679=VERTEX_POINT('',#15692);
#4680=VERTEX_POINT('',#15694);
#4681=VERTEX_POINT('',#15696);
#4682=VERTEX_POINT('',#15698);
#4683=VERTEX_POINT('',#15705);
#4684=VERTEX_POINT('',#15707);
#4685=VERTEX_POINT('',#15711);
#4686=VERTEX_POINT('',#15715);
#4687=VERTEX_POINT('',#15719);
#4688=VERTEX_POINT('',#15724);
#4689=VERTEX_POINT('',#15728);
#4690=VERTEX_POINT('',#15730);
#4691=VERTEX_POINT('',#15734);
#4692=VERTEX_POINT('',#15736);
#4693=VERTEX_POINT('',#15740);
#4694=VERTEX_POINT('',#15742);
#4695=VERTEX_POINT('',#15748);
#4696=VERTEX_POINT('',#15750);
#4697=VERTEX_POINT('',#15756);
#4698=VERTEX_POINT('',#15758);
#4699=VERTEX_POINT('',#15761);
#4700=VERTEX_POINT('',#15763);
#4701=VERTEX_POINT('',#15777);
#4702=VERTEX_POINT('',#15779);
#4703=VERTEX_POINT('',#15781);
#4704=VERTEX_POINT('',#15785);
#4705=VERTEX_POINT('',#15786);
#4706=VERTEX_POINT('',#15792);
#4707=VERTEX_POINT('',#15797);
#4708=VERTEX_POINT('',#15799);
#4709=VERTEX_POINT('',#15801);
#4710=VERTEX_POINT('',#15803);
#4711=VERTEX_POINT('',#15810);
#4712=VERTEX_POINT('',#15812);
#4713=VERTEX_POINT('',#15814);
#4714=VERTEX_POINT('',#15816);
#4715=VERTEX_POINT('',#15823);
#4716=VERTEX_POINT('',#15825);
#4717=VERTEX_POINT('',#15827);
#4718=VERTEX_POINT('',#15829);
#4719=VERTEX_POINT('',#15836);
#4720=VERTEX_POINT('',#15838);
#4721=VERTEX_POINT('',#15842);
#4722=VERTEX_POINT('',#15846);
#4723=VERTEX_POINT('',#15850);
#4724=VERTEX_POINT('',#15855);
#4725=VERTEX_POINT('',#15859);
#4726=VERTEX_POINT('',#15861);
#4727=VERTEX_POINT('',#15865);
#4728=VERTEX_POINT('',#15867);
#4729=VERTEX_POINT('',#15871);
#4730=VERTEX_POINT('',#15873);
#4731=VERTEX_POINT('',#15879);
#4732=VERTEX_POINT('',#15881);
#4733=VERTEX_POINT('',#15887);
#4734=VERTEX_POINT('',#15889);
#4735=VERTEX_POINT('',#15892);
#4736=VERTEX_POINT('',#15894);
#4737=VERTEX_POINT('',#15908);
#4738=VERTEX_POINT('',#15909);
#4739=VERTEX_POINT('',#15911);
#4740=VERTEX_POINT('',#15936);
#4741=VERTEX_POINT('',#15959);
#4742=VERTEX_POINT('',#15960);
#4743=VERTEX_POINT('',#16037);
#4744=VERTEX_POINT('',#16038);
#4745=VERTEX_POINT('',#16113);
#4746=VERTEX_POINT('',#16114);
#4747=VERTEX_POINT('',#16189);
#4748=VERTEX_POINT('',#16190);
#4749=VERTEX_POINT('',#16265);
#4750=VERTEX_POINT('',#16266);
#4751=VERTEX_POINT('',#16341);
#4752=VERTEX_POINT('',#16342);
#4753=VERTEX_POINT('',#16419);
#4754=VERTEX_POINT('',#16420);
#4755=VERTEX_POINT('',#16497);
#4756=VERTEX_POINT('',#16498);
#4757=VERTEX_POINT('',#16573);
#4758=VERTEX_POINT('',#16574);
#4759=VERTEX_POINT('',#16649);
#4760=VERTEX_POINT('',#16650);
#4761=VERTEX_POINT('',#16725);
#4762=VERTEX_POINT('',#16726);
#4763=VERTEX_POINT('',#16801);
#4764=VERTEX_POINT('',#16802);
#4765=VERTEX_POINT('',#16877);
#4766=VERTEX_POINT('',#16878);
#4767=VERTEX_POINT('',#16955);
#4768=VERTEX_POINT('',#16956);
#4769=VERTEX_POINT('',#17033);
#4770=VERTEX_POINT('',#17034);
#4771=VERTEX_POINT('',#17109);
#4772=VERTEX_POINT('',#17110);
#4773=VERTEX_POINT('',#17185);
#4774=VERTEX_POINT('',#17186);
#4775=VERTEX_POINT('',#17261);
#4776=VERTEX_POINT('',#17262);
#4777=VERTEX_POINT('',#17337);
#4778=VERTEX_POINT('',#17338);
#4779=VERTEX_POINT('',#17340);
#4780=VERTEX_POINT('',#17357);
#4781=VERTEX_POINT('',#17372);
#4782=VERTEX_POINT('',#17373);
#4783=VERTEX_POINT('',#17450);
#4784=VERTEX_POINT('',#17451);
#4785=VERTEX_POINT('',#17526);
#4786=VERTEX_POINT('',#17527);
#4787=VERTEX_POINT('',#17602);
#4788=VERTEX_POINT('',#17603);
#4789=VERTEX_POINT('',#17678);
#4790=VERTEX_POINT('',#17679);
#4791=VERTEX_POINT('',#17754);
#4792=VERTEX_POINT('',#17755);
#4793=VERTEX_POINT('',#17830);
#4794=VERTEX_POINT('',#17831);
#4795=VERTEX_POINT('',#17910);
#4796=VERTEX_POINT('',#17911);
#4797=VERTEX_POINT('',#17986);
#4798=VERTEX_POINT('',#17987);
#4799=VERTEX_POINT('',#18062);
#4800=VERTEX_POINT('',#18063);
#4801=VERTEX_POINT('',#18138);
#4802=VERTEX_POINT('',#18139);
#4803=VERTEX_POINT('',#18214);
#4804=VERTEX_POINT('',#18215);
#4805=VERTEX_POINT('',#18290);
#4806=VERTEX_POINT('',#18291);
#4807=VERTEX_POINT('',#18368);
#4808=VERTEX_POINT('',#18369);
#4809=VERTEX_POINT('',#18446);
#4810=VERTEX_POINT('',#18447);
#4811=VERTEX_POINT('',#18522);
#4812=VERTEX_POINT('',#18523);
#4813=VERTEX_POINT('',#18598);
#4814=VERTEX_POINT('',#18599);
#4815=VERTEX_POINT('',#18674);
#4816=VERTEX_POINT('',#18675);
#4817=VERTEX_POINT('',#18750);
#4818=VERTEX_POINT('',#18751);
#4819=VERTEX_POINT('',#18753);
#4820=VERTEX_POINT('',#18764);
#4821=VERTEX_POINT('',#18765);
#4822=VERTEX_POINT('',#18842);
#4823=VERTEX_POINT('',#18843);
#4824=VERTEX_POINT('',#18918);
#4825=VERTEX_POINT('',#18919);
#4826=VERTEX_POINT('',#18994);
#4827=VERTEX_POINT('',#18995);
#4828=VERTEX_POINT('',#19070);
#4829=VERTEX_POINT('',#19071);
#4830=VERTEX_POINT('',#19146);
#4831=VERTEX_POINT('',#19147);
#4832=VERTEX_POINT('',#19222);
#4833=VERTEX_POINT('',#19223);
#4834=VERTEX_POINT('',#19300);
#4835=VERTEX_POINT('',#19301);
#4836=VERTEX_POINT('',#19378);
#4837=VERTEX_POINT('',#19379);
#4838=VERTEX_POINT('',#19454);
#4839=VERTEX_POINT('',#19455);
#4840=VERTEX_POINT('',#19530);
#4841=VERTEX_POINT('',#19531);
#4842=VERTEX_POINT('',#19606);
#4843=VERTEX_POINT('',#19607);
#4844=VERTEX_POINT('',#19682);
#4845=VERTEX_POINT('',#19683);
#4846=VERTEX_POINT('',#19760);
#4847=VERTEX_POINT('',#19761);
#4848=VERTEX_POINT('',#19838);
#4849=VERTEX_POINT('',#19839);
#4850=VERTEX_POINT('',#19914);
#4851=VERTEX_POINT('',#19915);
#4852=VERTEX_POINT('',#19990);
#4853=VERTEX_POINT('',#19991);
#4854=VERTEX_POINT('',#20066);
#4855=VERTEX_POINT('',#20067);
#4856=VERTEX_POINT('',#20142);
#4857=VERTEX_POINT('',#20143);
#4858=VERTEX_POINT('',#20145);
#4859=VERTEX_POINT('',#20180);
#4860=VERTEX_POINT('',#20213);
#4861=VERTEX_POINT('',#20214);
#4862=VERTEX_POINT('',#20289);
#4863=VERTEX_POINT('',#20290);
#4864=VERTEX_POINT('',#20365);
#4865=VERTEX_POINT('',#20366);
#4866=VERTEX_POINT('',#20441);
#4867=VERTEX_POINT('',#20442);
#4868=VERTEX_POINT('',#20517);
#4869=VERTEX_POINT('',#20518);
#4870=VERTEX_POINT('',#20593);
#4871=VERTEX_POINT('',#20594);
#4872=VERTEX_POINT('',#20671);
#4873=VERTEX_POINT('',#20672);
#4874=VERTEX_POINT('',#20749);
#4875=VERTEX_POINT('',#20750);
#4876=VERTEX_POINT('',#20825);
#4877=VERTEX_POINT('',#20826);
#4878=VERTEX_POINT('',#20901);
#4879=VERTEX_POINT('',#20902);
#4880=VERTEX_POINT('',#20977);
#4881=VERTEX_POINT('',#20978);
#4882=VERTEX_POINT('',#21053);
#4883=VERTEX_POINT('',#21054);
#4884=VERTEX_POINT('',#21129);
#4885=VERTEX_POINT('',#21130);
#4886=VERTEX_POINT('',#21209);
#4887=VERTEX_POINT('',#21210);
#4888=VERTEX_POINT('',#21285);
#4889=VERTEX_POINT('',#21286);
#4890=VERTEX_POINT('',#21361);
#4891=VERTEX_POINT('',#21362);
#4892=VERTEX_POINT('',#21437);
#4893=VERTEX_POINT('',#21438);
#4894=VERTEX_POINT('',#21513);
#4895=VERTEX_POINT('',#21514);
#4896=VERTEX_POINT('',#21516);
#4897=VERTEX_POINT('',#21533);
#4898=VERTEX_POINT('',#21534);
#4899=VERTEX_POINT('',#21536);
#4900=VERTEX_POINT('',#21593);
#4901=VERTEX_POINT('',#21594);
#4902=VERTEX_POINT('',#21669);
#4903=VERTEX_POINT('',#21670);
#4904=VERTEX_POINT('',#21745);
#4905=VERTEX_POINT('',#21746);
#4906=VERTEX_POINT('',#21821);
#4907=VERTEX_POINT('',#21822);
#4908=VERTEX_POINT('',#21899);
#4909=VERTEX_POINT('',#21900);
#4910=VERTEX_POINT('',#21902);
#4911=VERTEX_POINT('',#21937);
#4912=VERTEX_POINT('',#21972);
#4913=VERTEX_POINT('',#21973);
#4914=VERTEX_POINT('',#21975);
#4915=VERTEX_POINT('',#21992);
#4916=VERTEX_POINT('',#21993);
#4917=VERTEX_POINT('',#21995);
#4918=VERTEX_POINT('',#22052);
#4919=VERTEX_POINT('',#22053);
#4920=VERTEX_POINT('',#22128);
#4921=VERTEX_POINT('',#22129);
#4922=VERTEX_POINT('',#22204);
#4923=VERTEX_POINT('',#22205);
#4924=VERTEX_POINT('',#22280);
#4925=VERTEX_POINT('',#22281);
#4926=VERTEX_POINT('',#22358);
#4927=VERTEX_POINT('',#22359);
#4928=VERTEX_POINT('',#22361);
#4929=VERTEX_POINT('',#22396);
#4930=VERTEX_POINT('',#22431);
#4931=VERTEX_POINT('',#22432);
#4932=VERTEX_POINT('',#22434);
#4933=VERTEX_POINT('',#22451);
#4934=VERTEX_POINT('',#22452);
#4935=VERTEX_POINT('',#22454);
#4936=VERTEX_POINT('',#22511);
#4937=VERTEX_POINT('',#22512);
#4938=VERTEX_POINT('',#22587);
#4939=VERTEX_POINT('',#22588);
#4940=VERTEX_POINT('',#22663);
#4941=VERTEX_POINT('',#22664);
#4942=VERTEX_POINT('',#22739);
#4943=VERTEX_POINT('',#22740);
#4944=VERTEX_POINT('',#22817);
#4945=VERTEX_POINT('',#22818);
#4946=VERTEX_POINT('',#22820);
#4947=VERTEX_POINT('',#22855);
#4948=VERTEX_POINT('',#22890);
#4949=VERTEX_POINT('',#22891);
#4950=VERTEX_POINT('',#22893);
#4951=VERTEX_POINT('',#22910);
#4952=VERTEX_POINT('',#22911);
#4953=VERTEX_POINT('',#22913);
#4954=VERTEX_POINT('',#22970);
#4955=VERTEX_POINT('',#22971);
#4956=VERTEX_POINT('',#23046);
#4957=VERTEX_POINT('',#23047);
#4958=VERTEX_POINT('',#23122);
#4959=VERTEX_POINT('',#23123);
#4960=VERTEX_POINT('',#23198);
#4961=VERTEX_POINT('',#23199);
#4962=VERTEX_POINT('',#23276);
#4963=VERTEX_POINT('',#23277);
#4964=VERTEX_POINT('',#23279);
#4965=VERTEX_POINT('',#23314);
#4966=VERTEX_POINT('',#23641);
#4967=VERTEX_POINT('',#23678);
#4968=VERTEX_POINT('',#23713);
#4969=VERTEX_POINT('',#23742);
#4970=VERTEX_POINT('',#23769);
#4971=VERTEX_POINT('',#23790);
#4972=VERTEX_POINT('',#23809);
#4973=VERTEX_POINT('',#23822);
#4974=VERTEX_POINT('',#23833);
#4975=VERTEX_POINT('',#23835);
#4976=VERTEX_POINT('',#23839);
#4977=VERTEX_POINT('',#23841);
#4978=VERTEX_POINT('',#23845);
#4979=VERTEX_POINT('',#23847);
#4980=VERTEX_POINT('',#23851);
#4981=VERTEX_POINT('',#23855);
#4982=VERTEX_POINT('',#23884);
#4983=VERTEX_POINT('',#23897);
#4984=VERTEX_POINT('',#23913);
#4985=VERTEX_POINT('',#23917);
#4986=VERTEX_POINT('',#23946);
#4987=VERTEX_POINT('',#23959);
#4988=VERTEX_POINT('',#23975);
#4989=VERTEX_POINT('',#23979);
#4990=VERTEX_POINT('',#24008);
#4991=VERTEX_POINT('',#24021);
#4992=VERTEX_POINT('',#24037);
#4993=VERTEX_POINT('',#24041);
#4994=VERTEX_POINT('',#24070);
#4995=VERTEX_POINT('',#24083);
#4996=VERTEX_POINT('',#24099);
#4997=VERTEX_POINT('',#24741);
#4998=VERTEX_POINT('',#25683);
#4999=VERTEX_POINT('',#26631);
#5000=VERTEX_POINT('',#26632);
#5001=VERTEX_POINT('',#26634);
#5002=VERTEX_POINT('',#26636);
#5003=VERTEX_POINT('',#26638);
#5004=VERTEX_POINT('',#26640);
#5005=VERTEX_POINT('',#26642);
#5006=VERTEX_POINT('',#26644);
#5007=VERTEX_POINT('',#27291);
#5008=VERTEX_POINT('',#28232);
#5009=VERTEX_POINT('',#29817);
#5010=VERTEX_POINT('',#30758);
#5011=VERTEX_POINT('',#32343);
#5012=VERTEX_POINT('',#33284);
#5013=VERTEX_POINT('',#34234);
#5014=VERTEX_POINT('',#34236);
#5015=VERTEX_POINT('',#34240);
#5016=VERTEX_POINT('',#34244);
#5017=VERTEX_POINT('',#34246);
#5018=VERTEX_POINT('',#34250);
#5019=VERTEX_POINT('',#34254);
#5020=VERTEX_POINT('',#34258);
#5021=VERTEX_POINT('',#34262);
#5022=VERTEX_POINT('',#34266);
#5023=VERTEX_POINT('',#34270);
#5024=VERTEX_POINT('',#34274);
#5025=VERTEX_POINT('',#34278);
#5026=VERTEX_POINT('',#34282);
#5027=VERTEX_POINT('',#34288);
#5028=VERTEX_POINT('',#34292);
#5029=VERTEX_POINT('',#34299);
#5030=VERTEX_POINT('',#34300);
#5031=VERTEX_POINT('',#34302);
#5032=VERTEX_POINT('',#34304);
#5033=VERTEX_POINT('',#34311);
#5034=VERTEX_POINT('',#34317);
#5035=VERTEX_POINT('',#34318);
#5036=VERTEX_POINT('',#34322);
#5037=VERTEX_POINT('',#34325);
#5038=VERTEX_POINT('',#34327);
#5039=VERTEX_POINT('',#34336);
#5040=VERTEX_POINT('',#34338);
#5041=VERTEX_POINT('',#34342);
#5042=VERTEX_POINT('',#34344);
#5043=VERTEX_POINT('',#34348);
#5044=VERTEX_POINT('',#34350);
#5045=VERTEX_POINT('',#34354);
#5046=VERTEX_POINT('',#34356);
#5047=VERTEX_POINT('',#34360);
#5048=VERTEX_POINT('',#34362);
#5049=VERTEX_POINT('',#34366);
#5050=VERTEX_POINT('',#34370);
#5051=VERTEX_POINT('',#34374);
#5052=VERTEX_POINT('',#34378);
#5053=VERTEX_POINT('',#34382);
#5054=VERTEX_POINT('',#34384);
#5055=VERTEX_POINT('',#34392);
#5056=VERTEX_POINT('',#34393);
#5057=VERTEX_POINT('',#34395);
#5058=VERTEX_POINT('',#34397);
#5059=VERTEX_POINT('',#34401);
#5060=VERTEX_POINT('',#34402);
#5061=VERTEX_POINT('',#34407);
#5062=VERTEX_POINT('',#34411);
#5063=VERTEX_POINT('',#34417);
#5064=VERTEX_POINT('',#34418);
#5065=VERTEX_POINT('',#34420);
#5066=VERTEX_POINT('',#34422);
#5067=VERTEX_POINT('',#34426);
#5068=VERTEX_POINT('',#34428);
#5069=VERTEX_POINT('',#34432);
#5070=VERTEX_POINT('',#34433);
#5071=VERTEX_POINT('',#34435);
#5072=VERTEX_POINT('',#34437);
#5073=VERTEX_POINT('',#34439);
#5074=VERTEX_POINT('',#34441);
#5075=VERTEX_POINT('',#34443);
#5076=VERTEX_POINT('',#34445);
#5077=VERTEX_POINT('',#34449);
#5078=VERTEX_POINT('',#34451);
#5079=VERTEX_POINT('',#34455);
#5080=VERTEX_POINT('',#34459);
#5081=VERTEX_POINT('',#34463);
#5082=VERTEX_POINT('',#34465);
#5083=VERTEX_POINT('',#34469);
#5084=VERTEX_POINT('',#34473);
#5085=VERTEX_POINT('',#34477);
#5086=VERTEX_POINT('',#34481);
#5087=VERTEX_POINT('',#34485);
#5088=VERTEX_POINT('',#34489);
#5089=VERTEX_POINT('',#34493);
#5090=VERTEX_POINT('',#34497);
#5091=VERTEX_POINT('',#34501);
#5092=VERTEX_POINT('',#34505);
#5093=VERTEX_POINT('',#34507);
#5094=VERTEX_POINT('',#34511);
#5095=VERTEX_POINT('',#34515);
#5096=VERTEX_POINT('',#34522);
#5097=VERTEX_POINT('',#34530);
#5098=VERTEX_POINT('',#34532);
#5099=VERTEX_POINT('',#34536);
#5100=VERTEX_POINT('',#34538);
#5101=VERTEX_POINT('',#34542);
#5102=VERTEX_POINT('',#34544);
#5103=VERTEX_POINT('',#34548);
#5104=VERTEX_POINT('',#34550);
#5105=VERTEX_POINT('',#34554);
#5106=VERTEX_POINT('',#34556);
#5107=VERTEX_POINT('',#34560);
#5108=VERTEX_POINT('',#34561);
#5109=VERTEX_POINT('',#34563);
#5110=VERTEX_POINT('',#34565);
#5111=VERTEX_POINT('',#34567);
#5112=VERTEX_POINT('',#34569);
#5113=VERTEX_POINT('',#34571);
#5114=VERTEX_POINT('',#34573);
#5115=VERTEX_POINT('',#34577);
#5116=VERTEX_POINT('',#34578);
#5117=VERTEX_POINT('',#34580);
#5118=VERTEX_POINT('',#34582);
#5119=VERTEX_POINT('',#34584);
#5120=VERTEX_POINT('',#34586);
#5121=VERTEX_POINT('',#34588);
#5122=VERTEX_POINT('',#34590);
#5123=VERTEX_POINT('',#34616);
#5124=VERTEX_POINT('',#34618);
#5125=VERTEX_POINT('',#34622);
#5126=VERTEX_POINT('',#34626);
#5127=VERTEX_POINT('',#34629);
#5128=VERTEX_POINT('',#34633);
#5129=VERTEX_POINT('',#34639);
#5130=VERTEX_POINT('',#34641);
#5131=VERTEX_POINT('',#34645);
#5132=VERTEX_POINT('',#34647);
#5133=VERTEX_POINT('',#34654);
#5134=VERTEX_POINT('',#34656);
#5135=VERTEX_POINT('',#34660);
#5136=VERTEX_POINT('',#34662);
#5137=VERTEX_POINT('',#34666);
#5138=VERTEX_POINT('',#34667);
#5139=VERTEX_POINT('',#34669);
#5140=VERTEX_POINT('',#34673);
#5141=VERTEX_POINT('',#34679);
#5142=VERTEX_POINT('',#34683);
#5143=VERTEX_POINT('',#34689);
#5144=VERTEX_POINT('',#34690);
#5145=VERTEX_POINT('',#34694);
#5146=VERTEX_POINT('',#34697);
#5147=VERTEX_POINT('',#34701);
#5148=VERTEX_POINT('',#34712);
#5149=VERTEX_POINT('',#34718);
#5150=VERTEX_POINT('',#34722);
#5151=VERTEX_POINT('',#34728);
#5152=VERTEX_POINT('',#34738);
#5153=VERTEX_POINT('',#34747);
#5154=VERTEX_POINT('',#34749);
#5155=VERTEX_POINT('',#34753);
#5156=VERTEX_POINT('',#34757);
#5157=VERTEX_POINT('',#34761);
#5158=VERTEX_POINT('',#34763);
#5159=VERTEX_POINT('',#34767);
#5160=VERTEX_POINT('',#34768);
#5161=VERTEX_POINT('',#34773);
#5162=VERTEX_POINT('',#34779);
#5163=VERTEX_POINT('',#34781);
#5164=VERTEX_POINT('',#34785);
#5165=VERTEX_POINT('',#34789);
#5166=VERTEX_POINT('',#34791);
#5167=VERTEX_POINT('',#34795);
#5168=VERTEX_POINT('',#34801);
#5169=VERTEX_POINT('',#34803);
#5170=VERTEX_POINT('',#34807);
#5171=VERTEX_POINT('',#34808);
#5172=VERTEX_POINT('',#34813);
#5173=VERTEX_POINT('',#34817);
#5174=VERTEX_POINT('',#34819);
#5175=VERTEX_POINT('',#34823);
#5176=VERTEX_POINT('',#34827);
#5177=VERTEX_POINT('',#34829);
#5178=VERTEX_POINT('',#34833);
#5179=VERTEX_POINT('',#34840);
#5180=VERTEX_POINT('',#34841);
#5181=VERTEX_POINT('',#34844);
#5182=VERTEX_POINT('',#34845);
#5183=VERTEX_POINT('',#34848);
#5184=VERTEX_POINT('',#34849);
#5185=VERTEX_POINT('',#34852);
#5186=VERTEX_POINT('',#34853);
#5187=VERTEX_POINT('',#34856);
#5188=VERTEX_POINT('',#34857);
#5189=VERTEX_POINT('',#34860);
#5190=VERTEX_POINT('',#34861);
#5191=VERTEX_POINT('',#34864);
#5192=VERTEX_POINT('',#34865);
#5193=VERTEX_POINT('',#34868);
#5194=VERTEX_POINT('',#34869);
#5195=VERTEX_POINT('',#34872);
#5196=VERTEX_POINT('',#34873);
#5197=VERTEX_POINT('',#34876);
#5198=VERTEX_POINT('',#34877);
#5199=VERTEX_POINT('',#34886);
#5200=VERTEX_POINT('',#34887);
#5201=VERTEX_POINT('',#34889);
#5202=VERTEX_POINT('',#34891);
#5203=VERTEX_POINT('',#34895);
#5204=VERTEX_POINT('',#34896);
#5205=VERTEX_POINT('',#34898);
#5206=VERTEX_POINT('',#34900);
#5207=VERTEX_POINT('',#34904);
#5208=VERTEX_POINT('',#34905);
#5209=VERTEX_POINT('',#34907);
#5210=VERTEX_POINT('',#34909);
#5211=VERTEX_POINT('',#34913);
#5212=VERTEX_POINT('',#34914);
#5213=VERTEX_POINT('',#34916);
#5214=VERTEX_POINT('',#34918);
#5215=VERTEX_POINT('',#34922);
#5216=VERTEX_POINT('',#34923);
#5217=VERTEX_POINT('',#34925);
#5218=VERTEX_POINT('',#34927);
#5219=VERTEX_POINT('',#34931);
#5220=VERTEX_POINT('',#34933);
#5221=VERTEX_POINT('',#34937);
#5222=VERTEX_POINT('',#34938);
#5223=VERTEX_POINT('',#34940);
#5224=VERTEX_POINT('',#34942);
#5225=VERTEX_POINT('',#34946);
#5226=VERTEX_POINT('',#34947);
#5227=VERTEX_POINT('',#34949);
#5228=VERTEX_POINT('',#34951);
#5229=VERTEX_POINT('',#34958);
#5230=VERTEX_POINT('',#34960);
#5231=VERTEX_POINT('',#34964);
#5232=VERTEX_POINT('',#34966);
#5233=VERTEX_POINT('',#34970);
#5234=VERTEX_POINT('',#34972);
#5235=VERTEX_POINT('',#34976);
#5236=VERTEX_POINT('',#34978);
#5237=VERTEX_POINT('',#34982);
#5238=VERTEX_POINT('',#34984);
#5239=VERTEX_POINT('',#34988);
#5240=VERTEX_POINT('',#34990);
#5241=VERTEX_POINT('',#34994);
#5242=VERTEX_POINT('',#34996);
#5243=VERTEX_POINT('',#35000);
#5244=VERTEX_POINT('',#35002);
#5245=VERTEX_POINT('',#35006);
#5246=VERTEX_POINT('',#35008);
#5247=VERTEX_POINT('',#35012);
#5248=VERTEX_POINT('',#35014);
#5249=VERTEX_POINT('',#35021);
#5250=VERTEX_POINT('',#35022);
#5251=VERTEX_POINT('',#35024);
#5252=VERTEX_POINT('',#35026);
#5253=VERTEX_POINT('',#35036);
#5254=VERTEX_POINT('',#35037);
#5255=VERTEX_POINT('',#35039);
#5256=VERTEX_POINT('',#35041);
#5257=VERTEX_POINT('',#35045);
#5258=VERTEX_POINT('',#35047);
#5259=VERTEX_POINT('',#35054);
#5260=VERTEX_POINT('',#35055);
#5261=VERTEX_POINT('',#35057);
#5262=VERTEX_POINT('',#35059);
#5263=VERTEX_POINT('',#35066);
#5264=VERTEX_POINT('',#35068);
#5265=VERTEX_POINT('',#35072);
#5266=VERTEX_POINT('',#35074);
#5267=VERTEX_POINT('',#35078);
#5268=VERTEX_POINT('',#35080);
#5269=VERTEX_POINT('',#35084);
#5270=VERTEX_POINT('',#35086);
#5271=VERTEX_POINT('',#35090);
#5272=VERTEX_POINT('',#35092);
#5273=VERTEX_POINT('',#35096);
#5274=VERTEX_POINT('',#35098);
#5275=VERTEX_POINT('',#35102);
#5276=VERTEX_POINT('',#35104);
#5277=VERTEX_POINT('',#35108);
#5278=VERTEX_POINT('',#35110);
#5279=VERTEX_POINT('',#35114);
#5280=VERTEX_POINT('',#35116);
#5281=VERTEX_POINT('',#35120);
#5282=VERTEX_POINT('',#35122);
#5283=VERTEX_POINT('',#35132);
#5284=VERTEX_POINT('',#35134);
#5285=VERTEX_POINT('',#35138);
#5286=VERTEX_POINT('',#35140);
#5287=VERTEX_POINT('',#35144);
#5288=VERTEX_POINT('',#35146);
#5289=VERTEX_POINT('',#35150);
#5290=VERTEX_POINT('',#35152);
#5291=VERTEX_POINT('',#35156);
#5292=VERTEX_POINT('',#35158);
#5293=VERTEX_POINT('',#35162);
#5294=VERTEX_POINT('',#35164);
#5295=VERTEX_POINT('',#35168);
#5296=VERTEX_POINT('',#35170);
#5297=VERTEX_POINT('',#35174);
#5298=VERTEX_POINT('',#35176);
#5299=VERTEX_POINT('',#35178);
#5300=VERTEX_POINT('',#35180);
#5301=VERTEX_POINT('',#35182);
#5302=VERTEX_POINT('',#35184);
#5303=VERTEX_POINT('',#35186);
#5304=VERTEX_POINT('',#35188);
#5305=VERTEX_POINT('',#35190);
#5306=VERTEX_POINT('',#35192);
#5307=VERTEX_POINT('',#35194);
#5308=VERTEX_POINT('',#35196);
#5309=VERTEX_POINT('',#35198);
#5310=VERTEX_POINT('',#35200);
#5311=VERTEX_POINT('',#35202);
#5312=VERTEX_POINT('',#35204);
#5313=VERTEX_POINT('',#35206);
#5314=VERTEX_POINT('',#35208);
#5315=VERTEX_POINT('',#35210);
#5316=VERTEX_POINT('',#35212);
#5317=VERTEX_POINT('',#35214);
#5318=VERTEX_POINT('',#35216);
#5319=VERTEX_POINT('',#35218);
#5320=VERTEX_POINT('',#35220);
#5321=VERTEX_POINT('',#35222);
#5322=VERTEX_POINT('',#35224);
#5323=VERTEX_POINT('',#35226);
#5324=VERTEX_POINT('',#35228);
#5325=VERTEX_POINT('',#35230);
#5326=VERTEX_POINT('',#35232);
#5327=VERTEX_POINT('',#35234);
#5328=VERTEX_POINT('',#35236);
#5329=VERTEX_POINT('',#35238);
#5330=VERTEX_POINT('',#35240);
#5331=VERTEX_POINT('',#35242);
#5332=VERTEX_POINT('',#35244);
#5333=VERTEX_POINT('',#35246);
#5334=VERTEX_POINT('',#35248);
#5335=VERTEX_POINT('',#35250);
#5336=VERTEX_POINT('',#35252);
#5337=VERTEX_POINT('',#35255);
#5338=VERTEX_POINT('',#35257);
#5339=VERTEX_POINT('',#35259);
#5340=VERTEX_POINT('',#35261);
#5341=VERTEX_POINT('',#35264);
#5342=VERTEX_POINT('',#35267);
#5343=VERTEX_POINT('',#35271);
#5344=VERTEX_POINT('',#35275);
#5345=VERTEX_POINT('',#35277);
#5346=VERTEX_POINT('',#35281);
#5347=VERTEX_POINT('',#35283);
#5348=VERTEX_POINT('',#35287);
#5349=VERTEX_POINT('',#35289);
#5350=VERTEX_POINT('',#35293);
#5351=VERTEX_POINT('',#35297);
#5352=VERTEX_POINT('',#35299);
#5353=VERTEX_POINT('',#35303);
#5354=VERTEX_POINT('',#35305);
#5355=VERTEX_POINT('',#35311);
#5356=VERTEX_POINT('',#35315);
#5357=VERTEX_POINT('',#35319);
#5358=VERTEX_POINT('',#35323);
#5359=VERTEX_POINT('',#35327);
#5360=VERTEX_POINT('',#35331);
#5361=VERTEX_POINT('',#35335);
#5362=VERTEX_POINT('',#35339);
#5363=VERTEX_POINT('',#35343);
#5364=VERTEX_POINT('',#35347);
#5365=VERTEX_POINT('',#35353);
#5366=VERTEX_POINT('',#35355);
#5367=VERTEX_POINT('',#35363);
#5368=VERTEX_POINT('',#35367);
#5369=VERTEX_POINT('',#35371);
#5370=VERTEX_POINT('',#35377);
#5371=VERTEX_POINT('',#35379);
#5372=VERTEX_POINT('',#35385);
#5373=VERTEX_POINT('',#35389);
#5374=VERTEX_POINT('',#35393);
#5375=VERTEX_POINT('',#35397);
#5376=VERTEX_POINT('',#35401);
#5377=VERTEX_POINT('',#35405);
#5378=VERTEX_POINT('',#35409);
#5379=VERTEX_POINT('',#35413);
#5380=VERTEX_POINT('',#35417);
#5381=VERTEX_POINT('',#35421);
#5382=VERTEX_POINT('',#35429);
#5383=VERTEX_POINT('',#35433);
#5384=VERTEX_POINT('',#35437);
#5385=VERTEX_POINT('',#35441);
#5386=VERTEX_POINT('',#35445);
#5387=VERTEX_POINT('',#35453);
#5388=VERTEX_POINT('',#35455);
#5389=VERTEX_POINT('',#35458);
#5390=VERTEX_POINT('',#35460);
#5391=VERTEX_POINT('',#35464);
#5392=VERTEX_POINT('',#35467);
#5393=VERTEX_POINT('',#35470);
#5394=VERTEX_POINT('',#35476);
#5395=VERTEX_POINT('',#35482);
#5396=VERTEX_POINT('',#35484);
#5397=VERTEX_POINT('',#35488);
#5398=VERTEX_POINT('',#35489);
#5399=VERTEX_POINT('',#35491);
#5400=VERTEX_POINT('',#35493);
#5401=VERTEX_POINT('',#35497);
#5402=VERTEX_POINT('',#35499);
#5403=VERTEX_POINT('',#35503);
#5404=VERTEX_POINT('',#35505);
#5405=VERTEX_POINT('',#35512);
#5406=VERTEX_POINT('',#35513);
#5407=VERTEX_POINT('',#35515);
#5408=VERTEX_POINT('',#35517);
#5409=VERTEX_POINT('',#35521);
#5410=VERTEX_POINT('',#35523);
#5411=VERTEX_POINT('',#35527);
#5412=VERTEX_POINT('',#35529);
#5413=VERTEX_POINT('',#35536);
#5414=VERTEX_POINT('',#35538);
#5415=VERTEX_POINT('',#35542);
#5416=VERTEX_POINT('',#35544);
#5417=VERTEX_POINT('',#35548);
#5418=VERTEX_POINT('',#35549);
#5419=VERTEX_POINT('',#35551);
#5420=VERTEX_POINT('',#35553);
#5421=VERTEX_POINT('',#35557);
#5422=VERTEX_POINT('',#35559);
#5423=VERTEX_POINT('',#35563);
#5424=VERTEX_POINT('',#35565);
#5425=VERTEX_POINT('',#35572);
#5426=VERTEX_POINT('',#35574);
#5427=VERTEX_POINT('',#35578);
#5428=VERTEX_POINT('',#35580);
#5429=VERTEX_POINT('',#35584);
#5430=VERTEX_POINT('',#35585);
#5431=VERTEX_POINT('',#35587);
#5432=VERTEX_POINT('',#35589);
#5433=VERTEX_POINT('',#35593);
#5434=VERTEX_POINT('',#35595);
#5435=VERTEX_POINT('',#35599);
#5436=VERTEX_POINT('',#35601);
#5437=VERTEX_POINT('',#35605);
#5438=VERTEX_POINT('',#35607);
#5439=VERTEX_POINT('',#35611);
#5440=VERTEX_POINT('',#35613);
#5441=VERTEX_POINT('',#35617);
#5442=VERTEX_POINT('',#35619);
#5443=VERTEX_POINT('',#35623);
#5444=VERTEX_POINT('',#35625);
#5445=VERTEX_POINT('',#35629);
#5446=VERTEX_POINT('',#35631);
#5447=VERTEX_POINT('',#35635);
#5448=VERTEX_POINT('',#35637);
#5449=VERTEX_POINT('',#35641);
#5450=VERTEX_POINT('',#35643);
#5451=VERTEX_POINT('',#35647);
#5452=VERTEX_POINT('',#35649);
#5453=VERTEX_POINT('',#35653);
#5454=VERTEX_POINT('',#35655);
#5455=VERTEX_POINT('',#35659);
#5456=VERTEX_POINT('',#35661);
#5457=VERTEX_POINT('',#35665);
#5458=VERTEX_POINT('',#35667);
#5459=VERTEX_POINT('',#35671);
#5460=VERTEX_POINT('',#35673);
#5461=VERTEX_POINT('',#35683);
#5462=VERTEX_POINT('',#35718);
#5463=VERTEX_POINT('',#35755);
#5464=VERTEX_POINT('',#35756);
#5465=VERTEX_POINT('',#35767);
#5466=VERTEX_POINT('',#35796);
#5467=VERTEX_POINT('',#35798);
#5468=VERTEX_POINT('',#35809);
#5469=VERTEX_POINT('',#35839);
#5470=VERTEX_POINT('',#35842);
#5471=VERTEX_POINT('',#35846);
#5472=VERTEX_POINT('',#35849);
#5473=VERTEX_POINT('',#35851);
#5474=VERTEX_POINT('',#35854);
#5475=VERTEX_POINT('',#35859);
#5476=VERTEX_POINT('',#35863);
#5477=VERTEX_POINT('',#35868);
#5478=VERTEX_POINT('',#35870);
#5479=VERTEX_POINT('',#35877);
#5480=VERTEX_POINT('',#35878);
#5481=VERTEX_POINT('',#35880);
#5482=VERTEX_POINT('',#35882);
#5483=VERTEX_POINT('',#35885);
#5484=VERTEX_POINT('',#35886);
#5485=VERTEX_POINT('',#35888);
#5486=VERTEX_POINT('',#35890);
#5487=VERTEX_POINT('',#35894);
#5488=VERTEX_POINT('',#35896);
#5489=VERTEX_POINT('',#35900);
#5490=VERTEX_POINT('',#35904);
#5491=VERTEX_POINT('',#35910);
#5492=VERTEX_POINT('',#35912);
#5493=VERTEX_POINT('',#35916);
#5494=VERTEX_POINT('',#35920);
#5495=VERTEX_POINT('',#35928);
#5496=VERTEX_POINT('',#35930);
#5497=VERTEX_POINT('',#35934);
#5498=VERTEX_POINT('',#35935);
#5499=VERTEX_POINT('',#35937);
#5500=VERTEX_POINT('',#35939);
#5501=VERTEX_POINT('',#35943);
#5502=VERTEX_POINT('',#35945);
#5503=VERTEX_POINT('',#35949);
#5504=VERTEX_POINT('',#35951);
#5505=VERTEX_POINT('',#35958);
#5506=VERTEX_POINT('',#35960);
#5507=VERTEX_POINT('',#35964);
#5508=VERTEX_POINT('',#35966);
#5509=VERTEX_POINT('',#35970);
#5510=VERTEX_POINT('',#35972);
#5511=VERTEX_POINT('',#35976);
#5512=VERTEX_POINT('',#35978);
#5513=VERTEX_POINT('',#35982);
#5514=VERTEX_POINT('',#35984);
#5515=VERTEX_POINT('',#35988);
#5516=VERTEX_POINT('',#35989);
#5517=VERTEX_POINT('',#35991);
#5518=VERTEX_POINT('',#35993);
#5519=VERTEX_POINT('',#35997);
#5520=VERTEX_POINT('',#35999);
#5521=VERTEX_POINT('',#36003);
#5522=VERTEX_POINT('',#36005);
#5523=VERTEX_POINT('',#36012);
#5524=VERTEX_POINT('',#36013);
#5525=VERTEX_POINT('',#36015);
#5526=VERTEX_POINT('',#36017);
#5527=VERTEX_POINT('',#36021);
#5528=VERTEX_POINT('',#36023);
#5529=VERTEX_POINT('',#36027);
#5530=VERTEX_POINT('',#36029);
#5531=VERTEX_POINT('',#36036);
#5532=VERTEX_POINT('',#36038);
#5533=VERTEX_POINT('',#36042);
#5534=VERTEX_POINT('',#36044);
#5535=VERTEX_POINT('',#36048);
#5536=VERTEX_POINT('',#36050);
#5537=VERTEX_POINT('',#36054);
#5538=VERTEX_POINT('',#36056);
#5539=VERTEX_POINT('',#36060);
#5540=VERTEX_POINT('',#36062);
#5541=VERTEX_POINT('',#36066);
#5542=VERTEX_POINT('',#36067);
#5543=VERTEX_POINT('',#36069);
#5544=VERTEX_POINT('',#36071);
#5545=VERTEX_POINT('',#36075);
#5546=VERTEX_POINT('',#36077);
#5547=VERTEX_POINT('',#36081);
#5548=VERTEX_POINT('',#36083);
#5549=VERTEX_POINT('',#36090);
#5550=VERTEX_POINT('',#36092);
#5551=VERTEX_POINT('',#36096);
#5552=VERTEX_POINT('',#36098);
#5553=VERTEX_POINT('',#36102);
#5554=VERTEX_POINT('',#36103);
#5555=VERTEX_POINT('',#36105);
#5556=VERTEX_POINT('',#36107);
#5557=VERTEX_POINT('',#36111);
#5558=VERTEX_POINT('',#36113);
#5559=VERTEX_POINT('',#36117);
#5560=VERTEX_POINT('',#36119);
#5561=VERTEX_POINT('',#36126);
#5562=VERTEX_POINT('',#36127);
#5563=VERTEX_POINT('',#36129);
#5564=VERTEX_POINT('',#36131);
#5565=VERTEX_POINT('',#36135);
#5566=VERTEX_POINT('',#36137);
#5567=VERTEX_POINT('',#36141);
#5568=VERTEX_POINT('',#36143);
#5569=VERTEX_POINT('',#36150);
#5570=VERTEX_POINT('',#36151);
#5571=VERTEX_POINT('',#36153);
#5572=VERTEX_POINT('',#36155);
#5573=VERTEX_POINT('',#36159);
#5574=VERTEX_POINT('',#36161);
#5575=VERTEX_POINT('',#36165);
#5576=VERTEX_POINT('',#36167);
#5577=VERTEX_POINT('',#36174);
#5578=VERTEX_POINT('',#36175);
#5579=VERTEX_POINT('',#36177);
#5580=VERTEX_POINT('',#36179);
#5581=VERTEX_POINT('',#36183);
#5582=VERTEX_POINT('',#36185);
#5583=VERTEX_POINT('',#36189);
#5584=VERTEX_POINT('',#36191);
#5585=VERTEX_POINT('',#36198);
#5586=VERTEX_POINT('',#36200);
#5587=VERTEX_POINT('',#36204);
#5588=VERTEX_POINT('',#36206);
#5589=VERTEX_POINT('',#36210);
#5590=VERTEX_POINT('',#36211);
#5591=VERTEX_POINT('',#36213);
#5592=VERTEX_POINT('',#36215);
#5593=VERTEX_POINT('',#36219);
#5594=VERTEX_POINT('',#36221);
#5595=VERTEX_POINT('',#36225);
#5596=VERTEX_POINT('',#36227);
#5597=VERTEX_POINT('',#36231);
#5598=VERTEX_POINT('',#36233);
#5599=VERTEX_POINT('',#36237);
#5600=VERTEX_POINT('',#36239);
#5601=VERTEX_POINT('',#36243);
#5602=VERTEX_POINT('',#36245);
#5603=VERTEX_POINT('',#36249);
#5604=VERTEX_POINT('',#36251);
#5605=VERTEX_POINT('',#36261);
#5606=VERTEX_POINT('',#36263);
#5607=VERTEX_POINT('',#36267);
#5608=VERTEX_POINT('',#36269);
#5609=VERTEX_POINT('',#36273);
#5610=VERTEX_POINT('',#36275);
#5611=VERTEX_POINT('',#36279);
#5612=VERTEX_POINT('',#36281);
#5613=VERTEX_POINT('',#36285);
#5614=VERTEX_POINT('',#36287);
#5615=VERTEX_POINT('',#36291);
#5616=VERTEX_POINT('',#36292);
#5617=VERTEX_POINT('',#36294);
#5618=VERTEX_POINT('',#36296);
#5619=VERTEX_POINT('',#36300);
#5620=VERTEX_POINT('',#36302);
#5621=VERTEX_POINT('',#36306);
#5622=VERTEX_POINT('',#36308);
#5623=VERTEX_POINT('',#36312);
#5624=VERTEX_POINT('',#36314);
#5625=VERTEX_POINT('',#36318);
#5626=VERTEX_POINT('',#36320);
#5627=VERTEX_POINT('',#36324);
#5628=VERTEX_POINT('',#36326);
#5629=VERTEX_POINT('',#36330);
#5630=VERTEX_POINT('',#36332);
#5631=VERTEX_POINT('',#36342);
#5632=VERTEX_POINT('',#36344);
#5633=VERTEX_POINT('',#36348);
#5634=VERTEX_POINT('',#36350);
#5635=VERTEX_POINT('',#36354);
#5636=VERTEX_POINT('',#36359);
#5637=VERTEX_POINT('',#36360);
#5638=VERTEX_POINT('',#36362);
#5639=VERTEX_POINT('',#36366);
#5640=VERTEX_POINT('',#36370);
#5641=VERTEX_POINT('',#36374);
#5642=VERTEX_POINT('',#36378);
#5643=VERTEX_POINT('',#36384);
#5644=VERTEX_POINT('',#36385);
#5645=VERTEX_POINT('',#36390);
#5646=VERTEX_POINT('',#36394);
#5647=VERTEX_POINT('',#36398);
#5648=VERTEX_POINT('',#36402);
#5649=VERTEX_POINT('',#36409);
#5650=EDGE_CURVE('',#4593,#4593,#4280,.T.);
#5651=EDGE_CURVE('',#4593,#4594,#2388,.T.);
#5652=EDGE_CURVE('',#4594,#4595,#4281,.T.);
#5653=EDGE_CURVE('',#4595,#4594,#4282,.T.);
#5654=EDGE_CURVE('',#4596,#4597,#762,.F.);
#5655=EDGE_CURVE('',#4597,#4595,#4283,.T.);
#5656=EDGE_CURVE('',#4597,#4598,#763,.F.);
#5657=EDGE_CURVE('',#4598,#4599,#714,.T.);
#5658=EDGE_CURVE('',#4600,#4599,#4284,.T.);
#5659=EDGE_CURVE('',#4601,#4600,#715,.T.);
#5660=EDGE_CURVE('',#4601,#4602,#764,.T.);
#5661=EDGE_CURVE('',#4602,#4603,#716,.T.);
#5662=EDGE_CURVE('',#4604,#4603,#4285,.T.);
#5663=EDGE_CURVE('',#4604,#4605,#717,.T.);
#5664=EDGE_CURVE('',#4605,#4606,#765,.F.);
#5665=EDGE_CURVE('',#4607,#4606,#718,.T.);
#5666=EDGE_CURVE('',#4608,#4607,#4286,.T.);
#5667=EDGE_CURVE('',#4608,#4609,#719,.T.);
#5668=EDGE_CURVE('',#4609,#4610,#766,.T.);
#5669=EDGE_CURVE('',#4611,#4610,#720,.T.);
#5670=EDGE_CURVE('',#4612,#4611,#4287,.T.);
#5671=EDGE_CURVE('',#4596,#4612,#721,.T.);
#5672=EDGE_CURVE('',#4603,#4613,#2389,.T.);
#5673=EDGE_CURVE('',#4613,#4604,#2390,.T.);
#5674=EDGE_CURVE('',#4614,#4607,#2391,.T.);
#5675=EDGE_CURVE('',#4614,#4608,#2392,.T.);
#5676=EDGE_CURVE('',#4615,#4611,#2393,.T.);
#5677=EDGE_CURVE('',#4612,#4615,#2394,.T.);
#5678=EDGE_CURVE('',#4600,#4616,#2395,.T.);
#5679=EDGE_CURVE('',#4599,#4616,#2396,.T.);
#5680=EDGE_CURVE('',#4617,#4616,#2397,.T.);
#5681=EDGE_CURVE('',#4618,#4617,#2398,.T.);
#5682=EDGE_CURVE('',#4618,#4601,#2399,.T.);
#5683=EDGE_CURVE('',#4619,#4602,#2400,.T.);
#5684=EDGE_CURVE('',#4619,#4620,#2401,.T.);
#5685=EDGE_CURVE('',#4620,#4613,#2402,.T.);
#5686=EDGE_CURVE('',#4621,#4610,#2403,.T.);
#5687=EDGE_CURVE('',#4622,#4621,#2404,.T.);
#5688=EDGE_CURVE('',#4622,#4615,#2405,.T.);
#5689=EDGE_CURVE('',#4618,#4619,#2406,.T.);
#5690=EDGE_CURVE('',#4623,#4614,#2407,.T.);
#5691=EDGE_CURVE('',#4623,#4624,#2408,.T.);
#5692=EDGE_CURVE('',#4624,#4609,#2409,.T.);
#5693=EDGE_CURVE('',#4624,#4621,#2410,.T.);
#5694=EDGE_CURVE('',#4623,#4625,#2411,.T.);
#5695=EDGE_CURVE('',#4626,#4625,#2412,.T.);
#5696=EDGE_CURVE('',#4620,#4626,#2413,.T.);
#5697=EDGE_CURVE('',#4627,#4617,#2414,.T.);
#5698=EDGE_CURVE('',#4628,#4627,#2415,.T.);
#5699=EDGE_CURVE('',#4628,#4622,#2416,.T.);
#5700=EDGE_CURVE('',#4626,#4605,#2417,.T.);
#5701=EDGE_CURVE('',#4625,#4606,#2418,.T.);
#5702=EDGE_CURVE('',#4628,#4596,#2419,.T.);
#5703=EDGE_CURVE('',#4627,#4598,#2420,.T.);
#5704=EDGE_CURVE('',#4629,#4629,#4288,.T.);
#5705=EDGE_CURVE('',#4629,#4630,#2421,.T.);
#5706=EDGE_CURVE('',#4630,#4631,#4289,.T.);
#5707=EDGE_CURVE('',#4631,#4630,#4290,.T.);
#5708=EDGE_CURVE('',#4632,#4633,#767,.F.);
#5709=EDGE_CURVE('',#4633,#4631,#4291,.T.);
#5710=EDGE_CURVE('',#4633,#4634,#768,.F.);
#5711=EDGE_CURVE('',#4634,#4635,#722,.T.);
#5712=EDGE_CURVE('',#4636,#4635,#4292,.T.);
#5713=EDGE_CURVE('',#4637,#4636,#723,.T.);
#5714=EDGE_CURVE('',#4637,#4638,#769,.T.);
#5715=EDGE_CURVE('',#4638,#4639,#724,.T.);
#5716=EDGE_CURVE('',#4640,#4639,#4293,.T.);
#5717=EDGE_CURVE('',#4640,#4641,#725,.T.);
#5718=EDGE_CURVE('',#4641,#4642,#770,.F.);
#5719=EDGE_CURVE('',#4643,#4642,#726,.T.);
#5720=EDGE_CURVE('',#4644,#4643,#4294,.T.);
#5721=EDGE_CURVE('',#4644,#4645,#727,.T.);
#5722=EDGE_CURVE('',#4645,#4646,#771,.T.);
#5723=EDGE_CURVE('',#4647,#4646,#728,.T.);
#5724=EDGE_CURVE('',#4648,#4647,#4295,.T.);
#5725=EDGE_CURVE('',#4632,#4648,#729,.T.);
#5726=EDGE_CURVE('',#4639,#4649,#2422,.T.);
#5727=EDGE_CURVE('',#4649,#4640,#2423,.T.);
#5728=EDGE_CURVE('',#4650,#4643,#2424,.T.);
#5729=EDGE_CURVE('',#4650,#4644,#2425,.T.);
#5730=EDGE_CURVE('',#4651,#4647,#2426,.T.);
#5731=EDGE_CURVE('',#4648,#4651,#2427,.T.);
#5732=EDGE_CURVE('',#4636,#4652,#2428,.T.);
#5733=EDGE_CURVE('',#4635,#4652,#2429,.T.);
#5734=EDGE_CURVE('',#4653,#4652,#2430,.T.);
#5735=EDGE_CURVE('',#4654,#4653,#2431,.T.);
#5736=EDGE_CURVE('',#4654,#4637,#2432,.T.);
#5737=EDGE_CURVE('',#4655,#4638,#2433,.T.);
#5738=EDGE_CURVE('',#4655,#4656,#2434,.T.);
#5739=EDGE_CURVE('',#4656,#4649,#2435,.T.);
#5740=EDGE_CURVE('',#4657,#4646,#2436,.T.);
#5741=EDGE_CURVE('',#4658,#4657,#2437,.T.);
#5742=EDGE_CURVE('',#4658,#4651,#2438,.T.);
#5743=EDGE_CURVE('',#4654,#4655,#2439,.T.);
#5744=EDGE_CURVE('',#4659,#4650,#2440,.T.);
#5745=EDGE_CURVE('',#4659,#4660,#2441,.T.);
#5746=EDGE_CURVE('',#4660,#4645,#2442,.T.);
#5747=EDGE_CURVE('',#4660,#4657,#2443,.T.);
#5748=EDGE_CURVE('',#4659,#4661,#2444,.T.);
#5749=EDGE_CURVE('',#4662,#4661,#2445,.T.);
#5750=EDGE_CURVE('',#4656,#4662,#2446,.T.);
#5751=EDGE_CURVE('',#4663,#4653,#2447,.T.);
#5752=EDGE_CURVE('',#4664,#4663,#2448,.T.);
#5753=EDGE_CURVE('',#4664,#4658,#2449,.T.);
#5754=EDGE_CURVE('',#4662,#4641,#2450,.T.);
#5755=EDGE_CURVE('',#4661,#4642,#2451,.T.);
#5756=EDGE_CURVE('',#4664,#4632,#2452,.T.);
#5757=EDGE_CURVE('',#4663,#4634,#2453,.T.);
#5758=EDGE_CURVE('',#4665,#4665,#4296,.T.);
#5759=EDGE_CURVE('',#4665,#4666,#2454,.T.);
#5760=EDGE_CURVE('',#4666,#4667,#4297,.T.);
#5761=EDGE_CURVE('',#4667,#4666,#4298,.T.);
#5762=EDGE_CURVE('',#4668,#4669,#772,.F.);
#5763=EDGE_CURVE('',#4669,#4667,#4299,.T.);
#5764=EDGE_CURVE('',#4669,#4670,#773,.F.);
#5765=EDGE_CURVE('',#4670,#4671,#730,.T.);
#5766=EDGE_CURVE('',#4672,#4671,#4300,.T.);
#5767=EDGE_CURVE('',#4673,#4672,#731,.T.);
#5768=EDGE_CURVE('',#4673,#4674,#774,.T.);
#5769=EDGE_CURVE('',#4674,#4675,#732,.T.);
#5770=EDGE_CURVE('',#4676,#4675,#4301,.T.);
#5771=EDGE_CURVE('',#4676,#4677,#733,.T.);
#5772=EDGE_CURVE('',#4677,#4678,#775,.F.);
#5773=EDGE_CURVE('',#4679,#4678,#734,.T.);
#5774=EDGE_CURVE('',#4680,#4679,#4302,.T.);
#5775=EDGE_CURVE('',#4680,#4681,#735,.T.);
#5776=EDGE_CURVE('',#4681,#4682,#776,.T.);
#5777=EDGE_CURVE('',#4683,#4682,#736,.T.);
#5778=EDGE_CURVE('',#4684,#4683,#4303,.T.);
#5779=EDGE_CURVE('',#4668,#4684,#737,.T.);
#5780=EDGE_CURVE('',#4675,#4685,#2455,.T.);
#5781=EDGE_CURVE('',#4685,#4676,#2456,.T.);
#5782=EDGE_CURVE('',#4686,#4679,#2457,.T.);
#5783=EDGE_CURVE('',#4686,#4680,#2458,.T.);
#5784=EDGE_CURVE('',#4687,#4683,#2459,.T.);
#5785=EDGE_CURVE('',#4684,#4687,#2460,.T.);
#5786=EDGE_CURVE('',#4672,#4688,#2461,.T.);
#5787=EDGE_CURVE('',#4671,#4688,#2462,.T.);
#5788=EDGE_CURVE('',#4689,#4688,#2463,.T.);
#5789=EDGE_CURVE('',#4690,#4689,#2464,.T.);
#5790=EDGE_CURVE('',#4690,#4673,#2465,.T.);
#5791=EDGE_CURVE('',#4691,#4674,#2466,.T.);
#5792=EDGE_CURVE('',#4691,#4692,#2467,.T.);
#5793=EDGE_CURVE('',#4692,#4685,#2468,.T.);
#5794=EDGE_CURVE('',#4693,#4682,#2469,.T.);
#5795=EDGE_CURVE('',#4694,#4693,#2470,.T.);
#5796=EDGE_CURVE('',#4694,#4687,#2471,.T.);
#5797=EDGE_CURVE('',#4690,#4691,#2472,.T.);
#5798=EDGE_CURVE('',#4695,#4686,#2473,.T.);
#5799=EDGE_CURVE('',#4695,#4696,#2474,.T.);
#5800=EDGE_CURVE('',#4696,#4681,#2475,.T.);
#5801=EDGE_CURVE('',#4696,#4693,#2476,.T.);
#5802=EDGE_CURVE('',#4695,#4697,#2477,.T.);
#5803=EDGE_CURVE('',#4698,#4697,#2478,.T.);
#5804=EDGE_CURVE('',#4692,#4698,#2479,.T.);
#5805=EDGE_CURVE('',#4699,#4689,#2480,.T.);
#5806=EDGE_CURVE('',#4700,#4699,#2481,.T.);
#5807=EDGE_CURVE('',#4700,#4694,#2482,.T.);
#5808=EDGE_CURVE('',#4698,#4677,#2483,.T.);
#5809=EDGE_CURVE('',#4697,#4678,#2484,.T.);
#5810=EDGE_CURVE('',#4700,#4668,#2485,.T.);
#5811=EDGE_CURVE('',#4699,#4670,#2486,.T.);
#5812=EDGE_CURVE('',#4701,#4701,#4304,.T.);
#5813=EDGE_CURVE('',#4701,#4702,#2487,.T.);
#5814=EDGE_CURVE('',#4702,#4703,#4305,.T.);
#5815=EDGE_CURVE('',#4703,#4702,#4306,.T.);
#5816=EDGE_CURVE('',#4704,#4705,#777,.F.);
#5817=EDGE_CURVE('',#4705,#4703,#4307,.T.);
#5818=EDGE_CURVE('',#4705,#4706,#778,.F.);
#5819=EDGE_CURVE('',#4706,#4707,#738,.T.);
#5820=EDGE_CURVE('',#4708,#4707,#4308,.T.);
#5821=EDGE_CURVE('',#4709,#4708,#739,.T.);
#5822=EDGE_CURVE('',#4709,#4710,#779,.T.);
#5823=EDGE_CURVE('',#4710,#4711,#740,.T.);
#5824=EDGE_CURVE('',#4712,#4711,#4309,.T.);
#5825=EDGE_CURVE('',#4712,#4713,#741,.T.);
#5826=EDGE_CURVE('',#4713,#4714,#780,.F.);
#5827=EDGE_CURVE('',#4715,#4714,#742,.T.);
#5828=EDGE_CURVE('',#4716,#4715,#4310,.T.);
#5829=EDGE_CURVE('',#4716,#4717,#743,.T.);
#5830=EDGE_CURVE('',#4717,#4718,#781,.T.);
#5831=EDGE_CURVE('',#4719,#4718,#744,.T.);
#5832=EDGE_CURVE('',#4720,#4719,#4311,.T.);
#5833=EDGE_CURVE('',#4704,#4720,#745,.T.);
#5834=EDGE_CURVE('',#4711,#4721,#2488,.T.);
#5835=EDGE_CURVE('',#4721,#4712,#2489,.T.);
#5836=EDGE_CURVE('',#4722,#4715,#2490,.T.);
#5837=EDGE_CURVE('',#4722,#4716,#2491,.T.);
#5838=EDGE_CURVE('',#4723,#4719,#2492,.T.);
#5839=EDGE_CURVE('',#4720,#4723,#2493,.T.);
#5840=EDGE_CURVE('',#4708,#4724,#2494,.T.);
#5841=EDGE_CURVE('',#4707,#4724,#2495,.T.);
#5842=EDGE_CURVE('',#4725,#4724,#2496,.T.);
#5843=EDGE_CURVE('',#4726,#4725,#2497,.T.);
#5844=EDGE_CURVE('',#4726,#4709,#2498,.T.);
#5845=EDGE_CURVE('',#4727,#4710,#2499,.T.);
#5846=EDGE_CURVE('',#4727,#4728,#2500,.T.);
#5847=EDGE_CURVE('',#4728,#4721,#2501,.T.);
#5848=EDGE_CURVE('',#4729,#4718,#2502,.T.);
#5849=EDGE_CURVE('',#4730,#4729,#2503,.T.);
#5850=EDGE_CURVE('',#4730,#4723,#2504,.T.);
#5851=EDGE_CURVE('',#4726,#4727,#2505,.T.);
#5852=EDGE_CURVE('',#4731,#4722,#2506,.T.);
#5853=EDGE_CURVE('',#4731,#4732,#2507,.T.);
#5854=EDGE_CURVE('',#4732,#4717,#2508,.T.);
#5855=EDGE_CURVE('',#4732,#4729,#2509,.T.);
#5856=EDGE_CURVE('',#4731,#4733,#2510,.T.);
#5857=EDGE_CURVE('',#4734,#4733,#2511,.T.);
#5858=EDGE_CURVE('',#4728,#4734,#2512,.T.);
#5859=EDGE_CURVE('',#4735,#4725,#2513,.T.);
#5860=EDGE_CURVE('',#4736,#4735,#2514,.T.);
#5861=EDGE_CURVE('',#4736,#4730,#2515,.T.);
#5862=EDGE_CURVE('',#4734,#4713,#2516,.T.);
#5863=EDGE_CURVE('',#4733,#4714,#2517,.T.);
#5864=EDGE_CURVE('',#4736,#4704,#2518,.T.);
#5865=EDGE_CURVE('',#4735,#4706,#2519,.T.);
#5866=EDGE_CURVE('',#4737,#4738,#2520,.T.);
#5867=EDGE_CURVE('',#4737,#4739,#782,.T.);
#5868=EDGE_CURVE('',#4739,#4740,#4312,.T.);
#5869=EDGE_CURVE('',#4740,#4738,#783,.T.);
#5870=EDGE_CURVE('',#4741,#4742,#2521,.T.);
#5871=EDGE_CURVE('',#4741,#4737,#784,.T.);
#5872=EDGE_CURVE('',#4738,#4742,#785,.T.);
#5873=EDGE_CURVE('',#4743,#4744,#2522,.T.);
#5874=EDGE_CURVE('',#4743,#4741,#786,.T.);
#5875=EDGE_CURVE('',#4742,#4744,#787,.T.);
#5876=EDGE_CURVE('',#4745,#4746,#2523,.T.);
#5877=EDGE_CURVE('',#4745,#4743,#788,.T.);
#5878=EDGE_CURVE('',#4744,#4746,#789,.T.);
#5879=EDGE_CURVE('',#4747,#4748,#2524,.T.);
#5880=EDGE_CURVE('',#4747,#4745,#790,.T.);
#5881=EDGE_CURVE('',#4746,#4748,#791,.T.);
#5882=EDGE_CURVE('',#4749,#4750,#2525,.T.);
#5883=EDGE_CURVE('',#4749,#4747,#792,.T.);
#5884=EDGE_CURVE('',#4748,#4750,#793,.T.);
#5885=EDGE_CURVE('',#4751,#4752,#2526,.T.);
#5886=EDGE_CURVE('',#4751,#4749,#794,.T.);
#5887=EDGE_CURVE('',#4750,#4752,#795,.T.);
#5888=EDGE_CURVE('',#4753,#4754,#2527,.T.);
#5889=EDGE_CURVE('',#4753,#4751,#796,.T.);
#5890=EDGE_CURVE('',#4752,#4754,#797,.T.);
#5891=EDGE_CURVE('',#4755,#4756,#2528,.T.);
#5892=EDGE_CURVE('',#4755,#4753,#798,.T.);
#5893=EDGE_CURVE('',#4754,#4756,#799,.T.);
#5894=EDGE_CURVE('',#4757,#4758,#2529,.T.);
#5895=EDGE_CURVE('',#4757,#4755,#800,.T.);
#5896=EDGE_CURVE('',#4756,#4758,#801,.T.);
#5897=EDGE_CURVE('',#4759,#4760,#2530,.T.);
#5898=EDGE_CURVE('',#4759,#4757,#802,.T.);
#5899=EDGE_CURVE('',#4758,#4760,#803,.T.);
#5900=EDGE_CURVE('',#4761,#4762,#2531,.T.);
#5901=EDGE_CURVE('',#4761,#4759,#804,.T.);
#5902=EDGE_CURVE('',#4760,#4762,#805,.T.);
#5903=EDGE_CURVE('',#4763,#4764,#2532,.T.);
#5904=EDGE_CURVE('',#4763,#4761,#806,.T.);
#5905=EDGE_CURVE('',#4762,#4764,#807,.T.);
#5906=EDGE_CURVE('',#4765,#4766,#2533,.T.);
#5907=EDGE_CURVE('',#4765,#4763,#808,.T.);
#5908=EDGE_CURVE('',#4764,#4766,#809,.T.);
#5909=EDGE_CURVE('',#4767,#4768,#2534,.T.);
#5910=EDGE_CURVE('',#4767,#4765,#810,.T.);
#5911=EDGE_CURVE('',#4766,#4768,#811,.T.);
#5912=EDGE_CURVE('',#4769,#4770,#2535,.T.);
#5913=EDGE_CURVE('',#4769,#4767,#812,.T.);
#5914=EDGE_CURVE('',#4768,#4770,#813,.T.);
#5915=EDGE_CURVE('',#4771,#4772,#2536,.T.);
#5916=EDGE_CURVE('',#4771,#4769,#814,.T.);
#5917=EDGE_CURVE('',#4770,#4772,#815,.T.);
#5918=EDGE_CURVE('',#4773,#4774,#2537,.T.);
#5919=EDGE_CURVE('',#4773,#4771,#816,.T.);
#5920=EDGE_CURVE('',#4772,#4774,#817,.T.);
#5921=EDGE_CURVE('',#4775,#4776,#2538,.T.);
#5922=EDGE_CURVE('',#4775,#4773,#818,.T.);
#5923=EDGE_CURVE('',#4774,#4776,#819,.T.);
#5924=EDGE_CURVE('',#4777,#4778,#2539,.T.);
#5925=EDGE_CURVE('',#4777,#4779,#820,.T.);
#5926=EDGE_CURVE('',#4779,#4780,#4313,.T.);
#5927=EDGE_CURVE('',#4780,#4778,#821,.T.);
#5928=EDGE_CURVE('',#4781,#4782,#2540,.T.);
#5929=EDGE_CURVE('',#4781,#4777,#822,.T.);
#5930=EDGE_CURVE('',#4778,#4782,#823,.T.);
#5931=EDGE_CURVE('',#4783,#4784,#2541,.T.);
#5932=EDGE_CURVE('',#4783,#4781,#824,.T.);
#5933=EDGE_CURVE('',#4782,#4784,#825,.T.);
#5934=EDGE_CURVE('',#4785,#4786,#2542,.T.);
#5935=EDGE_CURVE('',#4785,#4783,#826,.T.);
#5936=EDGE_CURVE('',#4784,#4786,#827,.T.);
#5937=EDGE_CURVE('',#4787,#4788,#2543,.T.);
#5938=EDGE_CURVE('',#4787,#4785,#828,.T.);
#5939=EDGE_CURVE('',#4786,#4788,#829,.T.);
#5940=EDGE_CURVE('',#4789,#4790,#2544,.T.);
#5941=EDGE_CURVE('',#4789,#4787,#830,.T.);
#5942=EDGE_CURVE('',#4788,#4790,#831,.T.);
#5943=EDGE_CURVE('',#4791,#4792,#2545,.T.);
#5944=EDGE_CURVE('',#4791,#4789,#832,.T.);
#5945=EDGE_CURVE('',#4790,#4792,#833,.T.);
#5946=EDGE_CURVE('',#4793,#4794,#2546,.T.);
#5947=EDGE_CURVE('',#4793,#4791,#834,.T.);
#5948=EDGE_CURVE('',#4792,#4794,#835,.T.);
#5949=EDGE_CURVE('',#4795,#4796,#2547,.T.);
#5950=EDGE_CURVE('',#4795,#4793,#836,.T.);
#5951=EDGE_CURVE('',#4794,#4796,#837,.T.);
#5952=EDGE_CURVE('',#4797,#4798,#2548,.T.);
#5953=EDGE_CURVE('',#4797,#4795,#838,.T.);
#5954=EDGE_CURVE('',#4796,#4798,#839,.T.);
#5955=EDGE_CURVE('',#4799,#4800,#2549,.T.);
#5956=EDGE_CURVE('',#4799,#4797,#840,.T.);
#5957=EDGE_CURVE('',#4798,#4800,#841,.T.);
#5958=EDGE_CURVE('',#4801,#4802,#2550,.T.);
#5959=EDGE_CURVE('',#4801,#4799,#842,.T.);
#5960=EDGE_CURVE('',#4800,#4802,#843,.T.);
#5961=EDGE_CURVE('',#4803,#4804,#2551,.T.);
#5962=EDGE_CURVE('',#4803,#4801,#844,.T.);
#5963=EDGE_CURVE('',#4802,#4804,#845,.T.);
#5964=EDGE_CURVE('',#4805,#4806,#2552,.T.);
#5965=EDGE_CURVE('',#4805,#4803,#846,.T.);
#5966=EDGE_CURVE('',#4804,#4806,#847,.T.);
#5967=EDGE_CURVE('',#4807,#4808,#2553,.T.);
#5968=EDGE_CURVE('',#4807,#4805,#848,.T.);
#5969=EDGE_CURVE('',#4806,#4808,#849,.T.);
#5970=EDGE_CURVE('',#4809,#4810,#2554,.T.);
#5971=EDGE_CURVE('',#4809,#4807,#850,.T.);
#5972=EDGE_CURVE('',#4808,#4810,#851,.T.);
#5973=EDGE_CURVE('',#4811,#4812,#2555,.T.);
#5974=EDGE_CURVE('',#4811,#4809,#852,.T.);
#5975=EDGE_CURVE('',#4810,#4812,#853,.T.);
#5976=EDGE_CURVE('',#4813,#4814,#2556,.T.);
#5977=EDGE_CURVE('',#4813,#4811,#854,.T.);
#5978=EDGE_CURVE('',#4812,#4814,#855,.T.);
#5979=EDGE_CURVE('',#4815,#4816,#2557,.T.);
#5980=EDGE_CURVE('',#4815,#4813,#856,.T.);
#5981=EDGE_CURVE('',#4814,#4816,#857,.T.);
#5982=EDGE_CURVE('',#4817,#4818,#2558,.T.);
#5983=EDGE_CURVE('',#4817,#4819,#858,.T.);
#5984=EDGE_CURVE('',#4819,#4818,#4314,.T.);
#5985=EDGE_CURVE('',#4820,#4821,#2559,.T.);
#5986=EDGE_CURVE('',#4820,#4817,#859,.T.);
#5987=EDGE_CURVE('',#4818,#4821,#860,.T.);
#5988=EDGE_CURVE('',#4822,#4823,#2560,.T.);
#5989=EDGE_CURVE('',#4822,#4820,#861,.T.);
#5990=EDGE_CURVE('',#4821,#4823,#862,.T.);
#5991=EDGE_CURVE('',#4824,#4825,#2561,.T.);
#5992=EDGE_CURVE('',#4824,#4822,#863,.T.);
#5993=EDGE_CURVE('',#4823,#4825,#864,.T.);
#5994=EDGE_CURVE('',#4826,#4827,#2562,.T.);
#5995=EDGE_CURVE('',#4826,#4824,#865,.T.);
#5996=EDGE_CURVE('',#4825,#4827,#866,.T.);
#5997=EDGE_CURVE('',#4828,#4829,#2563,.T.);
#5998=EDGE_CURVE('',#4828,#4826,#867,.T.);
#5999=EDGE_CURVE('',#4827,#4829,#868,.T.);
#6000=EDGE_CURVE('',#4830,#4831,#2564,.T.);
#6001=EDGE_CURVE('',#4830,#4828,#869,.T.);
#6002=EDGE_CURVE('',#4829,#4831,#870,.T.);
#6003=EDGE_CURVE('',#4832,#4833,#2565,.T.);
#6004=EDGE_CURVE('',#4832,#4830,#871,.T.);
#6005=EDGE_CURVE('',#4831,#4833,#872,.T.);
#6006=EDGE_CURVE('',#4834,#4835,#2566,.T.);
#6007=EDGE_CURVE('',#4834,#4832,#873,.T.);
#6008=EDGE_CURVE('',#4833,#4835,#874,.T.);
#6009=EDGE_CURVE('',#4836,#4837,#2567,.T.);
#6010=EDGE_CURVE('',#4836,#4834,#875,.T.);
#6011=EDGE_CURVE('',#4835,#4837,#876,.T.);
#6012=EDGE_CURVE('',#4838,#4839,#2568,.T.);
#6013=EDGE_CURVE('',#4838,#4836,#877,.T.);
#6014=EDGE_CURVE('',#4837,#4839,#878,.T.);
#6015=EDGE_CURVE('',#4840,#4841,#2569,.T.);
#6016=EDGE_CURVE('',#4840,#4838,#879,.T.);
#6017=EDGE_CURVE('',#4839,#4841,#880,.T.);
#6018=EDGE_CURVE('',#4842,#4843,#2570,.T.);
#6019=EDGE_CURVE('',#4842,#4840,#881,.T.);
#6020=EDGE_CURVE('',#4841,#4843,#882,.T.);
#6021=EDGE_CURVE('',#4844,#4845,#2571,.T.);
#6022=EDGE_CURVE('',#4844,#4842,#883,.T.);
#6023=EDGE_CURVE('',#4843,#4845,#884,.T.);
#6024=EDGE_CURVE('',#4846,#4847,#2572,.T.);
#6025=EDGE_CURVE('',#4846,#4844,#885,.T.);
#6026=EDGE_CURVE('',#4845,#4847,#886,.T.);
#6027=EDGE_CURVE('',#4848,#4849,#2573,.T.);
#6028=EDGE_CURVE('',#4848,#4846,#887,.T.);
#6029=EDGE_CURVE('',#4847,#4849,#888,.T.);
#6030=EDGE_CURVE('',#4850,#4851,#2574,.T.);
#6031=EDGE_CURVE('',#4850,#4848,#889,.T.);
#6032=EDGE_CURVE('',#4849,#4851,#890,.T.);
#6033=EDGE_CURVE('',#4852,#4853,#2575,.T.);
#6034=EDGE_CURVE('',#4852,#4850,#891,.T.);
#6035=EDGE_CURVE('',#4851,#4853,#892,.T.);
#6036=EDGE_CURVE('',#4854,#4855,#2576,.T.);
#6037=EDGE_CURVE('',#4854,#4852,#893,.T.);
#6038=EDGE_CURVE('',#4853,#4855,#894,.T.);
#6039=EDGE_CURVE('',#4856,#4857,#2577,.T.);
#6040=EDGE_CURVE('',#4856,#4858,#895,.T.);
#6041=EDGE_CURVE('',#4858,#4859,#4315,.T.);
#6042=EDGE_CURVE('',#4859,#4857,#896,.T.);
#6043=EDGE_CURVE('',#4860,#4861,#2578,.T.);
#6044=EDGE_CURVE('',#4860,#4856,#897,.T.);
#6045=EDGE_CURVE('',#4857,#4861,#898,.T.);
#6046=EDGE_CURVE('',#4862,#4863,#2579,.T.);
#6047=EDGE_CURVE('',#4862,#4860,#899,.T.);
#6048=EDGE_CURVE('',#4861,#4863,#900,.T.);
#6049=EDGE_CURVE('',#4864,#4865,#2580,.T.);
#6050=EDGE_CURVE('',#4864,#4862,#901,.T.);
#6051=EDGE_CURVE('',#4863,#4865,#902,.T.);
#6052=EDGE_CURVE('',#4866,#4867,#2581,.T.);
#6053=EDGE_CURVE('',#4866,#4864,#903,.T.);
#6054=EDGE_CURVE('',#4865,#4867,#904,.T.);
#6055=EDGE_CURVE('',#4868,#4869,#2582,.T.);
#6056=EDGE_CURVE('',#4868,#4866,#905,.T.);
#6057=EDGE_CURVE('',#4867,#4869,#906,.T.);
#6058=EDGE_CURVE('',#4870,#4871,#2583,.T.);
#6059=EDGE_CURVE('',#4870,#4868,#907,.T.);
#6060=EDGE_CURVE('',#4869,#4871,#908,.T.);
#6061=EDGE_CURVE('',#4872,#4873,#2584,.T.);
#6062=EDGE_CURVE('',#4872,#4870,#909,.T.);
#6063=EDGE_CURVE('',#4871,#4873,#910,.T.);
#6064=EDGE_CURVE('',#4874,#4875,#2585,.T.);
#6065=EDGE_CURVE('',#4874,#4872,#911,.T.);
#6066=EDGE_CURVE('',#4873,#4875,#912,.T.);
#6067=EDGE_CURVE('',#4876,#4877,#2586,.T.);
#6068=EDGE_CURVE('',#4876,#4874,#913,.T.);
#6069=EDGE_CURVE('',#4875,#4877,#914,.T.);
#6070=EDGE_CURVE('',#4878,#4879,#2587,.T.);
#6071=EDGE_CURVE('',#4878,#4876,#915,.T.);
#6072=EDGE_CURVE('',#4877,#4879,#916,.T.);
#6073=EDGE_CURVE('',#4880,#4881,#2588,.T.);
#6074=EDGE_CURVE('',#4880,#4878,#917,.T.);
#6075=EDGE_CURVE('',#4879,#4881,#918,.T.);
#6076=EDGE_CURVE('',#4882,#4883,#2589,.T.);
#6077=EDGE_CURVE('',#4882,#4880,#919,.T.);
#6078=EDGE_CURVE('',#4881,#4883,#920,.T.);
#6079=EDGE_CURVE('',#4884,#4885,#2590,.T.);
#6080=EDGE_CURVE('',#4884,#4882,#921,.T.);
#6081=EDGE_CURVE('',#4883,#4885,#922,.T.);
#6082=EDGE_CURVE('',#4886,#4887,#2591,.T.);
#6083=EDGE_CURVE('',#4886,#4884,#923,.T.);
#6084=EDGE_CURVE('',#4885,#4887,#924,.T.);
#6085=EDGE_CURVE('',#4888,#4889,#2592,.T.);
#6086=EDGE_CURVE('',#4888,#4886,#925,.T.);
#6087=EDGE_CURVE('',#4887,#4889,#926,.T.);
#6088=EDGE_CURVE('',#4890,#4891,#2593,.T.);
#6089=EDGE_CURVE('',#4890,#4888,#927,.T.);
#6090=EDGE_CURVE('',#4889,#4891,#928,.T.);
#6091=EDGE_CURVE('',#4892,#4893,#2594,.T.);
#6092=EDGE_CURVE('',#4892,#4890,#929,.T.);
#6093=EDGE_CURVE('',#4891,#4893,#930,.T.);
#6094=EDGE_CURVE('',#4894,#4895,#2595,.T.);
#6095=EDGE_CURVE('',#4896,#4895,#4316,.T.);
#6096=EDGE_CURVE('',#4896,#4894,#931,.T.);
#6097=EDGE_CURVE('',#4897,#4898,#2596,.T.);
#6098=EDGE_CURVE('',#4899,#4898,#932,.F.);
#6099=EDGE_CURVE('',#4895,#4899,#4317,.T.);
#6100=EDGE_CURVE('',#4894,#4897,#933,.T.);
#6101=EDGE_CURVE('',#4900,#4901,#2597,.T.);
#6102=EDGE_CURVE('',#4898,#4901,#934,.F.);
#6103=EDGE_CURVE('',#4897,#4900,#935,.T.);
#6104=EDGE_CURVE('',#4902,#4903,#2598,.T.);
#6105=EDGE_CURVE('',#4901,#4903,#936,.F.);
#6106=EDGE_CURVE('',#4900,#4902,#937,.T.);
#6107=EDGE_CURVE('',#4904,#4905,#2599,.T.);
#6108=EDGE_CURVE('',#4903,#4905,#938,.F.);
#6109=EDGE_CURVE('',#4902,#4904,#939,.T.);
#6110=EDGE_CURVE('',#4906,#4907,#2600,.T.);
#6111=EDGE_CURVE('',#4905,#4907,#940,.F.);
#6112=EDGE_CURVE('',#4904,#4906,#941,.T.);
#6113=EDGE_CURVE('',#4908,#4909,#2601,.T.);
#6114=EDGE_CURVE('',#4908,#4910,#942,.T.);
#6115=EDGE_CURVE('',#4911,#4910,#2602,.T.);
#6116=EDGE_CURVE('',#4909,#4911,#943,.F.);
#6117=EDGE_CURVE('',#4912,#4913,#2603,.T.);
#6118=EDGE_CURVE('',#4914,#4913,#4318,.T.);
#6119=EDGE_CURVE('',#4914,#4912,#944,.T.);
#6120=EDGE_CURVE('',#4915,#4916,#2604,.T.);
#6121=EDGE_CURVE('',#4917,#4916,#945,.F.);
#6122=EDGE_CURVE('',#4913,#4917,#4319,.T.);
#6123=EDGE_CURVE('',#4912,#4915,#946,.T.);
#6124=EDGE_CURVE('',#4918,#4919,#2605,.T.);
#6125=EDGE_CURVE('',#4916,#4919,#947,.F.);
#6126=EDGE_CURVE('',#4915,#4918,#948,.T.);
#6127=EDGE_CURVE('',#4920,#4921,#2606,.T.);
#6128=EDGE_CURVE('',#4919,#4921,#949,.F.);
#6129=EDGE_CURVE('',#4918,#4920,#950,.T.);
#6130=EDGE_CURVE('',#4922,#4923,#2607,.T.);
#6131=EDGE_CURVE('',#4921,#4923,#951,.F.);
#6132=EDGE_CURVE('',#4920,#4922,#952,.T.);
#6133=EDGE_CURVE('',#4924,#4925,#2608,.T.);
#6134=EDGE_CURVE('',#4923,#4925,#953,.F.);
#6135=EDGE_CURVE('',#4922,#4924,#954,.T.);
#6136=EDGE_CURVE('',#4926,#4927,#2609,.T.);
#6137=EDGE_CURVE('',#4926,#4928,#955,.T.);
#6138=EDGE_CURVE('',#4929,#4928,#2610,.T.);
#6139=EDGE_CURVE('',#4927,#4929,#956,.F.);
#6140=EDGE_CURVE('',#4930,#4931,#2611,.T.);
#6141=EDGE_CURVE('',#4932,#4931,#4320,.T.);
#6142=EDGE_CURVE('',#4932,#4930,#957,.T.);
#6143=EDGE_CURVE('',#4933,#4934,#2612,.T.);
#6144=EDGE_CURVE('',#4935,#4934,#958,.F.);
#6145=EDGE_CURVE('',#4931,#4935,#4321,.T.);
#6146=EDGE_CURVE('',#4930,#4933,#959,.T.);
#6147=EDGE_CURVE('',#4936,#4937,#2613,.T.);
#6148=EDGE_CURVE('',#4934,#4937,#960,.F.);
#6149=EDGE_CURVE('',#4933,#4936,#961,.T.);
#6150=EDGE_CURVE('',#4938,#4939,#2614,.T.);
#6151=EDGE_CURVE('',#4937,#4939,#962,.F.);
#6152=EDGE_CURVE('',#4936,#4938,#963,.T.);
#6153=EDGE_CURVE('',#4940,#4941,#2615,.T.);
#6154=EDGE_CURVE('',#4939,#4941,#964,.F.);
#6155=EDGE_CURVE('',#4938,#4940,#965,.T.);
#6156=EDGE_CURVE('',#4942,#4943,#2616,.T.);
#6157=EDGE_CURVE('',#4941,#4943,#966,.F.);
#6158=EDGE_CURVE('',#4940,#4942,#967,.T.);
#6159=EDGE_CURVE('',#4944,#4945,#2617,.T.);
#6160=EDGE_CURVE('',#4944,#4946,#968,.T.);
#6161=EDGE_CURVE('',#4947,#4946,#2618,.T.);
#6162=EDGE_CURVE('',#4945,#4947,#969,.F.);
#6163=EDGE_CURVE('',#4948,#4949,#2619,.T.);
#6164=EDGE_CURVE('',#4950,#4949,#4322,.T.);
#6165=EDGE_CURVE('',#4950,#4948,#970,.T.);
#6166=EDGE_CURVE('',#4951,#4952,#2620,.T.);
#6167=EDGE_CURVE('',#4953,#4952,#971,.F.);
#6168=EDGE_CURVE('',#4949,#4953,#4323,.T.);
#6169=EDGE_CURVE('',#4948,#4951,#972,.T.);
#6170=EDGE_CURVE('',#4954,#4955,#2621,.T.);
#6171=EDGE_CURVE('',#4952,#4955,#973,.F.);
#6172=EDGE_CURVE('',#4951,#4954,#974,.T.);
#6173=EDGE_CURVE('',#4956,#4957,#2622,.T.);
#6174=EDGE_CURVE('',#4955,#4957,#975,.F.);
#6175=EDGE_CURVE('',#4954,#4956,#976,.T.);
#6176=EDGE_CURVE('',#4958,#4959,#2623,.T.);
#6177=EDGE_CURVE('',#4957,#4959,#977,.F.);
#6178=EDGE_CURVE('',#4956,#4958,#978,.T.);
#6179=EDGE_CURVE('',#4960,#4961,#2624,.T.);
#6180=EDGE_CURVE('',#4959,#4961,#979,.F.);
#6181=EDGE_CURVE('',#4958,#4960,#980,.T.);
#6182=EDGE_CURVE('',#4962,#4963,#2625,.T.);
#6183=EDGE_CURVE('',#4962,#4964,#981,.T.);
#6184=EDGE_CURVE('',#4965,#4964,#2626,.T.);
#6185=EDGE_CURVE('',#4963,#4965,#982,.F.);
#6186=EDGE_CURVE('',#4961,#4963,#983,.F.);
#6187=EDGE_CURVE('',#4960,#4962,#984,.T.);
#6188=EDGE_CURVE('',#4943,#4945,#985,.F.);
#6189=EDGE_CURVE('',#4942,#4944,#986,.T.);
#6190=EDGE_CURVE('',#4925,#4927,#987,.F.);
#6191=EDGE_CURVE('',#4924,#4926,#988,.T.);
#6192=EDGE_CURVE('',#4907,#4909,#989,.F.);
#6193=EDGE_CURVE('',#4906,#4908,#990,.T.);
#6194=EDGE_CURVE('',#4893,#4966,#991,.T.);
#6195=EDGE_CURVE('',#4967,#4966,#4324,.T.);
#6196=EDGE_CURVE('',#4967,#4892,#992,.T.);
#6197=EDGE_CURVE('',#4855,#4968,#993,.T.);
#6198=EDGE_CURVE('',#4969,#4968,#4325,.T.);
#6199=EDGE_CURVE('',#4969,#4854,#994,.T.);
#6200=EDGE_CURVE('',#4816,#4970,#995,.T.);
#6201=EDGE_CURVE('',#4971,#4970,#4326,.T.);
#6202=EDGE_CURVE('',#4971,#4815,#996,.T.);
#6203=EDGE_CURVE('',#4776,#4972,#997,.T.);
#6204=EDGE_CURVE('',#4973,#4972,#4327,.T.);
#6205=EDGE_CURVE('',#4973,#4775,#998,.T.);
#6206=EDGE_CURVE('',#4974,#4974,#4328,.T.);
#6207=EDGE_CURVE('',#4974,#4975,#2627,.T.);
#6208=EDGE_CURVE('',#4975,#4975,#4329,.T.);
#6209=EDGE_CURVE('',#4976,#4976,#4330,.T.);
#6210=EDGE_CURVE('',#4976,#4977,#2628,.T.);
#6211=EDGE_CURVE('',#4977,#4977,#4331,.T.);
#6212=EDGE_CURVE('',#4978,#4978,#4332,.T.);
#6213=EDGE_CURVE('',#4978,#4979,#2629,.T.);
#6214=EDGE_CURVE('',#4979,#4979,#4333,.T.);
#6215=EDGE_CURVE('',#4979,#4980,#2630,.T.);
#6216=EDGE_CURVE('',#4980,#4980,#4334,.T.);
#6217=EDGE_CURVE('',#4740,#4981,#999,.T.);
#6218=EDGE_CURVE('',#4982,#4739,#1000,.T.);
#6219=EDGE_CURVE('',#4983,#4982,#4335,.T.);
#6220=EDGE_CURVE('',#4981,#4983,#1001,.T.);
#6221=EDGE_CURVE('',#4981,#4984,#2631,.T.);
#6222=EDGE_CURVE('',#4984,#4984,#4336,.T.);
#6223=EDGE_CURVE('',#4780,#4985,#1002,.T.);
#6224=EDGE_CURVE('',#4986,#4779,#1003,.T.);
#6225=EDGE_CURVE('',#4987,#4986,#4337,.T.);
#6226=EDGE_CURVE('',#4985,#4987,#1004,.T.);
#6227=EDGE_CURVE('',#4985,#4988,#2632,.T.);
#6228=EDGE_CURVE('',#4988,#4988,#4338,.T.);
#6229=EDGE_CURVE('',#4818,#4989,#1005,.T.);
#6230=EDGE_CURVE('',#4990,#4819,#1006,.T.);
#6231=EDGE_CURVE('',#4991,#4990,#4339,.T.);
#6232=EDGE_CURVE('',#4989,#4991,#1007,.T.);
#6233=EDGE_CURVE('',#4989,#4992,#2633,.T.);
#6234=EDGE_CURVE('',#4992,#4992,#4340,.T.);
#6235=EDGE_CURVE('',#4859,#4993,#1008,.T.);
#6236=EDGE_CURVE('',#4994,#4858,#1009,.T.);
#6237=EDGE_CURVE('',#4995,#4994,#4341,.T.);
#6238=EDGE_CURVE('',#4993,#4995,#1010,.T.);
#6239=EDGE_CURVE('',#4993,#4996,#2634,.T.);
#6240=EDGE_CURVE('',#4996,#4996,#4342,.T.);
#6241=EDGE_CURVE('',#4966,#4896,#4343,.T.);
#6242=EDGE_CURVE('',#4995,#4997,#265,.T.);
#6243=EDGE_CURVE('',#4910,#4997,#2635,.T.);
#6244=EDGE_CURVE('',#4899,#4967,#4344,.T.);
#6245=EDGE_CURVE('',#4998,#4911,#2636,.T.);
#6246=EDGE_CURVE('',#4994,#4998,#266,.T.);
#6247=EDGE_CURVE('',#4997,#4998,#2637,.T.);
#6248=EDGE_CURVE('',#4999,#5000,#2638,.T.);
#6249=EDGE_CURVE('',#5001,#4999,#2639,.T.);
#6250=EDGE_CURVE('',#5002,#5001,#2640,.T.);
#6251=EDGE_CURVE('',#5003,#5002,#2641,.T.);
#6252=EDGE_CURVE('',#5003,#5004,#2642,.T.);
#6253=EDGE_CURVE('',#5005,#5004,#2643,.T.);
#6254=EDGE_CURVE('',#5006,#5005,#2644,.T.);
#6255=EDGE_CURVE('',#5000,#5006,#2645,.T.);
#6256=EDGE_CURVE('',#4972,#4950,#4345,.T.);
#6257=EDGE_CURVE('',#4953,#4973,#4346,.T.);
#6258=EDGE_CURVE('',#4970,#4932,#4347,.T.);
#6259=EDGE_CURVE('',#4935,#4971,#4348,.T.);
#6260=EDGE_CURVE('',#4968,#4914,#4349,.T.);
#6261=EDGE_CURVE('',#4917,#4969,#4350,.T.);
#6262=EDGE_CURVE('',#4991,#5007,#267,.T.);
#6263=EDGE_CURVE('',#4928,#5007,#2646,.T.);
#6264=EDGE_CURVE('',#5008,#4929,#2647,.T.);
#6265=EDGE_CURVE('',#4990,#5008,#268,.T.);
#6266=EDGE_CURVE('',#5007,#5008,#2648,.T.);
#6267=EDGE_CURVE('',#4987,#5009,#269,.T.);
#6268=EDGE_CURVE('',#4946,#5009,#2649,.T.);
#6269=EDGE_CURVE('',#5010,#4947,#2650,.T.);
#6270=EDGE_CURVE('',#4986,#5010,#270,.T.);
#6271=EDGE_CURVE('',#5009,#5010,#2651,.T.);
#6272=EDGE_CURVE('',#4983,#5011,#271,.T.);
#6273=EDGE_CURVE('',#4964,#5011,#2652,.T.);
#6274=EDGE_CURVE('',#5012,#4965,#2653,.T.);
#6275=EDGE_CURVE('',#4982,#5012,#272,.T.);
#6276=EDGE_CURVE('',#5011,#5012,#2654,.T.);
#6277=EDGE_CURVE('',#5013,#5006,#2655,.T.);
#6278=EDGE_CURVE('',#5013,#5014,#2656,.T.);
#6279=EDGE_CURVE('',#5014,#5000,#2657,.T.);
#6280=EDGE_CURVE('',#5015,#5005,#2658,.T.);
#6281=EDGE_CURVE('',#5015,#5013,#2659,.T.);
#6282=EDGE_CURVE('',#5013,#5016,#746,.T.);
#6283=EDGE_CURVE('',#5017,#5016,#2660,.T.);
#6284=EDGE_CURVE('',#5014,#5017,#747,.T.);
#6285=EDGE_CURVE('',#5014,#5018,#2661,.T.);
#6286=EDGE_CURVE('',#5018,#4999,#2662,.T.);
#6287=EDGE_CURVE('',#5019,#5004,#2663,.T.);
#6288=EDGE_CURVE('',#5019,#5015,#2664,.T.);
#6289=EDGE_CURVE('',#5015,#5020,#748,.T.);
#6290=EDGE_CURVE('',#5016,#5020,#2665,.T.);
#6291=EDGE_CURVE('',#5021,#5003,#2666,.T.);
#6292=EDGE_CURVE('',#5021,#5019,#2667,.T.);
#6293=EDGE_CURVE('',#5022,#5019,#749,.T.);
#6294=EDGE_CURVE('',#5020,#5022,#2668,.T.);
#6295=EDGE_CURVE('',#5023,#5002,#2669,.T.);
#6296=EDGE_CURVE('',#5023,#5021,#2670,.T.);
#6297=EDGE_CURVE('',#5024,#5021,#750,.T.);
#6298=EDGE_CURVE('',#5022,#5024,#2671,.T.);
#6299=EDGE_CURVE('',#5025,#5001,#2672,.T.);
#6300=EDGE_CURVE('',#5025,#5023,#2673,.T.);
#6301=EDGE_CURVE('',#5026,#5023,#751,.T.);
#6302=EDGE_CURVE('',#5024,#5026,#2674,.T.);
#6303=EDGE_CURVE('',#5018,#5025,#2675,.T.);
#6304=EDGE_CURVE('',#5027,#5025,#752,.T.);
#6305=EDGE_CURVE('',#5026,#5027,#2676,.T.);
#6306=EDGE_CURVE('',#5018,#5028,#753,.T.);
#6307=EDGE_CURVE('',#5027,#5028,#2677,.T.);
#6308=EDGE_CURVE('',#5028,#5017,#2678,.T.);
#6309=EDGE_CURVE('',#5029,#5030,#2679,.T.);
#6310=EDGE_CURVE('',#5031,#5029,#4351,.T.);
#6311=EDGE_CURVE('',#5032,#5031,#273,.T.);
#6312=EDGE_CURVE('',#5030,#5032,#4352,.T.);
#6313=EDGE_CURVE('',#5032,#5030,#4353,.T.);
#6314=EDGE_CURVE('',#5033,#5032,#274,.T.);
#6315=EDGE_CURVE('',#5029,#5033,#4354,.T.);
#6316=EDGE_CURVE('',#5034,#5035,#2680,.T.);
#6317=EDGE_CURVE('',#5035,#5035,#4355,.T.);
#6318=EDGE_CURVE('',#5036,#5036,#4356,.T.);
#6319=EDGE_CURVE('',#5036,#5029,#2681,.T.);
#6320=EDGE_CURVE('',#5033,#5037,#2682,.T.);
#6321=EDGE_CURVE('',#5037,#5038,#4357,.T.);
#6322=EDGE_CURVE('',#5038,#5031,#2683,.T.);
#6323=EDGE_CURVE('',#5037,#5038,#2684,.T.);
#6324=EDGE_CURVE('',#5039,#5039,#4358,.T.);
#6325=EDGE_CURVE('',#5039,#5040,#2685,.T.);
#6326=EDGE_CURVE('',#5040,#5040,#4359,.T.);
#6327=EDGE_CURVE('',#5041,#5041,#4360,.T.);
#6328=EDGE_CURVE('',#5041,#5042,#2686,.T.);
#6329=EDGE_CURVE('',#5042,#5042,#4361,.T.);
#6330=EDGE_CURVE('',#5043,#5043,#4362,.T.);
#6331=EDGE_CURVE('',#5043,#5044,#2687,.T.);
#6332=EDGE_CURVE('',#5044,#5044,#4363,.T.);
#6333=EDGE_CURVE('',#5045,#5045,#4364,.T.);
#6334=EDGE_CURVE('',#5045,#5046,#2688,.T.);
#6335=EDGE_CURVE('',#5046,#5046,#4365,.T.);
#6336=EDGE_CURVE('',#5047,#5047,#4366,.T.);
#6337=EDGE_CURVE('',#5047,#5048,#2689,.T.);
#6338=EDGE_CURVE('',#5048,#5048,#4367,.T.);
#6339=EDGE_CURVE('',#5049,#5049,#4368,.T.);
#6340=EDGE_CURVE('',#5049,#5041,#2690,.T.);
#6341=EDGE_CURVE('',#5050,#5050,#4369,.T.);
#6342=EDGE_CURVE('',#5050,#5043,#2691,.T.);
#6343=EDGE_CURVE('',#5051,#5051,#4370,.T.);
#6344=EDGE_CURVE('',#5051,#5045,#2692,.T.);
#6345=EDGE_CURVE('',#5052,#5052,#4371,.T.);
#6346=EDGE_CURVE('',#5052,#5047,#2693,.T.);
#6347=EDGE_CURVE('',#5053,#5053,#4372,.T.);
#6348=EDGE_CURVE('',#5053,#5054,#2694,.T.);
#6349=EDGE_CURVE('',#5054,#5054,#4373,.T.);
#6350=EDGE_CURVE('',#5055,#5056,#2695,.T.);
#6351=EDGE_CURVE('',#5056,#5057,#2696,.T.);
#6352=EDGE_CURVE('',#5057,#5058,#2697,.T.);
#6353=EDGE_CURVE('',#5058,#5055,#2698,.T.);
#6354=EDGE_CURVE('',#5059,#5060,#2699,.T.);
#6355=EDGE_CURVE('',#5058,#5060,#2700,.T.);
#6356=EDGE_CURVE('',#5057,#5059,#2701,.T.);
#6357=EDGE_CURVE('',#5060,#5061,#2702,.T.);
#6358=EDGE_CURVE('',#5055,#5061,#2703,.T.);
#6359=EDGE_CURVE('',#5061,#5062,#2704,.T.);
#6360=EDGE_CURVE('',#5056,#5062,#2705,.T.);
#6361=EDGE_CURVE('',#5062,#5059,#2706,.T.);
#6362=EDGE_CURVE('',#5063,#5064,#2707,.T.);
#6363=EDGE_CURVE('',#5064,#5065,#2708,.T.);
#6364=EDGE_CURVE('',#5065,#5066,#2709,.T.);
#6365=EDGE_CURVE('',#5066,#5063,#2710,.T.);
#6366=EDGE_CURVE('',#5064,#5067,#2711,.T.);
#6367=EDGE_CURVE('',#5067,#5068,#2712,.T.);
#6368=EDGE_CURVE('',#5065,#5068,#2713,.T.);
#6369=EDGE_CURVE('',#5069,#5070,#2714,.T.);
#6370=EDGE_CURVE('',#5070,#5071,#2715,.T.);
#6371=EDGE_CURVE('',#5071,#5072,#2716,.T.);
#6372=EDGE_CURVE('',#5072,#5073,#2717,.T.);
#6373=EDGE_CURVE('',#5073,#5074,#2718,.T.);
#6374=EDGE_CURVE('',#5074,#5075,#2719,.T.);
#6375=EDGE_CURVE('',#5075,#5076,#2720,.T.);
#6376=EDGE_CURVE('',#5076,#5069,#2721,.T.);
#6377=EDGE_CURVE('',#5077,#5073,#754,.T.);
#6378=EDGE_CURVE('',#5078,#5072,#755,.T.);
#6379=EDGE_CURVE('',#5077,#5078,#2722,.T.);
#6380=EDGE_CURVE('',#5079,#5071,#756,.T.);
#6381=EDGE_CURVE('',#5078,#5079,#2723,.T.);
#6382=EDGE_CURVE('',#5070,#5080,#757,.T.);
#6383=EDGE_CURVE('',#5079,#5080,#2724,.T.);
#6384=EDGE_CURVE('',#5081,#5078,#2725,.T.);
#6385=EDGE_CURVE('',#5082,#5079,#2726,.T.);
#6386=EDGE_CURVE('',#5081,#5082,#2727,.T.);
#6387=EDGE_CURVE('',#5069,#5083,#758,.T.);
#6388=EDGE_CURVE('',#5080,#5083,#2728,.T.);
#6389=EDGE_CURVE('',#5084,#5080,#2729,.T.);
#6390=EDGE_CURVE('',#5082,#5084,#2730,.T.);
#6391=EDGE_CURVE('',#5076,#5085,#759,.T.);
#6392=EDGE_CURVE('',#5083,#5085,#2731,.T.);
#6393=EDGE_CURVE('',#5086,#5083,#2732,.T.);
#6394=EDGE_CURVE('',#5086,#5084,#2733,.T.);
#6395=EDGE_CURVE('',#5075,#5087,#760,.T.);
#6396=EDGE_CURVE('',#5085,#5087,#2734,.T.);
#6397=EDGE_CURVE('',#5088,#5085,#2735,.T.);
#6398=EDGE_CURVE('',#5086,#5088,#2736,.T.);
#6399=EDGE_CURVE('',#5089,#5074,#761,.T.);
#6400=EDGE_CURVE('',#5087,#5089,#2737,.T.);
#6401=EDGE_CURVE('',#5090,#5087,#2738,.T.);
#6402=EDGE_CURVE('',#5088,#5090,#2739,.T.);
#6403=EDGE_CURVE('',#5091,#5077,#2740,.T.);
#6404=EDGE_CURVE('',#5091,#5081,#2741,.T.);
#6405=EDGE_CURVE('',#5068,#5092,#4374,.T.);
#6406=EDGE_CURVE('',#5092,#5093,#2742,.T.);
#6407=EDGE_CURVE('',#5066,#5093,#2743,.T.);
#6408=EDGE_CURVE('',#5093,#5094,#2744,.T.);
#6409=EDGE_CURVE('',#5063,#5094,#2745,.T.);
#6410=EDGE_CURVE('',#5094,#5095,#2746,.T.);
#6411=EDGE_CURVE('',#5095,#5067,#4375,.T.);
#6412=EDGE_CURVE('',#5092,#5077,#2747,.T.);
#6413=EDGE_CURVE('',#5089,#5095,#2748,.T.);
#6414=EDGE_CURVE('',#5096,#5089,#2749,.T.);
#6415=EDGE_CURVE('',#5090,#5096,#2750,.T.);
#6416=EDGE_CURVE('',#5096,#5091,#2751,.T.);
#6417=EDGE_CURVE('',#5097,#5097,#4376,.T.);
#6418=EDGE_CURVE('',#5097,#5098,#2752,.T.);
#6419=EDGE_CURVE('',#5098,#5098,#4377,.T.);
#6420=EDGE_CURVE('',#5099,#5099,#4378,.T.);
#6421=EDGE_CURVE('',#5099,#5100,#2753,.T.);
#6422=EDGE_CURVE('',#5100,#5100,#4379,.T.);
#6423=EDGE_CURVE('',#5101,#5101,#4380,.T.);
#6424=EDGE_CURVE('',#5101,#5102,#2754,.T.);
#6425=EDGE_CURVE('',#5102,#5102,#4381,.T.);
#6426=EDGE_CURVE('',#5103,#5103,#4382,.T.);
#6427=EDGE_CURVE('',#5103,#5104,#2755,.T.);
#6428=EDGE_CURVE('',#5104,#5104,#4383,.T.);
#6429=EDGE_CURVE('',#5105,#5105,#4384,.T.);
#6430=EDGE_CURVE('',#5105,#5106,#2756,.T.);
#6431=EDGE_CURVE('',#5106,#5106,#4385,.T.);
#6432=EDGE_CURVE('',#5107,#5108,#2757,.T.);
#6433=EDGE_CURVE('',#5108,#5109,#2758,.T.);
#6434=EDGE_CURVE('',#5110,#5109,#2759,.T.);
#6435=EDGE_CURVE('',#5111,#5110,#2760,.T.);
#6436=EDGE_CURVE('',#5112,#5111,#2761,.T.);
#6437=EDGE_CURVE('',#5112,#5113,#2762,.T.);
#6438=EDGE_CURVE('',#5113,#5114,#2763,.T.);
#6439=EDGE_CURVE('',#5114,#5107,#2764,.T.);
#6440=EDGE_CURVE('',#5115,#5116,#2765,.T.);
#6441=EDGE_CURVE('',#5117,#5115,#2766,.T.);
#6442=EDGE_CURVE('',#5118,#5117,#2767,.T.);
#6443=EDGE_CURVE('',#5119,#5118,#2768,.T.);
#6444=EDGE_CURVE('',#5119,#5120,#2769,.T.);
#6445=EDGE_CURVE('',#5120,#5121,#2770,.T.);
#6446=EDGE_CURVE('',#5121,#5122,#2771,.T.);
#6447=EDGE_CURVE('',#5116,#5122,#2772,.T.);
#6448=EDGE_CURVE('',#5107,#5115,#2773,.T.);
#6449=EDGE_CURVE('',#5114,#5117,#2774,.T.);
#6450=EDGE_CURVE('',#5108,#5116,#2775,.T.);
#6451=EDGE_CURVE('',#5113,#5118,#2776,.T.);
#6452=EDGE_CURVE('',#5110,#5121,#2777,.T.);
#6453=EDGE_CURVE('',#5109,#5122,#2778,.T.);
#6454=EDGE_CURVE('',#5112,#5119,#2779,.T.);
#6455=EDGE_CURVE('',#5111,#5120,#2780,.T.);
#6456=EDGE_CURVE('',#5123,#5123,#4386,.T.);
#6457=EDGE_CURVE('',#5123,#5124,#2781,.T.);
#6458=EDGE_CURVE('',#5124,#5124,#4387,.T.);
#6459=EDGE_CURVE('',#5125,#5125,#4388,.T.);
#6460=EDGE_CURVE('',#5125,#5123,#2782,.T.);
#6461=EDGE_CURVE('',#5126,#5126,#4389,.T.);
#6462=EDGE_CURVE('',#5125,#5127,#2783,.T.);
#6463=EDGE_CURVE('',#5127,#5127,#4390,.T.);
#6464=EDGE_CURVE('',#5128,#5128,#4391,.T.);
#6465=EDGE_CURVE('',#5126,#5128,#2784,.T.);
#6466=EDGE_CURVE('',#5129,#5129,#4392,.T.);
#6467=EDGE_CURVE('',#5129,#5130,#2785,.T.);
#6468=EDGE_CURVE('',#5130,#5130,#4393,.T.);
#6469=EDGE_CURVE('',#5131,#5131,#4394,.T.);
#6470=EDGE_CURVE('',#5131,#5132,#2786,.T.);
#6471=EDGE_CURVE('',#5132,#5132,#4395,.T.);
#6472=EDGE_CURVE('',#5133,#5133,#4396,.T.);
#6473=EDGE_CURVE('',#5133,#5134,#2787,.T.);
#6474=EDGE_CURVE('',#5134,#5134,#4397,.T.);
#6475=EDGE_CURVE('',#5135,#5135,#4398,.T.);
#6476=EDGE_CURVE('',#5135,#5136,#2788,.T.);
#6477=EDGE_CURVE('',#5136,#5136,#4399,.T.);
#6478=EDGE_CURVE('',#5137,#5138,#2789,.T.);
#6479=EDGE_CURVE('',#5139,#5137,#275,.T.);
#6480=EDGE_CURVE('',#5140,#5139,#2790,.T.);
#6481=EDGE_CURVE('',#5138,#5140,#276,.T.);
#6482=EDGE_CURVE('',#5141,#5139,#277,.T.);
#6483=EDGE_CURVE('',#5141,#5142,#2791,.T.);
#6484=EDGE_CURVE('',#5140,#5142,#278,.T.);
#6485=EDGE_CURVE('',#5143,#5144,#279,.F.);
#6486=EDGE_CURVE('',#5144,#5145,#2792,.T.);
#6487=EDGE_CURVE('',#5145,#5145,#4400,.T.);
#6488=EDGE_CURVE('',#5144,#5146,#280,.F.);
#6489=EDGE_CURVE('',#5146,#5147,#281,.T.);
#6490=EDGE_CURVE('',#5147,#5141,#282,.T.);
#6491=EDGE_CURVE('',#5137,#5143,#283,.T.);
#6492=EDGE_CURVE('',#5148,#5138,#284,.T.);
#6493=EDGE_CURVE('',#5143,#5148,#2793,.T.);
#6494=EDGE_CURVE('',#5149,#5148,#285,.F.);
#6495=EDGE_CURVE('',#5150,#5149,#286,.F.);
#6496=EDGE_CURVE('',#5146,#5150,#2794,.T.);
#6497=EDGE_CURVE('',#5151,#5150,#287,.T.);
#6498=EDGE_CURVE('',#5147,#5151,#2795,.T.);
#6499=EDGE_CURVE('',#5142,#5151,#288,.T.);
#6500=EDGE_CURVE('',#5152,#5152,#4401,.T.);
#6501=EDGE_CURVE('',#5149,#5152,#2796,.T.);
#6502=EDGE_CURVE('',#5135,#5133,#2797,.T.);
#6503=EDGE_CURVE('',#5153,#5153,#4402,.T.);
#6504=EDGE_CURVE('',#5153,#5154,#2798,.T.);
#6505=EDGE_CURVE('',#5154,#5154,#4403,.T.);
#6506=EDGE_CURVE('',#5155,#5155,#4404,.T.);
#6507=EDGE_CURVE('',#5155,#5153,#4405,.T.);
#6508=EDGE_CURVE('',#5156,#5156,#4406,.T.);
#6509=EDGE_CURVE('',#5156,#5155,#2799,.T.);
#6510=EDGE_CURVE('',#5157,#5157,#4407,.T.);
#6511=EDGE_CURVE('',#5157,#5158,#2800,.T.);
#6512=EDGE_CURVE('',#5158,#5158,#4408,.T.);
#6513=EDGE_CURVE('',#5159,#5160,#4409,.T.);
#6514=EDGE_CURVE('',#5160,#5159,#4410,.T.);
#6515=EDGE_CURVE('',#5160,#5157,#2801,.T.);
#6516=EDGE_CURVE('',#5159,#5161,#2802,.T.);
#6517=EDGE_CURVE('',#5161,#5161,#4411,.T.);
#6518=EDGE_CURVE('',#5162,#5162,#4412,.T.);
#6519=EDGE_CURVE('',#5162,#5163,#2803,.T.);
#6520=EDGE_CURVE('',#5163,#5163,#4413,.T.);
#6521=EDGE_CURVE('',#5163,#5164,#4414,.T.);
#6522=EDGE_CURVE('',#5164,#5164,#4415,.T.);
#6523=EDGE_CURVE('',#5165,#5165,#4416,.T.);
#6524=EDGE_CURVE('',#5165,#5166,#2804,.T.);
#6525=EDGE_CURVE('',#5166,#5166,#4417,.T.);
#6526=EDGE_CURVE('',#5166,#5167,#2805,.T.);
#6527=EDGE_CURVE('',#5167,#5167,#4418,.T.);
#6528=EDGE_CURVE('',#5168,#5168,#4419,.T.);
#6529=EDGE_CURVE('',#5168,#5169,#2806,.T.);
#6530=EDGE_CURVE('',#5169,#5169,#4420,.T.);
#6531=EDGE_CURVE('',#5170,#5171,#4421,.T.);
#6532=EDGE_CURVE('',#5171,#5170,#4422,.T.);
#6533=EDGE_CURVE('',#5171,#5168,#2807,.T.);
#6534=EDGE_CURVE('',#5170,#5172,#2808,.T.);
#6535=EDGE_CURVE('',#5172,#5172,#4423,.T.);
#6536=EDGE_CURVE('',#5173,#5173,#4424,.T.);
#6537=EDGE_CURVE('',#5173,#5174,#2809,.T.);
#6538=EDGE_CURVE('',#5174,#5174,#4425,.T.);
#6539=EDGE_CURVE('',#5175,#5175,#4426,.T.);
#6540=EDGE_CURVE('',#5175,#5173,#4427,.T.);
#6541=EDGE_CURVE('',#5176,#5176,#4428,.T.);
#6542=EDGE_CURVE('',#5176,#5177,#2810,.T.);
#6543=EDGE_CURVE('',#5177,#5177,#4429,.T.);
#6544=EDGE_CURVE('',#5178,#5178,#4430,.T.);
#6545=EDGE_CURVE('',#5178,#5176,#2811,.T.);
#6546=EDGE_CURVE('',#5179,#5180,#4431,.T.);
#6547=EDGE_CURVE('',#5181,#5182,#4432,.T.);
#6548=EDGE_CURVE('',#5183,#5184,#4433,.T.);
#6549=EDGE_CURVE('',#5185,#5186,#4434,.T.);
#6550=EDGE_CURVE('',#5187,#5188,#4435,.T.);
#6551=EDGE_CURVE('',#5189,#5190,#4436,.T.);
#6552=EDGE_CURVE('',#5191,#5192,#4437,.T.);
#6553=EDGE_CURVE('',#5193,#5194,#4438,.T.);
#6554=EDGE_CURVE('',#5195,#5196,#4439,.T.);
#6555=EDGE_CURVE('',#5197,#5198,#4440,.T.);
#6556=EDGE_CURVE('',#5199,#5200,#2812,.T.);
#6557=EDGE_CURVE('',#5200,#5201,#2813,.T.);
#6558=EDGE_CURVE('',#5201,#5202,#2814,.T.);
#6559=EDGE_CURVE('',#5199,#5202,#2815,.T.);
#6560=EDGE_CURVE('',#5203,#5204,#2816,.T.);
#6561=EDGE_CURVE('',#5204,#5205,#2817,.T.);
#6562=EDGE_CURVE('',#5205,#5206,#2818,.T.);
#6563=EDGE_CURVE('',#5203,#5206,#2819,.T.);
#6564=EDGE_CURVE('',#5207,#5208,#2820,.T.);
#6565=EDGE_CURVE('',#5209,#5207,#2821,.T.);
#6566=EDGE_CURVE('',#5209,#5210,#2822,.T.);
#6567=EDGE_CURVE('',#5210,#5208,#2823,.F.);
#6568=EDGE_CURVE('',#5211,#5212,#2824,.T.);
#6569=EDGE_CURVE('',#5212,#5213,#2825,.F.);
#6570=EDGE_CURVE('',#5214,#5213,#2826,.T.);
#6571=EDGE_CURVE('',#5211,#5214,#2827,.T.);
#6572=EDGE_CURVE('',#5215,#5216,#2828,.T.);
#6573=EDGE_CURVE('',#5217,#5215,#2829,.T.);
#6574=EDGE_CURVE('',#5217,#5218,#2830,.T.);
#6575=EDGE_CURVE('',#5218,#5216,#2831,.F.);
#6576=EDGE_CURVE('',#5219,#5219,#4441,.F.);
#6577=EDGE_CURVE('',#5219,#5220,#2832,.T.);
#6578=EDGE_CURVE('',#5220,#5220,#4442,.T.);
#6579=EDGE_CURVE('',#5221,#5222,#2833,.T.);
#6580=EDGE_CURVE('',#5222,#5223,#2834,.F.);
#6581=EDGE_CURVE('',#5224,#5223,#2835,.T.);
#6582=EDGE_CURVE('',#5221,#5224,#2836,.T.);
#6583=EDGE_CURVE('',#5225,#5226,#2837,.T.);
#6584=EDGE_CURVE('',#5226,#5227,#2838,.T.);
#6585=EDGE_CURVE('',#5227,#5228,#2839,.F.);
#6586=EDGE_CURVE('',#5225,#5228,#2840,.T.);
#6587=EDGE_CURVE('',#5226,#5224,#2841,.T.);
#6588=EDGE_CURVE('',#5223,#5227,#2842,.F.);
#6589=EDGE_CURVE('',#5229,#5217,#2843,.T.);
#6590=EDGE_CURVE('',#5229,#5230,#2844,.T.);
#6591=EDGE_CURVE('',#5230,#5218,#2845,.F.);
#6592=EDGE_CURVE('',#5231,#5229,#2846,.T.);
#6593=EDGE_CURVE('',#5231,#5232,#2847,.T.);
#6594=EDGE_CURVE('',#5232,#5230,#2848,.F.);
#6595=EDGE_CURVE('',#5231,#5233,#2849,.T.);
#6596=EDGE_CURVE('',#5233,#5234,#2850,.T.);
#6597=EDGE_CURVE('',#5234,#5232,#2851,.F.);
#6598=EDGE_CURVE('',#5233,#5235,#2852,.T.);
#6599=EDGE_CURVE('',#5235,#5236,#2853,.T.);
#6600=EDGE_CURVE('',#5236,#5234,#2854,.F.);
#6601=EDGE_CURVE('',#5237,#5235,#2855,.T.);
#6602=EDGE_CURVE('',#5237,#5238,#2856,.T.);
#6603=EDGE_CURVE('',#5238,#5236,#2857,.F.);
#6604=EDGE_CURVE('',#5239,#5237,#2858,.T.);
#6605=EDGE_CURVE('',#5239,#5240,#2859,.T.);
#6606=EDGE_CURVE('',#5240,#5238,#2860,.F.);
#6607=EDGE_CURVE('',#5241,#5239,#4443,.T.);
#6608=EDGE_CURVE('',#5241,#5242,#2861,.T.);
#6609=EDGE_CURVE('',#5242,#5240,#4444,.F.);
#6610=EDGE_CURVE('',#5243,#5241,#2862,.T.);
#6611=EDGE_CURVE('',#5243,#5244,#2863,.T.);
#6612=EDGE_CURVE('',#5244,#5242,#2864,.F.);
#6613=EDGE_CURVE('',#5243,#5245,#2865,.T.);
#6614=EDGE_CURVE('',#5245,#5246,#2866,.T.);
#6615=EDGE_CURVE('',#5246,#5244,#2867,.F.);
#6616=EDGE_CURVE('',#5247,#5245,#2868,.T.);
#6617=EDGE_CURVE('',#5247,#5248,#2869,.T.);
#6618=EDGE_CURVE('',#5248,#5246,#2870,.F.);
#6619=EDGE_CURVE('',#5225,#5247,#2871,.T.);
#6620=EDGE_CURVE('',#5228,#5248,#2872,.F.);
#6621=EDGE_CURVE('',#5249,#5250,#2873,.T.);
#6622=EDGE_CURVE('',#5250,#5251,#2874,.T.);
#6623=EDGE_CURVE('',#5251,#5252,#2875,.F.);
#6624=EDGE_CURVE('',#5249,#5252,#2876,.T.);
#6625=EDGE_CURVE('',#5250,#5214,#2877,.T.);
#6626=EDGE_CURVE('',#5213,#5251,#2878,.F.);
#6627=EDGE_CURVE('',#5203,#5209,#2879,.T.);
#6628=EDGE_CURVE('',#5206,#5210,#2880,.F.);
#6629=EDGE_CURVE('',#5253,#5254,#2881,.T.);
#6630=EDGE_CURVE('',#5254,#5255,#2882,.T.);
#6631=EDGE_CURVE('',#5255,#5256,#2883,.F.);
#6632=EDGE_CURVE('',#5253,#5256,#2884,.T.);
#6633=EDGE_CURVE('',#5257,#5254,#2885,.T.);
#6634=EDGE_CURVE('',#5257,#5258,#2886,.T.);
#6635=EDGE_CURVE('',#5258,#5255,#2887,.F.);
#6636=EDGE_CURVE('',#5249,#5257,#2888,.T.);
#6637=EDGE_CURVE('',#5252,#5258,#2889,.F.);
#6638=EDGE_CURVE('',#5259,#5260,#2890,.T.);
#6639=EDGE_CURVE('',#5260,#5261,#2891,.T.);
#6640=EDGE_CURVE('',#5261,#5262,#2892,.F.);
#6641=EDGE_CURVE('',#5259,#5262,#2893,.T.);
#6642=EDGE_CURVE('',#5260,#5215,#2894,.T.);
#6643=EDGE_CURVE('',#5216,#5261,#2895,.F.);
#6644=EDGE_CURVE('',#5263,#5211,#2896,.T.);
#6645=EDGE_CURVE('',#5263,#5264,#2897,.T.);
#6646=EDGE_CURVE('',#5264,#5212,#2898,.F.);
#6647=EDGE_CURVE('',#5265,#5263,#2899,.T.);
#6648=EDGE_CURVE('',#5265,#5266,#2900,.T.);
#6649=EDGE_CURVE('',#5266,#5264,#2901,.F.);
#6650=EDGE_CURVE('',#5265,#5267,#2902,.T.);
#6651=EDGE_CURVE('',#5267,#5268,#2903,.T.);
#6652=EDGE_CURVE('',#5268,#5266,#2904,.F.);
#6653=EDGE_CURVE('',#5267,#5269,#2905,.T.);
#6654=EDGE_CURVE('',#5269,#5270,#2906,.T.);
#6655=EDGE_CURVE('',#5270,#5268,#2907,.F.);
#6656=EDGE_CURVE('',#5271,#5269,#2908,.T.);
#6657=EDGE_CURVE('',#5271,#5272,#2909,.T.);
#6658=EDGE_CURVE('',#5272,#5270,#2910,.F.);
#6659=EDGE_CURVE('',#5273,#5271,#2911,.T.);
#6660=EDGE_CURVE('',#5273,#5274,#2912,.T.);
#6661=EDGE_CURVE('',#5274,#5272,#2913,.F.);
#6662=EDGE_CURVE('',#5275,#5273,#4445,.T.);
#6663=EDGE_CURVE('',#5275,#5276,#2914,.T.);
#6664=EDGE_CURVE('',#5276,#5274,#4446,.F.);
#6665=EDGE_CURVE('',#5277,#5275,#2915,.T.);
#6666=EDGE_CURVE('',#5277,#5278,#2916,.T.);
#6667=EDGE_CURVE('',#5278,#5276,#2917,.F.);
#6668=EDGE_CURVE('',#5277,#5279,#2918,.T.);
#6669=EDGE_CURVE('',#5279,#5280,#2919,.T.);
#6670=EDGE_CURVE('',#5280,#5278,#2920,.F.);
#6671=EDGE_CURVE('',#5281,#5279,#2921,.T.);
#6672=EDGE_CURVE('',#5281,#5282,#2922,.T.);
#6673=EDGE_CURVE('',#5282,#5280,#2923,.F.);
#6674=EDGE_CURVE('',#5259,#5281,#2924,.T.);
#6675=EDGE_CURVE('',#5262,#5282,#2925,.F.);
#6676=EDGE_CURVE('',#5200,#5207,#2926,.T.);
#6677=EDGE_CURVE('',#5208,#5201,#2927,.F.);
#6678=EDGE_CURVE('',#5283,#5221,#2928,.T.);
#6679=EDGE_CURVE('',#5283,#5284,#2929,.T.);
#6680=EDGE_CURVE('',#5284,#5222,#2930,.F.);
#6681=EDGE_CURVE('',#5285,#5283,#2931,.T.);
#6682=EDGE_CURVE('',#5285,#5286,#2932,.T.);
#6683=EDGE_CURVE('',#5286,#5284,#2933,.F.);
#6684=EDGE_CURVE('',#5285,#5287,#2934,.T.);
#6685=EDGE_CURVE('',#5287,#5288,#2935,.T.);
#6686=EDGE_CURVE('',#5288,#5286,#2936,.F.);
#6687=EDGE_CURVE('',#5287,#5289,#2937,.T.);
#6688=EDGE_CURVE('',#5289,#5290,#2938,.T.);
#6689=EDGE_CURVE('',#5290,#5288,#2939,.F.);
#6690=EDGE_CURVE('',#5291,#5289,#2940,.T.);
#6691=EDGE_CURVE('',#5291,#5292,#2941,.T.);
#6692=EDGE_CURVE('',#5292,#5290,#2942,.F.);
#6693=EDGE_CURVE('',#5199,#5293,#2943,.T.);
#6694=EDGE_CURVE('',#5202,#5294,#2944,.T.);
#6695=EDGE_CURVE('',#5293,#5294,#2945,.T.);
#6696=EDGE_CURVE('',#5293,#5295,#2946,.T.);
#6697=EDGE_CURVE('',#5296,#5294,#2947,.F.);
#6698=EDGE_CURVE('',#5295,#5296,#2948,.T.);
#6699=EDGE_CURVE('',#5297,#5291,#2949,.T.);
#6700=EDGE_CURVE('',#5298,#5253,#2950,.T.);
#6701=EDGE_CURVE('',#5298,#5299,#2951,.T.);
#6702=EDGE_CURVE('',#5300,#5299,#2952,.T.);
#6703=EDGE_CURVE('',#5301,#5300,#2953,.T.);
#6704=EDGE_CURVE('',#5301,#5302,#2954,.T.);
#6705=EDGE_CURVE('',#5302,#5303,#2955,.T.);
#6706=EDGE_CURVE('',#5304,#5303,#2956,.T.);
#6707=EDGE_CURVE('',#5305,#5304,#2957,.T.);
#6708=EDGE_CURVE('',#5306,#5305,#2958,.T.);
#6709=EDGE_CURVE('',#5306,#5307,#2959,.T.);
#6710=EDGE_CURVE('',#5307,#5308,#2960,.T.);
#6711=EDGE_CURVE('',#5309,#5308,#2961,.T.);
#6712=EDGE_CURVE('',#5310,#5309,#2962,.T.);
#6713=EDGE_CURVE('',#5311,#5310,#4447,.T.);
#6714=EDGE_CURVE('',#5312,#5311,#2963,.T.);
#6715=EDGE_CURVE('',#5312,#5313,#2964,.T.);
#6716=EDGE_CURVE('',#5314,#5313,#2965,.T.);
#6717=EDGE_CURVE('',#5315,#5314,#2966,.T.);
#6718=EDGE_CURVE('',#5315,#5316,#2967,.T.);
#6719=EDGE_CURVE('',#5316,#5317,#2968,.T.);
#6720=EDGE_CURVE('',#5318,#5317,#2969,.T.);
#6721=EDGE_CURVE('',#5319,#5318,#2970,.T.);
#6722=EDGE_CURVE('',#5320,#5319,#2971,.T.);
#6723=EDGE_CURVE('',#5320,#5321,#2972,.T.);
#6724=EDGE_CURVE('',#5321,#5322,#2973,.T.);
#6725=EDGE_CURVE('',#5323,#5322,#2974,.T.);
#6726=EDGE_CURVE('',#5324,#5323,#2975,.T.);
#6727=EDGE_CURVE('',#5325,#5324,#4448,.T.);
#6728=EDGE_CURVE('',#5326,#5325,#2976,.T.);
#6729=EDGE_CURVE('',#5326,#5327,#2977,.T.);
#6730=EDGE_CURVE('',#5328,#5327,#2978,.T.);
#6731=EDGE_CURVE('',#5329,#5328,#2979,.T.);
#6732=EDGE_CURVE('',#5329,#5330,#2980,.T.);
#6733=EDGE_CURVE('',#5330,#5331,#2981,.T.);
#6734=EDGE_CURVE('',#5332,#5331,#2982,.T.);
#6735=EDGE_CURVE('',#5333,#5332,#2983,.T.);
#6736=EDGE_CURVE('',#5334,#5333,#2984,.T.);
#6737=EDGE_CURVE('',#5334,#5335,#2985,.T.);
#6738=EDGE_CURVE('',#5335,#5336,#2986,.T.);
#6739=EDGE_CURVE('',#5297,#5336,#2987,.T.);
#6740=EDGE_CURVE('',#5295,#5337,#2988,.T.);
#6741=EDGE_CURVE('',#5338,#5337,#2989,.T.);
#6742=EDGE_CURVE('',#5339,#5338,#2990,.T.);
#6743=EDGE_CURVE('',#5339,#5340,#2991,.T.);
#6744=EDGE_CURVE('',#5340,#5204,#2992,.T.);
#6745=EDGE_CURVE('',#5341,#5341,#4449,.T.);
#6746=EDGE_CURVE('',#5340,#5342,#2993,.T.);
#6747=EDGE_CURVE('',#5342,#5205,#2994,.T.);
#6748=EDGE_CURVE('',#5339,#5343,#2995,.T.);
#6749=EDGE_CURVE('',#5342,#5343,#2996,.F.);
#6750=EDGE_CURVE('',#5337,#5344,#2997,.T.);
#6751=EDGE_CURVE('',#5345,#5344,#2998,.T.);
#6752=EDGE_CURVE('',#5338,#5345,#2999,.T.);
#6753=EDGE_CURVE('',#5304,#5346,#3000,.T.);
#6754=EDGE_CURVE('',#5303,#5347,#3001,.T.);
#6755=EDGE_CURVE('',#5346,#5347,#3002,.T.);
#6756=EDGE_CURVE('',#5317,#5348,#3003,.T.);
#6757=EDGE_CURVE('',#5349,#5348,#3004,.T.);
#6758=EDGE_CURVE('',#5318,#5349,#3005,.T.);
#6759=EDGE_CURVE('',#5341,#5350,#3006,.T.);
#6760=EDGE_CURVE('',#5350,#5350,#4450,.T.);
#6761=EDGE_CURVE('',#5332,#5351,#3007,.T.);
#6762=EDGE_CURVE('',#5331,#5352,#3008,.T.);
#6763=EDGE_CURVE('',#5351,#5352,#3009,.T.);
#6764=EDGE_CURVE('',#5329,#5353,#3010,.T.);
#6765=EDGE_CURVE('',#5354,#5353,#3011,.T.);
#6766=EDGE_CURVE('',#5330,#5354,#3012,.T.);
#6767=EDGE_CURVE('',#5352,#5354,#3013,.T.);
#6768=EDGE_CURVE('',#5355,#5349,#3014,.T.);
#6769=EDGE_CURVE('',#5319,#5355,#3015,.T.);
#6770=EDGE_CURVE('',#5356,#5355,#3016,.T.);
#6771=EDGE_CURVE('',#5320,#5356,#3017,.T.);
#6772=EDGE_CURVE('',#5357,#5356,#3018,.T.);
#6773=EDGE_CURVE('',#5321,#5357,#3019,.T.);
#6774=EDGE_CURVE('',#5358,#5357,#3020,.T.);
#6775=EDGE_CURVE('',#5322,#5358,#3021,.T.);
#6776=EDGE_CURVE('',#5359,#5358,#3022,.T.);
#6777=EDGE_CURVE('',#5323,#5359,#3023,.T.);
#6778=EDGE_CURVE('',#5360,#5359,#3024,.T.);
#6779=EDGE_CURVE('',#5324,#5360,#3025,.T.);
#6780=EDGE_CURVE('',#5361,#5360,#4451,.T.);
#6781=EDGE_CURVE('',#5325,#5361,#3026,.T.);
#6782=EDGE_CURVE('',#5362,#5361,#3027,.T.);
#6783=EDGE_CURVE('',#5326,#5362,#3028,.T.);
#6784=EDGE_CURVE('',#5363,#5362,#3029,.T.);
#6785=EDGE_CURVE('',#5327,#5363,#3030,.T.);
#6786=EDGE_CURVE('',#5364,#5363,#3031,.T.);
#6787=EDGE_CURVE('',#5328,#5364,#3032,.T.);
#6788=EDGE_CURVE('',#5353,#5364,#3033,.T.);
#6789=EDGE_CURVE('',#5301,#5365,#3034,.T.);
#6790=EDGE_CURVE('',#5366,#5365,#3035,.T.);
#6791=EDGE_CURVE('',#5302,#5366,#3036,.T.);
#6792=EDGE_CURVE('',#5347,#5366,#3037,.T.);
#6793=EDGE_CURVE('',#5343,#5345,#3038,.T.);
#6794=EDGE_CURVE('',#5367,#5256,#3039,.T.);
#6795=EDGE_CURVE('',#5298,#5367,#3040,.T.);
#6796=EDGE_CURVE('',#5368,#5367,#3041,.T.);
#6797=EDGE_CURVE('',#5299,#5368,#3042,.T.);
#6798=EDGE_CURVE('',#5369,#5368,#3043,.T.);
#6799=EDGE_CURVE('',#5300,#5369,#3044,.T.);
#6800=EDGE_CURVE('',#5365,#5369,#3045,.T.);
#6801=EDGE_CURVE('',#5315,#5370,#3046,.T.);
#6802=EDGE_CURVE('',#5371,#5370,#3047,.T.);
#6803=EDGE_CURVE('',#5316,#5371,#3048,.T.);
#6804=EDGE_CURVE('',#5348,#5371,#3049,.T.);
#6805=EDGE_CURVE('',#5372,#5346,#3050,.T.);
#6806=EDGE_CURVE('',#5305,#5372,#3051,.T.);
#6807=EDGE_CURVE('',#5373,#5372,#3052,.T.);
#6808=EDGE_CURVE('',#5306,#5373,#3053,.T.);
#6809=EDGE_CURVE('',#5374,#5373,#3054,.T.);
#6810=EDGE_CURVE('',#5307,#5374,#3055,.T.);
#6811=EDGE_CURVE('',#5375,#5374,#3056,.T.);
#6812=EDGE_CURVE('',#5308,#5375,#3057,.T.);
#6813=EDGE_CURVE('',#5376,#5375,#3058,.T.);
#6814=EDGE_CURVE('',#5309,#5376,#3059,.T.);
#6815=EDGE_CURVE('',#5377,#5376,#3060,.T.);
#6816=EDGE_CURVE('',#5310,#5377,#3061,.T.);
#6817=EDGE_CURVE('',#5378,#5377,#4452,.T.);
#6818=EDGE_CURVE('',#5311,#5378,#3062,.T.);
#6819=EDGE_CURVE('',#5379,#5378,#3063,.T.);
#6820=EDGE_CURVE('',#5312,#5379,#3064,.T.);
#6821=EDGE_CURVE('',#5380,#5379,#3065,.T.);
#6822=EDGE_CURVE('',#5313,#5380,#3066,.T.);
#6823=EDGE_CURVE('',#5381,#5380,#3067,.T.);
#6824=EDGE_CURVE('',#5314,#5381,#3068,.T.);
#6825=EDGE_CURVE('',#5370,#5381,#3069,.T.);
#6826=EDGE_CURVE('',#5344,#5296,#3070,.T.);
#6827=EDGE_CURVE('',#5382,#5351,#3071,.T.);
#6828=EDGE_CURVE('',#5333,#5382,#3072,.T.);
#6829=EDGE_CURVE('',#5383,#5382,#3073,.T.);
#6830=EDGE_CURVE('',#5334,#5383,#3074,.T.);
#6831=EDGE_CURVE('',#5384,#5383,#3075,.T.);
#6832=EDGE_CURVE('',#5335,#5384,#3076,.T.);
#6833=EDGE_CURVE('',#5385,#5384,#3077,.T.);
#6834=EDGE_CURVE('',#5336,#5385,#3078,.T.);
#6835=EDGE_CURVE('',#5386,#5385,#3079,.T.);
#6836=EDGE_CURVE('',#5297,#5386,#3080,.T.);
#6837=EDGE_CURVE('',#5386,#5292,#3081,.F.);
#6838=EDGE_CURVE('',#5387,#5387,#4453,.T.);
#6839=EDGE_CURVE('',#5388,#5388,#4454,.T.);
#6840=EDGE_CURVE('',#5389,#5389,#4455,.T.);
#6841=EDGE_CURVE('',#5389,#5390,#3082,.T.);
#6842=EDGE_CURVE('',#5390,#5390,#4456,.F.);
#6843=EDGE_CURVE('',#5391,#5391,#4457,.T.);
#6844=EDGE_CURVE('',#5392,#5392,#4458,.T.);
#6845=EDGE_CURVE('',#5391,#5393,#3083,.T.);
#6846=EDGE_CURVE('',#5393,#5393,#4459,.T.);
#6847=EDGE_CURVE('',#5387,#5392,#3084,.T.);
#6848=EDGE_CURVE('',#5394,#5394,#4460,.T.);
#6849=EDGE_CURVE('',#5394,#5388,#3085,.T.);
#6850=EDGE_CURVE('',#5395,#5395,#4461,.T.);
#6851=EDGE_CURVE('',#5395,#5396,#3086,.T.);
#6852=EDGE_CURVE('',#5396,#5396,#4462,.T.);
#6853=EDGE_CURVE('',#5397,#5398,#3087,.T.);
#6854=EDGE_CURVE('',#5398,#5399,#3088,.T.);
#6855=EDGE_CURVE('',#5400,#5399,#3089,.T.);
#6856=EDGE_CURVE('',#5397,#5400,#3090,.T.);
#6857=EDGE_CURVE('',#5401,#5397,#3091,.T.);
#6858=EDGE_CURVE('',#5402,#5400,#3092,.T.);
#6859=EDGE_CURVE('',#5401,#5402,#3093,.T.);
#6860=EDGE_CURVE('',#5403,#5401,#3094,.T.);
#6861=EDGE_CURVE('',#5404,#5402,#3095,.T.);
#6862=EDGE_CURVE('',#5403,#5404,#3096,.T.);
#6863=EDGE_CURVE('',#5398,#5403,#3097,.T.);
#6864=EDGE_CURVE('',#5399,#5404,#3098,.T.);
#6865=EDGE_CURVE('',#5405,#5406,#3099,.T.);
#6866=EDGE_CURVE('',#5406,#5407,#3100,.T.);
#6867=EDGE_CURVE('',#5408,#5407,#3101,.T.);
#6868=EDGE_CURVE('',#5405,#5408,#3102,.T.);
#6869=EDGE_CURVE('',#5409,#5405,#3103,.T.);
#6870=EDGE_CURVE('',#5410,#5408,#3104,.T.);
#6871=EDGE_CURVE('',#5409,#5410,#3105,.T.);
#6872=EDGE_CURVE('',#5411,#5409,#3106,.T.);
#6873=EDGE_CURVE('',#5412,#5410,#3107,.T.);
#6874=EDGE_CURVE('',#5411,#5412,#3108,.T.);
#6875=EDGE_CURVE('',#5406,#5411,#3109,.T.);
#6876=EDGE_CURVE('',#5407,#5412,#3110,.T.);
#6877=EDGE_CURVE('',#5413,#5413,#4463,.T.);
#6878=EDGE_CURVE('',#5413,#5414,#3111,.T.);
#6879=EDGE_CURVE('',#5414,#5414,#4464,.T.);
#6880=EDGE_CURVE('',#5415,#5415,#4465,.T.);
#6881=EDGE_CURVE('',#5415,#5416,#3112,.T.);
#6882=EDGE_CURVE('',#5416,#5416,#4466,.T.);
#6883=EDGE_CURVE('',#5417,#5418,#3113,.T.);
#6884=EDGE_CURVE('',#5418,#5419,#3114,.T.);
#6885=EDGE_CURVE('',#5420,#5419,#3115,.T.);
#6886=EDGE_CURVE('',#5417,#5420,#3116,.T.);
#6887=EDGE_CURVE('',#5421,#5417,#3117,.T.);
#6888=EDGE_CURVE('',#5422,#5420,#3118,.T.);
#6889=EDGE_CURVE('',#5421,#5422,#3119,.T.);
#6890=EDGE_CURVE('',#5423,#5421,#3120,.T.);
#6891=EDGE_CURVE('',#5424,#5422,#3121,.T.);
#6892=EDGE_CURVE('',#5423,#5424,#3122,.T.);
#6893=EDGE_CURVE('',#5418,#5423,#3123,.T.);
#6894=EDGE_CURVE('',#5419,#5424,#3124,.T.);
#6895=EDGE_CURVE('',#5425,#5425,#4467,.T.);
#6896=EDGE_CURVE('',#5425,#5426,#3125,.T.);
#6897=EDGE_CURVE('',#5426,#5426,#4468,.T.);
#6898=EDGE_CURVE('',#5427,#5427,#4469,.T.);
#6899=EDGE_CURVE('',#5427,#5428,#3126,.T.);
#6900=EDGE_CURVE('',#5428,#5428,#4470,.T.);
#6901=EDGE_CURVE('',#5429,#5430,#3127,.T.);
#6902=EDGE_CURVE('',#5429,#5431,#3128,.T.);
#6903=EDGE_CURVE('',#5432,#5431,#3129,.T.);
#6904=EDGE_CURVE('',#5430,#5432,#3130,.T.);
#6905=EDGE_CURVE('',#5430,#5433,#3131,.T.);
#6906=EDGE_CURVE('',#5434,#5432,#3132,.T.);
#6907=EDGE_CURVE('',#5433,#5434,#3133,.T.);
#6908=EDGE_CURVE('',#5433,#5435,#3134,.T.);
#6909=EDGE_CURVE('',#5436,#5434,#3135,.T.);
#6910=EDGE_CURVE('',#5435,#5436,#3136,.T.);
#6911=EDGE_CURVE('',#5435,#5437,#3137,.T.);
#6912=EDGE_CURVE('',#5438,#5436,#3138,.T.);
#6913=EDGE_CURVE('',#5437,#5438,#3139,.T.);
#6914=EDGE_CURVE('',#5437,#5439,#3140,.T.);
#6915=EDGE_CURVE('',#5440,#5438,#3141,.T.);
#6916=EDGE_CURVE('',#5439,#5440,#3142,.T.);
#6917=EDGE_CURVE('',#5439,#5441,#3143,.T.);
#6918=EDGE_CURVE('',#5442,#5440,#3144,.T.);
#6919=EDGE_CURVE('',#5441,#5442,#3145,.T.);
#6920=EDGE_CURVE('',#5441,#5443,#3146,.T.);
#6921=EDGE_CURVE('',#5444,#5442,#3147,.T.);
#6922=EDGE_CURVE('',#5443,#5444,#3148,.T.);
#6923=EDGE_CURVE('',#5443,#5445,#3149,.T.);
#6924=EDGE_CURVE('',#5446,#5444,#3150,.T.);
#6925=EDGE_CURVE('',#5445,#5446,#3151,.T.);
#6926=EDGE_CURVE('',#5445,#5447,#3152,.T.);
#6927=EDGE_CURVE('',#5448,#5446,#3153,.T.);
#6928=EDGE_CURVE('',#5447,#5448,#3154,.T.);
#6929=EDGE_CURVE('',#5449,#5447,#4471,.T.);
#6930=EDGE_CURVE('',#5450,#5448,#4472,.T.);
#6931=EDGE_CURVE('',#5449,#5450,#3155,.T.);
#6932=EDGE_CURVE('',#5449,#5451,#3156,.T.);
#6933=EDGE_CURVE('',#5452,#5450,#3157,.T.);
#6934=EDGE_CURVE('',#5451,#5452,#3158,.T.);
#6935=EDGE_CURVE('',#5453,#5451,#4473,.T.);
#6936=EDGE_CURVE('',#5454,#5452,#4474,.T.);
#6937=EDGE_CURVE('',#5453,#5454,#3159,.T.);
#6938=EDGE_CURVE('',#5453,#5455,#3160,.T.);
#6939=EDGE_CURVE('',#5456,#5454,#3161,.T.);
#6940=EDGE_CURVE('',#5455,#5456,#3162,.T.);
#6941=EDGE_CURVE('',#5457,#5455,#4475,.T.);
#6942=EDGE_CURVE('',#5458,#5456,#4476,.T.);
#6943=EDGE_CURVE('',#5457,#5458,#3163,.T.);
#6944=EDGE_CURVE('',#5457,#5459,#3164,.T.);
#6945=EDGE_CURVE('',#5460,#5458,#3165,.T.);
#6946=EDGE_CURVE('',#5459,#5460,#3166,.T.);
#6947=EDGE_CURVE('',#5429,#5459,#4477,.T.);
#6948=EDGE_CURVE('',#5431,#5460,#4478,.T.);
#6949=EDGE_CURVE('',#5461,#5461,#1011,.T.);
#6950=EDGE_CURVE('',#5461,#5462,#3167,.T.);
#6951=EDGE_CURVE('',#5462,#5462,#1012,.T.);
#6952=EDGE_CURVE('',#5463,#5464,#1013,.T.);
#6953=EDGE_CURVE('',#5465,#5463,#1014,.T.);
#6954=EDGE_CURVE('',#5464,#5465,#1015,.T.);
#6955=EDGE_CURVE('',#5464,#5466,#3168,.T.);
#6956=EDGE_CURVE('',#5467,#5466,#1016,.T.);
#6957=EDGE_CURVE('',#5468,#5467,#1017,.T.);
#6958=EDGE_CURVE('',#5466,#5468,#1018,.T.);
#6959=EDGE_CURVE('',#5469,#5469,#4479,.T.);
#6960=EDGE_CURVE('',#5469,#5467,#3169,.T.);
#6961=EDGE_CURVE('',#5468,#5470,#3170,.T.);
#6962=EDGE_CURVE('',#5470,#5470,#4480,.T.);
#6963=EDGE_CURVE('',#5471,#5471,#4481,.T.);
#6964=EDGE_CURVE('',#5472,#5472,#4482,.T.);
#6965=EDGE_CURVE('',#5473,#5473,#4483,.T.);
#6966=EDGE_CURVE('',#5474,#5474,#4484,.T.);
#6967=EDGE_CURVE('',#5474,#5472,#3171,.T.);
#6968=EDGE_CURVE('',#5473,#5475,#3172,.T.);
#6969=EDGE_CURVE('',#5475,#5475,#4485,.T.);
#6970=EDGE_CURVE('',#5476,#5476,#4486,.T.);
#6971=EDGE_CURVE('',#5476,#5463,#3173,.T.);
#6972=EDGE_CURVE('',#5465,#5471,#3174,.T.);
#6973=EDGE_CURVE('',#5477,#5477,#4487,.T.);
#6974=EDGE_CURVE('',#5477,#5478,#3175,.T.);
#6975=EDGE_CURVE('',#5478,#5478,#4488,.T.);
#6976=EDGE_CURVE('',#5479,#5480,#4489,.T.);
#6977=EDGE_CURVE('',#5480,#5481,#3176,.T.);
#6978=EDGE_CURVE('',#5481,#5482,#4490,.T.);
#6979=EDGE_CURVE('',#5482,#5479,#3177,.T.);
#6980=EDGE_CURVE('',#5483,#5484,#4491,.T.);
#6981=EDGE_CURVE('',#5484,#5485,#3178,.T.);
#6982=EDGE_CURVE('',#5485,#5486,#4492,.T.);
#6983=EDGE_CURVE('',#5486,#5483,#3179,.T.);
#6984=EDGE_CURVE('',#5487,#5484,#3180,.T.);
#6985=EDGE_CURVE('',#5488,#5487,#3181,.T.);
#6986=EDGE_CURVE('',#5485,#5488,#3182,.T.);
#6987=EDGE_CURVE('',#5489,#5488,#4493,.T.);
#6988=EDGE_CURVE('',#5486,#5489,#3183,.T.);
#6989=EDGE_CURVE('',#5490,#5489,#3184,.T.);
#6990=EDGE_CURVE('',#5483,#5490,#3185,.T.);
#6991=EDGE_CURVE('',#5487,#5490,#4494,.T.);
#6992=EDGE_CURVE('',#5491,#5480,#3186,.T.);
#6993=EDGE_CURVE('',#5492,#5491,#3187,.T.);
#6994=EDGE_CURVE('',#5481,#5492,#3188,.T.);
#6995=EDGE_CURVE('',#5493,#5492,#4495,.T.);
#6996=EDGE_CURVE('',#5482,#5493,#3189,.T.);
#6997=EDGE_CURVE('',#5494,#5493,#3190,.T.);
#6998=EDGE_CURVE('',#5479,#5494,#3191,.T.);
#6999=EDGE_CURVE('',#5491,#5494,#4496,.T.);
#7000=EDGE_CURVE('',#5495,#5495,#4497,.T.);
#7001=EDGE_CURVE('',#5495,#5496,#3192,.T.);
#7002=EDGE_CURVE('',#5496,#5496,#4498,.T.);
#7003=EDGE_CURVE('',#5497,#5498,#3193,.T.);
#7004=EDGE_CURVE('',#5498,#5499,#3194,.T.);
#7005=EDGE_CURVE('',#5500,#5499,#3195,.T.);
#7006=EDGE_CURVE('',#5497,#5500,#3196,.T.);
#7007=EDGE_CURVE('',#5501,#5497,#4499,.T.);
#7008=EDGE_CURVE('',#5502,#5500,#4500,.T.);
#7009=EDGE_CURVE('',#5501,#5502,#3197,.T.);
#7010=EDGE_CURVE('',#5503,#5501,#3198,.T.);
#7011=EDGE_CURVE('',#5504,#5502,#3199,.T.);
#7012=EDGE_CURVE('',#5503,#5504,#3200,.T.);
#7013=EDGE_CURVE('',#5498,#5503,#4501,.T.);
#7014=EDGE_CURVE('',#5499,#5504,#4502,.T.);
#7015=EDGE_CURVE('',#5505,#5505,#4503,.T.);
#7016=EDGE_CURVE('',#5505,#5506,#3201,.T.);
#7017=EDGE_CURVE('',#5506,#5506,#4504,.T.);
#7018=EDGE_CURVE('',#5507,#5507,#4505,.T.);
#7019=EDGE_CURVE('',#5507,#5508,#3202,.T.);
#7020=EDGE_CURVE('',#5508,#5508,#4506,.T.);
#7021=EDGE_CURVE('',#5509,#5509,#4507,.T.);
#7022=EDGE_CURVE('',#5509,#5510,#3203,.T.);
#7023=EDGE_CURVE('',#5510,#5510,#4508,.T.);
#7024=EDGE_CURVE('',#5511,#5511,#4509,.T.);
#7025=EDGE_CURVE('',#5511,#5512,#3204,.T.);
#7026=EDGE_CURVE('',#5512,#5512,#4510,.T.);
#7027=EDGE_CURVE('',#5513,#5513,#4511,.T.);
#7028=EDGE_CURVE('',#5513,#5514,#3205,.T.);
#7029=EDGE_CURVE('',#5514,#5514,#4512,.T.);
#7030=EDGE_CURVE('',#5515,#5516,#3206,.T.);
#7031=EDGE_CURVE('',#5516,#5517,#3207,.T.);
#7032=EDGE_CURVE('',#5518,#5517,#3208,.T.);
#7033=EDGE_CURVE('',#5515,#5518,#3209,.T.);
#7034=EDGE_CURVE('',#5519,#5515,#4513,.T.);
#7035=EDGE_CURVE('',#5520,#5518,#4514,.T.);
#7036=EDGE_CURVE('',#5519,#5520,#3210,.T.);
#7037=EDGE_CURVE('',#5521,#5519,#3211,.T.);
#7038=EDGE_CURVE('',#5522,#5520,#3212,.T.);
#7039=EDGE_CURVE('',#5521,#5522,#3213,.T.);
#7040=EDGE_CURVE('',#5516,#5521,#4515,.T.);
#7041=EDGE_CURVE('',#5517,#5522,#4516,.T.);
#7042=EDGE_CURVE('',#5523,#5524,#3214,.T.);
#7043=EDGE_CURVE('',#5524,#5525,#3215,.T.);
#7044=EDGE_CURVE('',#5526,#5525,#3216,.T.);
#7045=EDGE_CURVE('',#5523,#5526,#3217,.T.);
#7046=EDGE_CURVE('',#5527,#5523,#4517,.T.);
#7047=EDGE_CURVE('',#5528,#5526,#4518,.T.);
#7048=EDGE_CURVE('',#5527,#5528,#3218,.T.);
#7049=EDGE_CURVE('',#5529,#5527,#3219,.T.);
#7050=EDGE_CURVE('',#5530,#5528,#3220,.T.);
#7051=EDGE_CURVE('',#5529,#5530,#3221,.T.);
#7052=EDGE_CURVE('',#5524,#5529,#4519,.T.);
#7053=EDGE_CURVE('',#5525,#5530,#4520,.T.);
#7054=EDGE_CURVE('',#5531,#5531,#4521,.T.);
#7055=EDGE_CURVE('',#5531,#5532,#3222,.T.);
#7056=EDGE_CURVE('',#5532,#5532,#4522,.T.);
#7057=EDGE_CURVE('',#5533,#5533,#4523,.T.);
#7058=EDGE_CURVE('',#5533,#5534,#3223,.T.);
#7059=EDGE_CURVE('',#5534,#5534,#4524,.T.);
#7060=EDGE_CURVE('',#5535,#5535,#4525,.T.);
#7061=EDGE_CURVE('',#5535,#5536,#3224,.T.);
#7062=EDGE_CURVE('',#5536,#5536,#4526,.T.);
#7063=EDGE_CURVE('',#5537,#5537,#4527,.T.);
#7064=EDGE_CURVE('',#5537,#5538,#3225,.T.);
#7065=EDGE_CURVE('',#5538,#5538,#4528,.T.);
#7066=EDGE_CURVE('',#5539,#5539,#4529,.T.);
#7067=EDGE_CURVE('',#5539,#5540,#3226,.T.);
#7068=EDGE_CURVE('',#5540,#5540,#4530,.T.);
#7069=EDGE_CURVE('',#5541,#5542,#3227,.T.);
#7070=EDGE_CURVE('',#5542,#5543,#3228,.T.);
#7071=EDGE_CURVE('',#5544,#5543,#3229,.T.);
#7072=EDGE_CURVE('',#5541,#5544,#3230,.T.);
#7073=EDGE_CURVE('',#5545,#5541,#4531,.T.);
#7074=EDGE_CURVE('',#5546,#5544,#4532,.T.);
#7075=EDGE_CURVE('',#5545,#5546,#3231,.T.);
#7076=EDGE_CURVE('',#5547,#5545,#3232,.T.);
#7077=EDGE_CURVE('',#5548,#5546,#3233,.T.);
#7078=EDGE_CURVE('',#5547,#5548,#3234,.T.);
#7079=EDGE_CURVE('',#5542,#5547,#4533,.T.);
#7080=EDGE_CURVE('',#5543,#5548,#4534,.T.);
#7081=EDGE_CURVE('',#5549,#5549,#4535,.T.);
#7082=EDGE_CURVE('',#5549,#5550,#3235,.T.);
#7083=EDGE_CURVE('',#5550,#5550,#4536,.T.);
#7084=EDGE_CURVE('',#5551,#5551,#4537,.T.);
#7085=EDGE_CURVE('',#5551,#5552,#3236,.T.);
#7086=EDGE_CURVE('',#5552,#5552,#4538,.T.);
#7087=EDGE_CURVE('',#5553,#5554,#3237,.T.);
#7088=EDGE_CURVE('',#5554,#5555,#3238,.T.);
#7089=EDGE_CURVE('',#5556,#5555,#3239,.T.);
#7090=EDGE_CURVE('',#5553,#5556,#3240,.T.);
#7091=EDGE_CURVE('',#5557,#5553,#4539,.T.);
#7092=EDGE_CURVE('',#5558,#5556,#4540,.T.);
#7093=EDGE_CURVE('',#5557,#5558,#3241,.T.);
#7094=EDGE_CURVE('',#5559,#5557,#3242,.T.);
#7095=EDGE_CURVE('',#5560,#5558,#3243,.T.);
#7096=EDGE_CURVE('',#5559,#5560,#3244,.T.);
#7097=EDGE_CURVE('',#5554,#5559,#4541,.T.);
#7098=EDGE_CURVE('',#5555,#5560,#4542,.T.);
#7099=EDGE_CURVE('',#5561,#5562,#3245,.T.);
#7100=EDGE_CURVE('',#5562,#5563,#3246,.T.);
#7101=EDGE_CURVE('',#5564,#5563,#3247,.T.);
#7102=EDGE_CURVE('',#5561,#5564,#3248,.T.);
#7103=EDGE_CURVE('',#5565,#5561,#4543,.T.);
#7104=EDGE_CURVE('',#5566,#5564,#4544,.T.);
#7105=EDGE_CURVE('',#5565,#5566,#3249,.T.);
#7106=EDGE_CURVE('',#5567,#5565,#3250,.T.);
#7107=EDGE_CURVE('',#5568,#5566,#3251,.T.);
#7108=EDGE_CURVE('',#5567,#5568,#3252,.T.);
#7109=EDGE_CURVE('',#5562,#5567,#4545,.T.);
#7110=EDGE_CURVE('',#5563,#5568,#4546,.T.);
#7111=EDGE_CURVE('',#5569,#5570,#3253,.T.);
#7112=EDGE_CURVE('',#5570,#5571,#3254,.T.);
#7113=EDGE_CURVE('',#5572,#5571,#3255,.T.);
#7114=EDGE_CURVE('',#5569,#5572,#3256,.T.);
#7115=EDGE_CURVE('',#5573,#5569,#4547,.T.);
#7116=EDGE_CURVE('',#5574,#5572,#4548,.T.);
#7117=EDGE_CURVE('',#5573,#5574,#3257,.T.);
#7118=EDGE_CURVE('',#5575,#5573,#3258,.T.);
#7119=EDGE_CURVE('',#5576,#5574,#3259,.T.);
#7120=EDGE_CURVE('',#5575,#5576,#3260,.T.);
#7121=EDGE_CURVE('',#5570,#5575,#4549,.T.);
#7122=EDGE_CURVE('',#5571,#5576,#4550,.T.);
#7123=EDGE_CURVE('',#5577,#5578,#3261,.T.);
#7124=EDGE_CURVE('',#5578,#5579,#3262,.T.);
#7125=EDGE_CURVE('',#5580,#5579,#3263,.T.);
#7126=EDGE_CURVE('',#5577,#5580,#3264,.T.);
#7127=EDGE_CURVE('',#5581,#5577,#4551,.T.);
#7128=EDGE_CURVE('',#5582,#5580,#4552,.T.);
#7129=EDGE_CURVE('',#5581,#5582,#3265,.T.);
#7130=EDGE_CURVE('',#5583,#5581,#3266,.T.);
#7131=EDGE_CURVE('',#5584,#5582,#3267,.T.);
#7132=EDGE_CURVE('',#5583,#5584,#3268,.T.);
#7133=EDGE_CURVE('',#5578,#5583,#4553,.T.);
#7134=EDGE_CURVE('',#5579,#5584,#4554,.T.);
#7135=EDGE_CURVE('',#5585,#5585,#4555,.T.);
#7136=EDGE_CURVE('',#5585,#5586,#3269,.T.);
#7137=EDGE_CURVE('',#5586,#5586,#4556,.T.);
#7138=EDGE_CURVE('',#5587,#5587,#4557,.T.);
#7139=EDGE_CURVE('',#5587,#5588,#3270,.T.);
#7140=EDGE_CURVE('',#5588,#5588,#4558,.T.);
#7141=EDGE_CURVE('',#5589,#5590,#3271,.T.);
#7142=EDGE_CURVE('',#5589,#5591,#3272,.T.);
#7143=EDGE_CURVE('',#5592,#5591,#3273,.T.);
#7144=EDGE_CURVE('',#5590,#5592,#3274,.T.);
#7145=EDGE_CURVE('',#5593,#5590,#4559,.T.);
#7146=EDGE_CURVE('',#5594,#5592,#4560,.T.);
#7147=EDGE_CURVE('',#5593,#5594,#3275,.T.);
#7148=EDGE_CURVE('',#5593,#5595,#3276,.T.);
#7149=EDGE_CURVE('',#5596,#5594,#3277,.T.);
#7150=EDGE_CURVE('',#5595,#5596,#3278,.T.);
#7151=EDGE_CURVE('',#5597,#5595,#4561,.T.);
#7152=EDGE_CURVE('',#5598,#5596,#4562,.T.);
#7153=EDGE_CURVE('',#5597,#5598,#3279,.T.);
#7154=EDGE_CURVE('',#5597,#5599,#3280,.T.);
#7155=EDGE_CURVE('',#5600,#5598,#3281,.T.);
#7156=EDGE_CURVE('',#5599,#5600,#3282,.T.);
#7157=EDGE_CURVE('',#5601,#5599,#4563,.T.);
#7158=EDGE_CURVE('',#5602,#5600,#4564,.T.);
#7159=EDGE_CURVE('',#5601,#5602,#3283,.T.);
#7160=EDGE_CURVE('',#5601,#5603,#3284,.T.);
#7161=EDGE_CURVE('',#5604,#5602,#3285,.T.);
#7162=EDGE_CURVE('',#5603,#5604,#3286,.T.);
#7163=EDGE_CURVE('',#5589,#5603,#4565,.T.);
#7164=EDGE_CURVE('',#5591,#5604,#4566,.T.);
#7165=EDGE_CURVE('',#5605,#5605,#4567,.T.);
#7166=EDGE_CURVE('',#5605,#5606,#3287,.T.);
#7167=EDGE_CURVE('',#5606,#5606,#4568,.T.);
#7168=EDGE_CURVE('',#5607,#5607,#4569,.T.);
#7169=EDGE_CURVE('',#5607,#5608,#3288,.T.);
#7170=EDGE_CURVE('',#5608,#5608,#4570,.T.);
#7171=EDGE_CURVE('',#5609,#5609,#4571,.T.);
#7172=EDGE_CURVE('',#5609,#5610,#3289,.T.);
#7173=EDGE_CURVE('',#5610,#5610,#4572,.T.);
#7174=EDGE_CURVE('',#5611,#5611,#4573,.T.);
#7175=EDGE_CURVE('',#5611,#5612,#3290,.T.);
#7176=EDGE_CURVE('',#5612,#5612,#4574,.T.);
#7177=EDGE_CURVE('',#5613,#5613,#4575,.T.);
#7178=EDGE_CURVE('',#5613,#5614,#3291,.T.);
#7179=EDGE_CURVE('',#5614,#5614,#4576,.T.);
#7180=EDGE_CURVE('',#5615,#5616,#4577,.T.);
#7181=EDGE_CURVE('',#5615,#5617,#3292,.T.);
#7182=EDGE_CURVE('',#5618,#5617,#4578,.T.);
#7183=EDGE_CURVE('',#5616,#5618,#3293,.T.);
#7184=EDGE_CURVE('',#5619,#5616,#3294,.T.);
#7185=EDGE_CURVE('',#5620,#5618,#3295,.T.);
#7186=EDGE_CURVE('',#5619,#5620,#3296,.T.);
#7187=EDGE_CURVE('',#5619,#5621,#4579,.T.);
#7188=EDGE_CURVE('',#5622,#5620,#4580,.T.);
#7189=EDGE_CURVE('',#5621,#5622,#3297,.T.);
#7190=EDGE_CURVE('',#5623,#5621,#3298,.T.);
#7191=EDGE_CURVE('',#5624,#5622,#3299,.T.);
#7192=EDGE_CURVE('',#5623,#5624,#3300,.T.);
#7193=EDGE_CURVE('',#5623,#5625,#4581,.T.);
#7194=EDGE_CURVE('',#5626,#5624,#4582,.T.);
#7195=EDGE_CURVE('',#5625,#5626,#3301,.T.);
#7196=EDGE_CURVE('',#5627,#5625,#3302,.T.);
#7197=EDGE_CURVE('',#5628,#5626,#3303,.T.);
#7198=EDGE_CURVE('',#5627,#5628,#3304,.T.);
#7199=EDGE_CURVE('',#5627,#5629,#4583,.T.);
#7200=EDGE_CURVE('',#5630,#5628,#4584,.T.);
#7201=EDGE_CURVE('',#5629,#5630,#3305,.T.);
#7202=EDGE_CURVE('',#5615,#5629,#3306,.T.);
#7203=EDGE_CURVE('',#5617,#5630,#3307,.T.);
#7204=EDGE_CURVE('',#5631,#5631,#4585,.T.);
#7205=EDGE_CURVE('',#5631,#5632,#3308,.T.);
#7206=EDGE_CURVE('',#5632,#5632,#4586,.T.);
#7207=EDGE_CURVE('',#5633,#5633,#4587,.T.);
#7208=EDGE_CURVE('',#5633,#5634,#4588,.T.);
#7209=EDGE_CURVE('',#5634,#5634,#4589,.T.);
#7210=EDGE_CURVE('',#5635,#5635,#4590,.T.);
#7211=EDGE_CURVE('',#5631,#5633,#3309,.T.);
#7212=EDGE_CURVE('',#5636,#5637,#3310,.T.);
#7213=EDGE_CURVE('',#5638,#5636,#3311,.T.);
#7214=EDGE_CURVE('',#5638,#5637,#3312,.T.);
#7215=EDGE_CURVE('',#5639,#5638,#3313,.T.);
#7216=EDGE_CURVE('',#5639,#5637,#3314,.T.);
#7217=EDGE_CURVE('',#5640,#5639,#3315,.T.);
#7218=EDGE_CURVE('',#5640,#5637,#3316,.T.);
#7219=EDGE_CURVE('',#5641,#5640,#3317,.T.);
#7220=EDGE_CURVE('',#5641,#5637,#3318,.T.);
#7221=EDGE_CURVE('',#5642,#5641,#3319,.T.);
#7222=EDGE_CURVE('',#5642,#5637,#3320,.T.);
#7223=EDGE_CURVE('',#5636,#5642,#3321,.T.);
#7224=EDGE_CURVE('',#5643,#5644,#3322,.T.);
#7225=EDGE_CURVE('',#5643,#5638,#3323,.T.);
#7226=EDGE_CURVE('',#5644,#5636,#3324,.T.);
#7227=EDGE_CURVE('',#5645,#5643,#3325,.T.);
#7228=EDGE_CURVE('',#5645,#5639,#3326,.T.);
#7229=EDGE_CURVE('',#5646,#5645,#3327,.T.);
#7230=EDGE_CURVE('',#5646,#5640,#3328,.T.);
#7231=EDGE_CURVE('',#5647,#5646,#3329,.T.);
#7232=EDGE_CURVE('',#5647,#5641,#3330,.T.);
#7233=EDGE_CURVE('',#5648,#5647,#3331,.T.);
#7234=EDGE_CURVE('',#5648,#5642,#3332,.T.);
#7235=EDGE_CURVE('',#5644,#5648,#3333,.T.);
#7236=EDGE_CURVE('',#5649,#5649,#4591,.T.);
#7237=EDGE_CURVE('',#5649,#5635,#4592,.T.);
#7238=ORIENTED_EDGE('',*,*,#5650,.T.);
#7239=ORIENTED_EDGE('',*,*,#5651,.T.);
#7240=ORIENTED_EDGE('',*,*,#5652,.T.);
#7241=ORIENTED_EDGE('',*,*,#5653,.T.);
#7242=ORIENTED_EDGE('',*,*,#5651,.F.);
#7243=ORIENTED_EDGE('',*,*,#5654,.T.);
#7244=ORIENTED_EDGE('',*,*,#5655,.T.);
#7245=ORIENTED_EDGE('',*,*,#5652,.F.);
#7246=ORIENTED_EDGE('',*,*,#5653,.F.);
#7247=ORIENTED_EDGE('',*,*,#5655,.F.);
#7248=ORIENTED_EDGE('',*,*,#5656,.T.);
#7249=ORIENTED_EDGE('',*,*,#5657,.T.);
#7250=ORIENTED_EDGE('',*,*,#5658,.F.);
#7251=ORIENTED_EDGE('',*,*,#5659,.F.);
#7252=ORIENTED_EDGE('',*,*,#5660,.T.);
#7253=ORIENTED_EDGE('',*,*,#5661,.T.);
#7254=ORIENTED_EDGE('',*,*,#5662,.F.);
#7255=ORIENTED_EDGE('',*,*,#5663,.T.);
#7256=ORIENTED_EDGE('',*,*,#5664,.T.);
#7257=ORIENTED_EDGE('',*,*,#5665,.F.);
#7258=ORIENTED_EDGE('',*,*,#5666,.F.);
#7259=ORIENTED_EDGE('',*,*,#5667,.T.);
#7260=ORIENTED_EDGE('',*,*,#5668,.T.);
#7261=ORIENTED_EDGE('',*,*,#5669,.F.);
#7262=ORIENTED_EDGE('',*,*,#5670,.F.);
#7263=ORIENTED_EDGE('',*,*,#5671,.F.);
#7264=ORIENTED_EDGE('',*,*,#5662,.T.);
#7265=ORIENTED_EDGE('',*,*,#5672,.T.);
#7266=ORIENTED_EDGE('',*,*,#5673,.T.);
#7267=ORIENTED_EDGE('',*,*,#5674,.F.);
#7268=ORIENTED_EDGE('',*,*,#5675,.T.);
#7269=ORIENTED_EDGE('',*,*,#5666,.T.);
#7270=ORIENTED_EDGE('',*,*,#5676,.F.);
#7271=ORIENTED_EDGE('',*,*,#5677,.F.);
#7272=ORIENTED_EDGE('',*,*,#5670,.T.);
#7273=ORIENTED_EDGE('',*,*,#5650,.F.);
#7274=ORIENTED_EDGE('',*,*,#5678,.F.);
#7275=ORIENTED_EDGE('',*,*,#5658,.T.);
#7276=ORIENTED_EDGE('',*,*,#5679,.T.);
#7277=ORIENTED_EDGE('',*,*,#5659,.T.);
#7278=ORIENTED_EDGE('',*,*,#5678,.T.);
#7279=ORIENTED_EDGE('',*,*,#5680,.F.);
#7280=ORIENTED_EDGE('',*,*,#5681,.F.);
#7281=ORIENTED_EDGE('',*,*,#5682,.T.);
#7282=ORIENTED_EDGE('',*,*,#5683,.F.);
#7283=ORIENTED_EDGE('',*,*,#5684,.T.);
#7284=ORIENTED_EDGE('',*,*,#5685,.T.);
#7285=ORIENTED_EDGE('',*,*,#5672,.F.);
#7286=ORIENTED_EDGE('',*,*,#5661,.F.);
#7287=ORIENTED_EDGE('',*,*,#5669,.T.);
#7288=ORIENTED_EDGE('',*,*,#5686,.F.);
#7289=ORIENTED_EDGE('',*,*,#5687,.F.);
#7290=ORIENTED_EDGE('',*,*,#5688,.T.);
#7291=ORIENTED_EDGE('',*,*,#5676,.T.);
#7292=ORIENTED_EDGE('',*,*,#5682,.F.);
#7293=ORIENTED_EDGE('',*,*,#5689,.T.);
#7294=ORIENTED_EDGE('',*,*,#5683,.T.);
#7295=ORIENTED_EDGE('',*,*,#5660,.F.);
#7296=ORIENTED_EDGE('',*,*,#5675,.F.);
#7297=ORIENTED_EDGE('',*,*,#5690,.F.);
#7298=ORIENTED_EDGE('',*,*,#5691,.T.);
#7299=ORIENTED_EDGE('',*,*,#5692,.T.);
#7300=ORIENTED_EDGE('',*,*,#5667,.F.);
#7301=ORIENTED_EDGE('',*,*,#5692,.F.);
#7302=ORIENTED_EDGE('',*,*,#5693,.T.);
#7303=ORIENTED_EDGE('',*,*,#5686,.T.);
#7304=ORIENTED_EDGE('',*,*,#5668,.F.);
#7305=ORIENTED_EDGE('',*,*,#5687,.T.);
#7306=ORIENTED_EDGE('',*,*,#5693,.F.);
#7307=ORIENTED_EDGE('',*,*,#5691,.F.);
#7308=ORIENTED_EDGE('',*,*,#5694,.T.);
#7309=ORIENTED_EDGE('',*,*,#5695,.F.);
#7310=ORIENTED_EDGE('',*,*,#5696,.F.);
#7311=ORIENTED_EDGE('',*,*,#5684,.F.);
#7312=ORIENTED_EDGE('',*,*,#5689,.F.);
#7313=ORIENTED_EDGE('',*,*,#5681,.T.);
#7314=ORIENTED_EDGE('',*,*,#5697,.F.);
#7315=ORIENTED_EDGE('',*,*,#5698,.F.);
#7316=ORIENTED_EDGE('',*,*,#5699,.T.);
#7317=ORIENTED_EDGE('',*,*,#5700,.F.);
#7318=ORIENTED_EDGE('',*,*,#5695,.T.);
#7319=ORIENTED_EDGE('',*,*,#5701,.T.);
#7320=ORIENTED_EDGE('',*,*,#5664,.F.);
#7321=ORIENTED_EDGE('',*,*,#5673,.F.);
#7322=ORIENTED_EDGE('',*,*,#5685,.F.);
#7323=ORIENTED_EDGE('',*,*,#5696,.T.);
#7324=ORIENTED_EDGE('',*,*,#5700,.T.);
#7325=ORIENTED_EDGE('',*,*,#5663,.F.);
#7326=ORIENTED_EDGE('',*,*,#5665,.T.);
#7327=ORIENTED_EDGE('',*,*,#5701,.F.);
#7328=ORIENTED_EDGE('',*,*,#5694,.F.);
#7329=ORIENTED_EDGE('',*,*,#5690,.T.);
#7330=ORIENTED_EDGE('',*,*,#5674,.T.);
#7331=ORIENTED_EDGE('',*,*,#5671,.T.);
#7332=ORIENTED_EDGE('',*,*,#5677,.T.);
#7333=ORIENTED_EDGE('',*,*,#5688,.F.);
#7334=ORIENTED_EDGE('',*,*,#5699,.F.);
#7335=ORIENTED_EDGE('',*,*,#5702,.T.);
#7336=ORIENTED_EDGE('',*,*,#5702,.F.);
#7337=ORIENTED_EDGE('',*,*,#5698,.T.);
#7338=ORIENTED_EDGE('',*,*,#5703,.T.);
#7339=ORIENTED_EDGE('',*,*,#5656,.F.);
#7340=ORIENTED_EDGE('',*,*,#5654,.F.);
#7341=ORIENTED_EDGE('',*,*,#5703,.F.);
#7342=ORIENTED_EDGE('',*,*,#5697,.T.);
#7343=ORIENTED_EDGE('',*,*,#5680,.T.);
#7344=ORIENTED_EDGE('',*,*,#5679,.F.);
#7345=ORIENTED_EDGE('',*,*,#5657,.F.);
#7346=ORIENTED_EDGE('',*,*,#5704,.T.);
#7347=ORIENTED_EDGE('',*,*,#5705,.T.);
#7348=ORIENTED_EDGE('',*,*,#5706,.T.);
#7349=ORIENTED_EDGE('',*,*,#5707,.T.);
#7350=ORIENTED_EDGE('',*,*,#5705,.F.);
#7351=ORIENTED_EDGE('',*,*,#5708,.T.);
#7352=ORIENTED_EDGE('',*,*,#5709,.T.);
#7353=ORIENTED_EDGE('',*,*,#5706,.F.);
#7354=ORIENTED_EDGE('',*,*,#5707,.F.);
#7355=ORIENTED_EDGE('',*,*,#5709,.F.);
#7356=ORIENTED_EDGE('',*,*,#5710,.T.);
#7357=ORIENTED_EDGE('',*,*,#5711,.T.);
#7358=ORIENTED_EDGE('',*,*,#5712,.F.);
#7359=ORIENTED_EDGE('',*,*,#5713,.F.);
#7360=ORIENTED_EDGE('',*,*,#5714,.T.);
#7361=ORIENTED_EDGE('',*,*,#5715,.T.);
#7362=ORIENTED_EDGE('',*,*,#5716,.F.);
#7363=ORIENTED_EDGE('',*,*,#5717,.T.);
#7364=ORIENTED_EDGE('',*,*,#5718,.T.);
#7365=ORIENTED_EDGE('',*,*,#5719,.F.);
#7366=ORIENTED_EDGE('',*,*,#5720,.F.);
#7367=ORIENTED_EDGE('',*,*,#5721,.T.);
#7368=ORIENTED_EDGE('',*,*,#5722,.T.);
#7369=ORIENTED_EDGE('',*,*,#5723,.F.);
#7370=ORIENTED_EDGE('',*,*,#5724,.F.);
#7371=ORIENTED_EDGE('',*,*,#5725,.F.);
#7372=ORIENTED_EDGE('',*,*,#5716,.T.);
#7373=ORIENTED_EDGE('',*,*,#5726,.T.);
#7374=ORIENTED_EDGE('',*,*,#5727,.T.);
#7375=ORIENTED_EDGE('',*,*,#5728,.F.);
#7376=ORIENTED_EDGE('',*,*,#5729,.T.);
#7377=ORIENTED_EDGE('',*,*,#5720,.T.);
#7378=ORIENTED_EDGE('',*,*,#5730,.F.);
#7379=ORIENTED_EDGE('',*,*,#5731,.F.);
#7380=ORIENTED_EDGE('',*,*,#5724,.T.);
#7381=ORIENTED_EDGE('',*,*,#5704,.F.);
#7382=ORIENTED_EDGE('',*,*,#5732,.F.);
#7383=ORIENTED_EDGE('',*,*,#5712,.T.);
#7384=ORIENTED_EDGE('',*,*,#5733,.T.);
#7385=ORIENTED_EDGE('',*,*,#5713,.T.);
#7386=ORIENTED_EDGE('',*,*,#5732,.T.);
#7387=ORIENTED_EDGE('',*,*,#5734,.F.);
#7388=ORIENTED_EDGE('',*,*,#5735,.F.);
#7389=ORIENTED_EDGE('',*,*,#5736,.T.);
#7390=ORIENTED_EDGE('',*,*,#5737,.F.);
#7391=ORIENTED_EDGE('',*,*,#5738,.T.);
#7392=ORIENTED_EDGE('',*,*,#5739,.T.);
#7393=ORIENTED_EDGE('',*,*,#5726,.F.);
#7394=ORIENTED_EDGE('',*,*,#5715,.F.);
#7395=ORIENTED_EDGE('',*,*,#5723,.T.);
#7396=ORIENTED_EDGE('',*,*,#5740,.F.);
#7397=ORIENTED_EDGE('',*,*,#5741,.F.);
#7398=ORIENTED_EDGE('',*,*,#5742,.T.);
#7399=ORIENTED_EDGE('',*,*,#5730,.T.);
#7400=ORIENTED_EDGE('',*,*,#5736,.F.);
#7401=ORIENTED_EDGE('',*,*,#5743,.T.);
#7402=ORIENTED_EDGE('',*,*,#5737,.T.);
#7403=ORIENTED_EDGE('',*,*,#5714,.F.);
#7404=ORIENTED_EDGE('',*,*,#5729,.F.);
#7405=ORIENTED_EDGE('',*,*,#5744,.F.);
#7406=ORIENTED_EDGE('',*,*,#5745,.T.);
#7407=ORIENTED_EDGE('',*,*,#5746,.T.);
#7408=ORIENTED_EDGE('',*,*,#5721,.F.);
#7409=ORIENTED_EDGE('',*,*,#5746,.F.);
#7410=ORIENTED_EDGE('',*,*,#5747,.T.);
#7411=ORIENTED_EDGE('',*,*,#5740,.T.);
#7412=ORIENTED_EDGE('',*,*,#5722,.F.);
#7413=ORIENTED_EDGE('',*,*,#5741,.T.);
#7414=ORIENTED_EDGE('',*,*,#5747,.F.);
#7415=ORIENTED_EDGE('',*,*,#5745,.F.);
#7416=ORIENTED_EDGE('',*,*,#5748,.T.);
#7417=ORIENTED_EDGE('',*,*,#5749,.F.);
#7418=ORIENTED_EDGE('',*,*,#5750,.F.);
#7419=ORIENTED_EDGE('',*,*,#5738,.F.);
#7420=ORIENTED_EDGE('',*,*,#5743,.F.);
#7421=ORIENTED_EDGE('',*,*,#5735,.T.);
#7422=ORIENTED_EDGE('',*,*,#5751,.F.);
#7423=ORIENTED_EDGE('',*,*,#5752,.F.);
#7424=ORIENTED_EDGE('',*,*,#5753,.T.);
#7425=ORIENTED_EDGE('',*,*,#5754,.F.);
#7426=ORIENTED_EDGE('',*,*,#5749,.T.);
#7427=ORIENTED_EDGE('',*,*,#5755,.T.);
#7428=ORIENTED_EDGE('',*,*,#5718,.F.);
#7429=ORIENTED_EDGE('',*,*,#5727,.F.);
#7430=ORIENTED_EDGE('',*,*,#5739,.F.);
#7431=ORIENTED_EDGE('',*,*,#5750,.T.);
#7432=ORIENTED_EDGE('',*,*,#5754,.T.);
#7433=ORIENTED_EDGE('',*,*,#5717,.F.);
#7434=ORIENTED_EDGE('',*,*,#5719,.T.);
#7435=ORIENTED_EDGE('',*,*,#5755,.F.);
#7436=ORIENTED_EDGE('',*,*,#5748,.F.);
#7437=ORIENTED_EDGE('',*,*,#5744,.T.);
#7438=ORIENTED_EDGE('',*,*,#5728,.T.);
#7439=ORIENTED_EDGE('',*,*,#5725,.T.);
#7440=ORIENTED_EDGE('',*,*,#5731,.T.);
#7441=ORIENTED_EDGE('',*,*,#5742,.F.);
#7442=ORIENTED_EDGE('',*,*,#5753,.F.);
#7443=ORIENTED_EDGE('',*,*,#5756,.T.);
#7444=ORIENTED_EDGE('',*,*,#5756,.F.);
#7445=ORIENTED_EDGE('',*,*,#5752,.T.);
#7446=ORIENTED_EDGE('',*,*,#5757,.T.);
#7447=ORIENTED_EDGE('',*,*,#5710,.F.);
#7448=ORIENTED_EDGE('',*,*,#5708,.F.);
#7449=ORIENTED_EDGE('',*,*,#5757,.F.);
#7450=ORIENTED_EDGE('',*,*,#5751,.T.);
#7451=ORIENTED_EDGE('',*,*,#5734,.T.);
#7452=ORIENTED_EDGE('',*,*,#5733,.F.);
#7453=ORIENTED_EDGE('',*,*,#5711,.F.);
#7454=ORIENTED_EDGE('',*,*,#5758,.T.);
#7455=ORIENTED_EDGE('',*,*,#5759,.T.);
#7456=ORIENTED_EDGE('',*,*,#5760,.T.);
#7457=ORIENTED_EDGE('',*,*,#5761,.T.);
#7458=ORIENTED_EDGE('',*,*,#5759,.F.);
#7459=ORIENTED_EDGE('',*,*,#5762,.T.);
#7460=ORIENTED_EDGE('',*,*,#5763,.T.);
#7461=ORIENTED_EDGE('',*,*,#5760,.F.);
#7462=ORIENTED_EDGE('',*,*,#5761,.F.);
#7463=ORIENTED_EDGE('',*,*,#5763,.F.);
#7464=ORIENTED_EDGE('',*,*,#5764,.T.);
#7465=ORIENTED_EDGE('',*,*,#5765,.T.);
#7466=ORIENTED_EDGE('',*,*,#5766,.F.);
#7467=ORIENTED_EDGE('',*,*,#5767,.F.);
#7468=ORIENTED_EDGE('',*,*,#5768,.T.);
#7469=ORIENTED_EDGE('',*,*,#5769,.T.);
#7470=ORIENTED_EDGE('',*,*,#5770,.F.);
#7471=ORIENTED_EDGE('',*,*,#5771,.T.);
#7472=ORIENTED_EDGE('',*,*,#5772,.T.);
#7473=ORIENTED_EDGE('',*,*,#5773,.F.);
#7474=ORIENTED_EDGE('',*,*,#5774,.F.);
#7475=ORIENTED_EDGE('',*,*,#5775,.T.);
#7476=ORIENTED_EDGE('',*,*,#5776,.T.);
#7477=ORIENTED_EDGE('',*,*,#5777,.F.);
#7478=ORIENTED_EDGE('',*,*,#5778,.F.);
#7479=ORIENTED_EDGE('',*,*,#5779,.F.);
#7480=ORIENTED_EDGE('',*,*,#5770,.T.);
#7481=ORIENTED_EDGE('',*,*,#5780,.T.);
#7482=ORIENTED_EDGE('',*,*,#5781,.T.);
#7483=ORIENTED_EDGE('',*,*,#5782,.F.);
#7484=ORIENTED_EDGE('',*,*,#5783,.T.);
#7485=ORIENTED_EDGE('',*,*,#5774,.T.);
#7486=ORIENTED_EDGE('',*,*,#5784,.F.);
#7487=ORIENTED_EDGE('',*,*,#5785,.F.);
#7488=ORIENTED_EDGE('',*,*,#5778,.T.);
#7489=ORIENTED_EDGE('',*,*,#5758,.F.);
#7490=ORIENTED_EDGE('',*,*,#5786,.F.);
#7491=ORIENTED_EDGE('',*,*,#5766,.T.);
#7492=ORIENTED_EDGE('',*,*,#5787,.T.);
#7493=ORIENTED_EDGE('',*,*,#5767,.T.);
#7494=ORIENTED_EDGE('',*,*,#5786,.T.);
#7495=ORIENTED_EDGE('',*,*,#5788,.F.);
#7496=ORIENTED_EDGE('',*,*,#5789,.F.);
#7497=ORIENTED_EDGE('',*,*,#5790,.T.);
#7498=ORIENTED_EDGE('',*,*,#5791,.F.);
#7499=ORIENTED_EDGE('',*,*,#5792,.T.);
#7500=ORIENTED_EDGE('',*,*,#5793,.T.);
#7501=ORIENTED_EDGE('',*,*,#5780,.F.);
#7502=ORIENTED_EDGE('',*,*,#5769,.F.);
#7503=ORIENTED_EDGE('',*,*,#5777,.T.);
#7504=ORIENTED_EDGE('',*,*,#5794,.F.);
#7505=ORIENTED_EDGE('',*,*,#5795,.F.);
#7506=ORIENTED_EDGE('',*,*,#5796,.T.);
#7507=ORIENTED_EDGE('',*,*,#5784,.T.);
#7508=ORIENTED_EDGE('',*,*,#5790,.F.);
#7509=ORIENTED_EDGE('',*,*,#5797,.T.);
#7510=ORIENTED_EDGE('',*,*,#5791,.T.);
#7511=ORIENTED_EDGE('',*,*,#5768,.F.);
#7512=ORIENTED_EDGE('',*,*,#5783,.F.);
#7513=ORIENTED_EDGE('',*,*,#5798,.F.);
#7514=ORIENTED_EDGE('',*,*,#5799,.T.);
#7515=ORIENTED_EDGE('',*,*,#5800,.T.);
#7516=ORIENTED_EDGE('',*,*,#5775,.F.);
#7517=ORIENTED_EDGE('',*,*,#5800,.F.);
#7518=ORIENTED_EDGE('',*,*,#5801,.T.);
#7519=ORIENTED_EDGE('',*,*,#5794,.T.);
#7520=ORIENTED_EDGE('',*,*,#5776,.F.);
#7521=ORIENTED_EDGE('',*,*,#5795,.T.);
#7522=ORIENTED_EDGE('',*,*,#5801,.F.);
#7523=ORIENTED_EDGE('',*,*,#5799,.F.);
#7524=ORIENTED_EDGE('',*,*,#5802,.T.);
#7525=ORIENTED_EDGE('',*,*,#5803,.F.);
#7526=ORIENTED_EDGE('',*,*,#5804,.F.);
#7527=ORIENTED_EDGE('',*,*,#5792,.F.);
#7528=ORIENTED_EDGE('',*,*,#5797,.F.);
#7529=ORIENTED_EDGE('',*,*,#5789,.T.);
#7530=ORIENTED_EDGE('',*,*,#5805,.F.);
#7531=ORIENTED_EDGE('',*,*,#5806,.F.);
#7532=ORIENTED_EDGE('',*,*,#5807,.T.);
#7533=ORIENTED_EDGE('',*,*,#5808,.F.);
#7534=ORIENTED_EDGE('',*,*,#5803,.T.);
#7535=ORIENTED_EDGE('',*,*,#5809,.T.);
#7536=ORIENTED_EDGE('',*,*,#5772,.F.);
#7537=ORIENTED_EDGE('',*,*,#5781,.F.);
#7538=ORIENTED_EDGE('',*,*,#5793,.F.);
#7539=ORIENTED_EDGE('',*,*,#5804,.T.);
#7540=ORIENTED_EDGE('',*,*,#5808,.T.);
#7541=ORIENTED_EDGE('',*,*,#5771,.F.);
#7542=ORIENTED_EDGE('',*,*,#5773,.T.);
#7543=ORIENTED_EDGE('',*,*,#5809,.F.);
#7544=ORIENTED_EDGE('',*,*,#5802,.F.);
#7545=ORIENTED_EDGE('',*,*,#5798,.T.);
#7546=ORIENTED_EDGE('',*,*,#5782,.T.);
#7547=ORIENTED_EDGE('',*,*,#5779,.T.);
#7548=ORIENTED_EDGE('',*,*,#5785,.T.);
#7549=ORIENTED_EDGE('',*,*,#5796,.F.);
#7550=ORIENTED_EDGE('',*,*,#5807,.F.);
#7551=ORIENTED_EDGE('',*,*,#5810,.T.);
#7552=ORIENTED_EDGE('',*,*,#5810,.F.);
#7553=ORIENTED_EDGE('',*,*,#5806,.T.);
#7554=ORIENTED_EDGE('',*,*,#5811,.T.);
#7555=ORIENTED_EDGE('',*,*,#5764,.F.);
#7556=ORIENTED_EDGE('',*,*,#5762,.F.);
#7557=ORIENTED_EDGE('',*,*,#5811,.F.);
#7558=ORIENTED_EDGE('',*,*,#5805,.T.);
#7559=ORIENTED_EDGE('',*,*,#5788,.T.);
#7560=ORIENTED_EDGE('',*,*,#5787,.F.);
#7561=ORIENTED_EDGE('',*,*,#5765,.F.);
#7562=ORIENTED_EDGE('',*,*,#5812,.T.);
#7563=ORIENTED_EDGE('',*,*,#5813,.T.);
#7564=ORIENTED_EDGE('',*,*,#5814,.T.);
#7565=ORIENTED_EDGE('',*,*,#5815,.T.);
#7566=ORIENTED_EDGE('',*,*,#5813,.F.);
#7567=ORIENTED_EDGE('',*,*,#5816,.T.);
#7568=ORIENTED_EDGE('',*,*,#5817,.T.);
#7569=ORIENTED_EDGE('',*,*,#5814,.F.);
#7570=ORIENTED_EDGE('',*,*,#5815,.F.);
#7571=ORIENTED_EDGE('',*,*,#5817,.F.);
#7572=ORIENTED_EDGE('',*,*,#5818,.T.);
#7573=ORIENTED_EDGE('',*,*,#5819,.T.);
#7574=ORIENTED_EDGE('',*,*,#5820,.F.);
#7575=ORIENTED_EDGE('',*,*,#5821,.F.);
#7576=ORIENTED_EDGE('',*,*,#5822,.T.);
#7577=ORIENTED_EDGE('',*,*,#5823,.T.);
#7578=ORIENTED_EDGE('',*,*,#5824,.F.);
#7579=ORIENTED_EDGE('',*,*,#5825,.T.);
#7580=ORIENTED_EDGE('',*,*,#5826,.T.);
#7581=ORIENTED_EDGE('',*,*,#5827,.F.);
#7582=ORIENTED_EDGE('',*,*,#5828,.F.);
#7583=ORIENTED_EDGE('',*,*,#5829,.T.);
#7584=ORIENTED_EDGE('',*,*,#5830,.T.);
#7585=ORIENTED_EDGE('',*,*,#5831,.F.);
#7586=ORIENTED_EDGE('',*,*,#5832,.F.);
#7587=ORIENTED_EDGE('',*,*,#5833,.F.);
#7588=ORIENTED_EDGE('',*,*,#5824,.T.);
#7589=ORIENTED_EDGE('',*,*,#5834,.T.);
#7590=ORIENTED_EDGE('',*,*,#5835,.T.);
#7591=ORIENTED_EDGE('',*,*,#5836,.F.);
#7592=ORIENTED_EDGE('',*,*,#5837,.T.);
#7593=ORIENTED_EDGE('',*,*,#5828,.T.);
#7594=ORIENTED_EDGE('',*,*,#5838,.F.);
#7595=ORIENTED_EDGE('',*,*,#5839,.F.);
#7596=ORIENTED_EDGE('',*,*,#5832,.T.);
#7597=ORIENTED_EDGE('',*,*,#5812,.F.);
#7598=ORIENTED_EDGE('',*,*,#5840,.F.);
#7599=ORIENTED_EDGE('',*,*,#5820,.T.);
#7600=ORIENTED_EDGE('',*,*,#5841,.T.);
#7601=ORIENTED_EDGE('',*,*,#5821,.T.);
#7602=ORIENTED_EDGE('',*,*,#5840,.T.);
#7603=ORIENTED_EDGE('',*,*,#5842,.F.);
#7604=ORIENTED_EDGE('',*,*,#5843,.F.);
#7605=ORIENTED_EDGE('',*,*,#5844,.T.);
#7606=ORIENTED_EDGE('',*,*,#5845,.F.);
#7607=ORIENTED_EDGE('',*,*,#5846,.T.);
#7608=ORIENTED_EDGE('',*,*,#5847,.T.);
#7609=ORIENTED_EDGE('',*,*,#5834,.F.);
#7610=ORIENTED_EDGE('',*,*,#5823,.F.);
#7611=ORIENTED_EDGE('',*,*,#5831,.T.);
#7612=ORIENTED_EDGE('',*,*,#5848,.F.);
#7613=ORIENTED_EDGE('',*,*,#5849,.F.);
#7614=ORIENTED_EDGE('',*,*,#5850,.T.);
#7615=ORIENTED_EDGE('',*,*,#5838,.T.);
#7616=ORIENTED_EDGE('',*,*,#5844,.F.);
#7617=ORIENTED_EDGE('',*,*,#5851,.T.);
#7618=ORIENTED_EDGE('',*,*,#5845,.T.);
#7619=ORIENTED_EDGE('',*,*,#5822,.F.);
#7620=ORIENTED_EDGE('',*,*,#5837,.F.);
#7621=ORIENTED_EDGE('',*,*,#5852,.F.);
#7622=ORIENTED_EDGE('',*,*,#5853,.T.);
#7623=ORIENTED_EDGE('',*,*,#5854,.T.);
#7624=ORIENTED_EDGE('',*,*,#5829,.F.);
#7625=ORIENTED_EDGE('',*,*,#5854,.F.);
#7626=ORIENTED_EDGE('',*,*,#5855,.T.);
#7627=ORIENTED_EDGE('',*,*,#5848,.T.);
#7628=ORIENTED_EDGE('',*,*,#5830,.F.);
#7629=ORIENTED_EDGE('',*,*,#5849,.T.);
#7630=ORIENTED_EDGE('',*,*,#5855,.F.);
#7631=ORIENTED_EDGE('',*,*,#5853,.F.);
#7632=ORIENTED_EDGE('',*,*,#5856,.T.);
#7633=ORIENTED_EDGE('',*,*,#5857,.F.);
#7634=ORIENTED_EDGE('',*,*,#5858,.F.);
#7635=ORIENTED_EDGE('',*,*,#5846,.F.);
#7636=ORIENTED_EDGE('',*,*,#5851,.F.);
#7637=ORIENTED_EDGE('',*,*,#5843,.T.);
#7638=ORIENTED_EDGE('',*,*,#5859,.F.);
#7639=ORIENTED_EDGE('',*,*,#5860,.F.);
#7640=ORIENTED_EDGE('',*,*,#5861,.T.);
#7641=ORIENTED_EDGE('',*,*,#5862,.F.);
#7642=ORIENTED_EDGE('',*,*,#5857,.T.);
#7643=ORIENTED_EDGE('',*,*,#5863,.T.);
#7644=ORIENTED_EDGE('',*,*,#5826,.F.);
#7645=ORIENTED_EDGE('',*,*,#5835,.F.);
#7646=ORIENTED_EDGE('',*,*,#5847,.F.);
#7647=ORIENTED_EDGE('',*,*,#5858,.T.);
#7648=ORIENTED_EDGE('',*,*,#5862,.T.);
#7649=ORIENTED_EDGE('',*,*,#5825,.F.);
#7650=ORIENTED_EDGE('',*,*,#5827,.T.);
#7651=ORIENTED_EDGE('',*,*,#5863,.F.);
#7652=ORIENTED_EDGE('',*,*,#5856,.F.);
#7653=ORIENTED_EDGE('',*,*,#5852,.T.);
#7654=ORIENTED_EDGE('',*,*,#5836,.T.);
#7655=ORIENTED_EDGE('',*,*,#5833,.T.);
#7656=ORIENTED_EDGE('',*,*,#5839,.T.);
#7657=ORIENTED_EDGE('',*,*,#5850,.F.);
#7658=ORIENTED_EDGE('',*,*,#5861,.F.);
#7659=ORIENTED_EDGE('',*,*,#5864,.T.);
#7660=ORIENTED_EDGE('',*,*,#5864,.F.);
#7661=ORIENTED_EDGE('',*,*,#5860,.T.);
#7662=ORIENTED_EDGE('',*,*,#5865,.T.);
#7663=ORIENTED_EDGE('',*,*,#5818,.F.);
#7664=ORIENTED_EDGE('',*,*,#5816,.F.);
#7665=ORIENTED_EDGE('',*,*,#5865,.F.);
#7666=ORIENTED_EDGE('',*,*,#5859,.T.);
#7667=ORIENTED_EDGE('',*,*,#5842,.T.);
#7668=ORIENTED_EDGE('',*,*,#5841,.F.);
#7669=ORIENTED_EDGE('',*,*,#5819,.F.);
#7670=ORIENTED_EDGE('',*,*,#5866,.F.);
#7671=ORIENTED_EDGE('',*,*,#5867,.T.);
#7672=ORIENTED_EDGE('',*,*,#5868,.T.);
#7673=ORIENTED_EDGE('',*,*,#5869,.T.);
#7674=ORIENTED_EDGE('',*,*,#5870,.F.);
#7675=ORIENTED_EDGE('',*,*,#5871,.T.);
#7676=ORIENTED_EDGE('',*,*,#5866,.T.);
#7677=ORIENTED_EDGE('',*,*,#5872,.T.);
#7678=ORIENTED_EDGE('',*,*,#5873,.F.);
#7679=ORIENTED_EDGE('',*,*,#5874,.T.);
#7680=ORIENTED_EDGE('',*,*,#5870,.T.);
#7681=ORIENTED_EDGE('',*,*,#5875,.T.);
#7682=ORIENTED_EDGE('',*,*,#5876,.F.);
#7683=ORIENTED_EDGE('',*,*,#5877,.T.);
#7684=ORIENTED_EDGE('',*,*,#5873,.T.);
#7685=ORIENTED_EDGE('',*,*,#5878,.T.);
#7686=ORIENTED_EDGE('',*,*,#5879,.F.);
#7687=ORIENTED_EDGE('',*,*,#5880,.T.);
#7688=ORIENTED_EDGE('',*,*,#5876,.T.);
#7689=ORIENTED_EDGE('',*,*,#5881,.T.);
#7690=ORIENTED_EDGE('',*,*,#5882,.F.);
#7691=ORIENTED_EDGE('',*,*,#5883,.T.);
#7692=ORIENTED_EDGE('',*,*,#5879,.T.);
#7693=ORIENTED_EDGE('',*,*,#5884,.T.);
#7694=ORIENTED_EDGE('',*,*,#5885,.F.);
#7695=ORIENTED_EDGE('',*,*,#5886,.T.);
#7696=ORIENTED_EDGE('',*,*,#5882,.T.);
#7697=ORIENTED_EDGE('',*,*,#5887,.T.);
#7698=ORIENTED_EDGE('',*,*,#5888,.F.);
#7699=ORIENTED_EDGE('',*,*,#5889,.T.);
#7700=ORIENTED_EDGE('',*,*,#5885,.T.);
#7701=ORIENTED_EDGE('',*,*,#5890,.T.);
#7702=ORIENTED_EDGE('',*,*,#5891,.F.);
#7703=ORIENTED_EDGE('',*,*,#5892,.T.);
#7704=ORIENTED_EDGE('',*,*,#5888,.T.);
#7705=ORIENTED_EDGE('',*,*,#5893,.T.);
#7706=ORIENTED_EDGE('',*,*,#5894,.F.);
#7707=ORIENTED_EDGE('',*,*,#5895,.T.);
#7708=ORIENTED_EDGE('',*,*,#5891,.T.);
#7709=ORIENTED_EDGE('',*,*,#5896,.T.);
#7710=ORIENTED_EDGE('',*,*,#5897,.F.);
#7711=ORIENTED_EDGE('',*,*,#5898,.T.);
#7712=ORIENTED_EDGE('',*,*,#5894,.T.);
#7713=ORIENTED_EDGE('',*,*,#5899,.T.);
#7714=ORIENTED_EDGE('',*,*,#5900,.F.);
#7715=ORIENTED_EDGE('',*,*,#5901,.T.);
#7716=ORIENTED_EDGE('',*,*,#5897,.T.);
#7717=ORIENTED_EDGE('',*,*,#5902,.T.);
#7718=ORIENTED_EDGE('',*,*,#5903,.F.);
#7719=ORIENTED_EDGE('',*,*,#5904,.T.);
#7720=ORIENTED_EDGE('',*,*,#5900,.T.);
#7721=ORIENTED_EDGE('',*,*,#5905,.T.);
#7722=ORIENTED_EDGE('',*,*,#5906,.F.);
#7723=ORIENTED_EDGE('',*,*,#5907,.T.);
#7724=ORIENTED_EDGE('',*,*,#5903,.T.);
#7725=ORIENTED_EDGE('',*,*,#5908,.T.);
#7726=ORIENTED_EDGE('',*,*,#5909,.F.);
#7727=ORIENTED_EDGE('',*,*,#5910,.T.);
#7728=ORIENTED_EDGE('',*,*,#5906,.T.);
#7729=ORIENTED_EDGE('',*,*,#5911,.T.);
#7730=ORIENTED_EDGE('',*,*,#5912,.F.);
#7731=ORIENTED_EDGE('',*,*,#5913,.T.);
#7732=ORIENTED_EDGE('',*,*,#5909,.T.);
#7733=ORIENTED_EDGE('',*,*,#5914,.T.);
#7734=ORIENTED_EDGE('',*,*,#5915,.F.);
#7735=ORIENTED_EDGE('',*,*,#5916,.T.);
#7736=ORIENTED_EDGE('',*,*,#5912,.T.);
#7737=ORIENTED_EDGE('',*,*,#5917,.T.);
#7738=ORIENTED_EDGE('',*,*,#5918,.F.);
#7739=ORIENTED_EDGE('',*,*,#5919,.T.);
#7740=ORIENTED_EDGE('',*,*,#5915,.T.);
#7741=ORIENTED_EDGE('',*,*,#5920,.T.);
#7742=ORIENTED_EDGE('',*,*,#5921,.F.);
#7743=ORIENTED_EDGE('',*,*,#5922,.T.);
#7744=ORIENTED_EDGE('',*,*,#5918,.T.);
#7745=ORIENTED_EDGE('',*,*,#5923,.T.);
#7746=ORIENTED_EDGE('',*,*,#5924,.F.);
#7747=ORIENTED_EDGE('',*,*,#5925,.T.);
#7748=ORIENTED_EDGE('',*,*,#5926,.T.);
#7749=ORIENTED_EDGE('',*,*,#5927,.T.);
#7750=ORIENTED_EDGE('',*,*,#5928,.F.);
#7751=ORIENTED_EDGE('',*,*,#5929,.T.);
#7752=ORIENTED_EDGE('',*,*,#5924,.T.);
#7753=ORIENTED_EDGE('',*,*,#5930,.T.);
#7754=ORIENTED_EDGE('',*,*,#5931,.F.);
#7755=ORIENTED_EDGE('',*,*,#5932,.T.);
#7756=ORIENTED_EDGE('',*,*,#5928,.T.);
#7757=ORIENTED_EDGE('',*,*,#5933,.T.);
#7758=ORIENTED_EDGE('',*,*,#5934,.F.);
#7759=ORIENTED_EDGE('',*,*,#5935,.T.);
#7760=ORIENTED_EDGE('',*,*,#5931,.T.);
#7761=ORIENTED_EDGE('',*,*,#5936,.T.);
#7762=ORIENTED_EDGE('',*,*,#5937,.F.);
#7763=ORIENTED_EDGE('',*,*,#5938,.T.);
#7764=ORIENTED_EDGE('',*,*,#5934,.T.);
#7765=ORIENTED_EDGE('',*,*,#5939,.T.);
#7766=ORIENTED_EDGE('',*,*,#5940,.F.);
#7767=ORIENTED_EDGE('',*,*,#5941,.T.);
#7768=ORIENTED_EDGE('',*,*,#5937,.T.);
#7769=ORIENTED_EDGE('',*,*,#5942,.T.);
#7770=ORIENTED_EDGE('',*,*,#5943,.F.);
#7771=ORIENTED_EDGE('',*,*,#5944,.T.);
#7772=ORIENTED_EDGE('',*,*,#5940,.T.);
#7773=ORIENTED_EDGE('',*,*,#5945,.T.);
#7774=ORIENTED_EDGE('',*,*,#5946,.F.);
#7775=ORIENTED_EDGE('',*,*,#5947,.T.);
#7776=ORIENTED_EDGE('',*,*,#5943,.T.);
#7777=ORIENTED_EDGE('',*,*,#5948,.T.);
#7778=ORIENTED_EDGE('',*,*,#5949,.F.);
#7779=ORIENTED_EDGE('',*,*,#5950,.T.);
#7780=ORIENTED_EDGE('',*,*,#5946,.T.);
#7781=ORIENTED_EDGE('',*,*,#5951,.T.);
#7782=ORIENTED_EDGE('',*,*,#5952,.F.);
#7783=ORIENTED_EDGE('',*,*,#5953,.T.);
#7784=ORIENTED_EDGE('',*,*,#5949,.T.);
#7785=ORIENTED_EDGE('',*,*,#5954,.T.);
#7786=ORIENTED_EDGE('',*,*,#5955,.F.);
#7787=ORIENTED_EDGE('',*,*,#5956,.T.);
#7788=ORIENTED_EDGE('',*,*,#5952,.T.);
#7789=ORIENTED_EDGE('',*,*,#5957,.T.);
#7790=ORIENTED_EDGE('',*,*,#5958,.F.);
#7791=ORIENTED_EDGE('',*,*,#5959,.T.);
#7792=ORIENTED_EDGE('',*,*,#5955,.T.);
#7793=ORIENTED_EDGE('',*,*,#5960,.T.);
#7794=ORIENTED_EDGE('',*,*,#5961,.F.);
#7795=ORIENTED_EDGE('',*,*,#5962,.T.);
#7796=ORIENTED_EDGE('',*,*,#5958,.T.);
#7797=ORIENTED_EDGE('',*,*,#5963,.T.);
#7798=ORIENTED_EDGE('',*,*,#5964,.F.);
#7799=ORIENTED_EDGE('',*,*,#5965,.T.);
#7800=ORIENTED_EDGE('',*,*,#5961,.T.);
#7801=ORIENTED_EDGE('',*,*,#5966,.T.);
#7802=ORIENTED_EDGE('',*,*,#5967,.F.);
#7803=ORIENTED_EDGE('',*,*,#5968,.T.);
#7804=ORIENTED_EDGE('',*,*,#5964,.T.);
#7805=ORIENTED_EDGE('',*,*,#5969,.T.);
#7806=ORIENTED_EDGE('',*,*,#5970,.F.);
#7807=ORIENTED_EDGE('',*,*,#5971,.T.);
#7808=ORIENTED_EDGE('',*,*,#5967,.T.);
#7809=ORIENTED_EDGE('',*,*,#5972,.T.);
#7810=ORIENTED_EDGE('',*,*,#5973,.F.);
#7811=ORIENTED_EDGE('',*,*,#5974,.T.);
#7812=ORIENTED_EDGE('',*,*,#5970,.T.);
#7813=ORIENTED_EDGE('',*,*,#5975,.T.);
#7814=ORIENTED_EDGE('',*,*,#5976,.F.);
#7815=ORIENTED_EDGE('',*,*,#5977,.T.);
#7816=ORIENTED_EDGE('',*,*,#5973,.T.);
#7817=ORIENTED_EDGE('',*,*,#5978,.T.);
#7818=ORIENTED_EDGE('',*,*,#5979,.F.);
#7819=ORIENTED_EDGE('',*,*,#5980,.T.);
#7820=ORIENTED_EDGE('',*,*,#5976,.T.);
#7821=ORIENTED_EDGE('',*,*,#5981,.T.);
#7822=ORIENTED_EDGE('',*,*,#5982,.F.);
#7823=ORIENTED_EDGE('',*,*,#5983,.T.);
#7824=ORIENTED_EDGE('',*,*,#5984,.T.);
#7825=ORIENTED_EDGE('',*,*,#5985,.F.);
#7826=ORIENTED_EDGE('',*,*,#5986,.T.);
#7827=ORIENTED_EDGE('',*,*,#5982,.T.);
#7828=ORIENTED_EDGE('',*,*,#5987,.T.);
#7829=ORIENTED_EDGE('',*,*,#5988,.F.);
#7830=ORIENTED_EDGE('',*,*,#5989,.T.);
#7831=ORIENTED_EDGE('',*,*,#5985,.T.);
#7832=ORIENTED_EDGE('',*,*,#5990,.T.);
#7833=ORIENTED_EDGE('',*,*,#5991,.F.);
#7834=ORIENTED_EDGE('',*,*,#5992,.T.);
#7835=ORIENTED_EDGE('',*,*,#5988,.T.);
#7836=ORIENTED_EDGE('',*,*,#5993,.T.);
#7837=ORIENTED_EDGE('',*,*,#5994,.F.);
#7838=ORIENTED_EDGE('',*,*,#5995,.T.);
#7839=ORIENTED_EDGE('',*,*,#5991,.T.);
#7840=ORIENTED_EDGE('',*,*,#5996,.T.);
#7841=ORIENTED_EDGE('',*,*,#5997,.F.);
#7842=ORIENTED_EDGE('',*,*,#5998,.T.);
#7843=ORIENTED_EDGE('',*,*,#5994,.T.);
#7844=ORIENTED_EDGE('',*,*,#5999,.T.);
#7845=ORIENTED_EDGE('',*,*,#6000,.F.);
#7846=ORIENTED_EDGE('',*,*,#6001,.T.);
#7847=ORIENTED_EDGE('',*,*,#5997,.T.);
#7848=ORIENTED_EDGE('',*,*,#6002,.T.);
#7849=ORIENTED_EDGE('',*,*,#6003,.F.);
#7850=ORIENTED_EDGE('',*,*,#6004,.T.);
#7851=ORIENTED_EDGE('',*,*,#6000,.T.);
#7852=ORIENTED_EDGE('',*,*,#6005,.T.);
#7853=ORIENTED_EDGE('',*,*,#6006,.F.);
#7854=ORIENTED_EDGE('',*,*,#6007,.T.);
#7855=ORIENTED_EDGE('',*,*,#6003,.T.);
#7856=ORIENTED_EDGE('',*,*,#6008,.T.);
#7857=ORIENTED_EDGE('',*,*,#6009,.F.);
#7858=ORIENTED_EDGE('',*,*,#6010,.T.);
#7859=ORIENTED_EDGE('',*,*,#6006,.T.);
#7860=ORIENTED_EDGE('',*,*,#6011,.T.);
#7861=ORIENTED_EDGE('',*,*,#6012,.F.);
#7862=ORIENTED_EDGE('',*,*,#6013,.T.);
#7863=ORIENTED_EDGE('',*,*,#6009,.T.);
#7864=ORIENTED_EDGE('',*,*,#6014,.T.);
#7865=ORIENTED_EDGE('',*,*,#6015,.F.);
#7866=ORIENTED_EDGE('',*,*,#6016,.T.);
#7867=ORIENTED_EDGE('',*,*,#6012,.T.);
#7868=ORIENTED_EDGE('',*,*,#6017,.T.);
#7869=ORIENTED_EDGE('',*,*,#6018,.F.);
#7870=ORIENTED_EDGE('',*,*,#6019,.T.);
#7871=ORIENTED_EDGE('',*,*,#6015,.T.);
#7872=ORIENTED_EDGE('',*,*,#6020,.T.);
#7873=ORIENTED_EDGE('',*,*,#6021,.F.);
#7874=ORIENTED_EDGE('',*,*,#6022,.T.);
#7875=ORIENTED_EDGE('',*,*,#6018,.T.);
#7876=ORIENTED_EDGE('',*,*,#6023,.T.);
#7877=ORIENTED_EDGE('',*,*,#6024,.F.);
#7878=ORIENTED_EDGE('',*,*,#6025,.T.);
#7879=ORIENTED_EDGE('',*,*,#6021,.T.);
#7880=ORIENTED_EDGE('',*,*,#6026,.T.);
#7881=ORIENTED_EDGE('',*,*,#6027,.F.);
#7882=ORIENTED_EDGE('',*,*,#6028,.T.);
#7883=ORIENTED_EDGE('',*,*,#6024,.T.);
#7884=ORIENTED_EDGE('',*,*,#6029,.T.);
#7885=ORIENTED_EDGE('',*,*,#6030,.F.);
#7886=ORIENTED_EDGE('',*,*,#6031,.T.);
#7887=ORIENTED_EDGE('',*,*,#6027,.T.);
#7888=ORIENTED_EDGE('',*,*,#6032,.T.);
#7889=ORIENTED_EDGE('',*,*,#6033,.F.);
#7890=ORIENTED_EDGE('',*,*,#6034,.T.);
#7891=ORIENTED_EDGE('',*,*,#6030,.T.);
#7892=ORIENTED_EDGE('',*,*,#6035,.T.);
#7893=ORIENTED_EDGE('',*,*,#6036,.F.);
#7894=ORIENTED_EDGE('',*,*,#6037,.T.);
#7895=ORIENTED_EDGE('',*,*,#6033,.T.);
#7896=ORIENTED_EDGE('',*,*,#6038,.T.);
#7897=ORIENTED_EDGE('',*,*,#6039,.F.);
#7898=ORIENTED_EDGE('',*,*,#6040,.T.);
#7899=ORIENTED_EDGE('',*,*,#6041,.T.);
#7900=ORIENTED_EDGE('',*,*,#6042,.T.);
#7901=ORIENTED_EDGE('',*,*,#6043,.F.);
#7902=ORIENTED_EDGE('',*,*,#6044,.T.);
#7903=ORIENTED_EDGE('',*,*,#6039,.T.);
#7904=ORIENTED_EDGE('',*,*,#6045,.T.);
#7905=ORIENTED_EDGE('',*,*,#6046,.F.);
#7906=ORIENTED_EDGE('',*,*,#6047,.T.);
#7907=ORIENTED_EDGE('',*,*,#6043,.T.);
#7908=ORIENTED_EDGE('',*,*,#6048,.T.);
#7909=ORIENTED_EDGE('',*,*,#6049,.F.);
#7910=ORIENTED_EDGE('',*,*,#6050,.T.);
#7911=ORIENTED_EDGE('',*,*,#6046,.T.);
#7912=ORIENTED_EDGE('',*,*,#6051,.T.);
#7913=ORIENTED_EDGE('',*,*,#6052,.F.);
#7914=ORIENTED_EDGE('',*,*,#6053,.T.);
#7915=ORIENTED_EDGE('',*,*,#6049,.T.);
#7916=ORIENTED_EDGE('',*,*,#6054,.T.);
#7917=ORIENTED_EDGE('',*,*,#6055,.F.);
#7918=ORIENTED_EDGE('',*,*,#6056,.T.);
#7919=ORIENTED_EDGE('',*,*,#6052,.T.);
#7920=ORIENTED_EDGE('',*,*,#6057,.T.);
#7921=ORIENTED_EDGE('',*,*,#6058,.F.);
#7922=ORIENTED_EDGE('',*,*,#6059,.T.);
#7923=ORIENTED_EDGE('',*,*,#6055,.T.);
#7924=ORIENTED_EDGE('',*,*,#6060,.T.);
#7925=ORIENTED_EDGE('',*,*,#6061,.F.);
#7926=ORIENTED_EDGE('',*,*,#6062,.T.);
#7927=ORIENTED_EDGE('',*,*,#6058,.T.);
#7928=ORIENTED_EDGE('',*,*,#6063,.T.);
#7929=ORIENTED_EDGE('',*,*,#6064,.F.);
#7930=ORIENTED_EDGE('',*,*,#6065,.T.);
#7931=ORIENTED_EDGE('',*,*,#6061,.T.);
#7932=ORIENTED_EDGE('',*,*,#6066,.T.);
#7933=ORIENTED_EDGE('',*,*,#6067,.F.);
#7934=ORIENTED_EDGE('',*,*,#6068,.T.);
#7935=ORIENTED_EDGE('',*,*,#6064,.T.);
#7936=ORIENTED_EDGE('',*,*,#6069,.T.);
#7937=ORIENTED_EDGE('',*,*,#6070,.F.);
#7938=ORIENTED_EDGE('',*,*,#6071,.T.);
#7939=ORIENTED_EDGE('',*,*,#6067,.T.);
#7940=ORIENTED_EDGE('',*,*,#6072,.T.);
#7941=ORIENTED_EDGE('',*,*,#6073,.F.);
#7942=ORIENTED_EDGE('',*,*,#6074,.T.);
#7943=ORIENTED_EDGE('',*,*,#6070,.T.);
#7944=ORIENTED_EDGE('',*,*,#6075,.T.);
#7945=ORIENTED_EDGE('',*,*,#6076,.F.);
#7946=ORIENTED_EDGE('',*,*,#6077,.T.);
#7947=ORIENTED_EDGE('',*,*,#6073,.T.);
#7948=ORIENTED_EDGE('',*,*,#6078,.T.);
#7949=ORIENTED_EDGE('',*,*,#6079,.F.);
#7950=ORIENTED_EDGE('',*,*,#6080,.T.);
#7951=ORIENTED_EDGE('',*,*,#6076,.T.);
#7952=ORIENTED_EDGE('',*,*,#6081,.T.);
#7953=ORIENTED_EDGE('',*,*,#6082,.F.);
#7954=ORIENTED_EDGE('',*,*,#6083,.T.);
#7955=ORIENTED_EDGE('',*,*,#6079,.T.);
#7956=ORIENTED_EDGE('',*,*,#6084,.T.);
#7957=ORIENTED_EDGE('',*,*,#6085,.F.);
#7958=ORIENTED_EDGE('',*,*,#6086,.T.);
#7959=ORIENTED_EDGE('',*,*,#6082,.T.);
#7960=ORIENTED_EDGE('',*,*,#6087,.T.);
#7961=ORIENTED_EDGE('',*,*,#6088,.F.);
#7962=ORIENTED_EDGE('',*,*,#6089,.T.);
#7963=ORIENTED_EDGE('',*,*,#6085,.T.);
#7964=ORIENTED_EDGE('',*,*,#6090,.T.);
#7965=ORIENTED_EDGE('',*,*,#6091,.F.);
#7966=ORIENTED_EDGE('',*,*,#6092,.T.);
#7967=ORIENTED_EDGE('',*,*,#6088,.T.);
#7968=ORIENTED_EDGE('',*,*,#6093,.T.);
#7969=ORIENTED_EDGE('',*,*,#6094,.T.);
#7970=ORIENTED_EDGE('',*,*,#6095,.F.);
#7971=ORIENTED_EDGE('',*,*,#6096,.T.);
#7972=ORIENTED_EDGE('',*,*,#6097,.T.);
#7973=ORIENTED_EDGE('',*,*,#6098,.F.);
#7974=ORIENTED_EDGE('',*,*,#6099,.F.);
#7975=ORIENTED_EDGE('',*,*,#6094,.F.);
#7976=ORIENTED_EDGE('',*,*,#6100,.T.);
#7977=ORIENTED_EDGE('',*,*,#6101,.T.);
#7978=ORIENTED_EDGE('',*,*,#6102,.F.);
#7979=ORIENTED_EDGE('',*,*,#6097,.F.);
#7980=ORIENTED_EDGE('',*,*,#6103,.T.);
#7981=ORIENTED_EDGE('',*,*,#6104,.T.);
#7982=ORIENTED_EDGE('',*,*,#6105,.F.);
#7983=ORIENTED_EDGE('',*,*,#6101,.F.);
#7984=ORIENTED_EDGE('',*,*,#6106,.T.);
#7985=ORIENTED_EDGE('',*,*,#6107,.T.);
#7986=ORIENTED_EDGE('',*,*,#6108,.F.);
#7987=ORIENTED_EDGE('',*,*,#6104,.F.);
#7988=ORIENTED_EDGE('',*,*,#6109,.T.);
#7989=ORIENTED_EDGE('',*,*,#6110,.T.);
#7990=ORIENTED_EDGE('',*,*,#6111,.F.);
#7991=ORIENTED_EDGE('',*,*,#6107,.F.);
#7992=ORIENTED_EDGE('',*,*,#6112,.T.);
#7993=ORIENTED_EDGE('',*,*,#6113,.F.);
#7994=ORIENTED_EDGE('',*,*,#6114,.T.);
#7995=ORIENTED_EDGE('',*,*,#6115,.F.);
#7996=ORIENTED_EDGE('',*,*,#6116,.F.);
#7997=ORIENTED_EDGE('',*,*,#6117,.T.);
#7998=ORIENTED_EDGE('',*,*,#6118,.F.);
#7999=ORIENTED_EDGE('',*,*,#6119,.T.);
#8000=ORIENTED_EDGE('',*,*,#6120,.T.);
#8001=ORIENTED_EDGE('',*,*,#6121,.F.);
#8002=ORIENTED_EDGE('',*,*,#6122,.F.);
#8003=ORIENTED_EDGE('',*,*,#6117,.F.);
#8004=ORIENTED_EDGE('',*,*,#6123,.T.);
#8005=ORIENTED_EDGE('',*,*,#6124,.T.);
#8006=ORIENTED_EDGE('',*,*,#6125,.F.);
#8007=ORIENTED_EDGE('',*,*,#6120,.F.);
#8008=ORIENTED_EDGE('',*,*,#6126,.T.);
#8009=ORIENTED_EDGE('',*,*,#6127,.T.);
#8010=ORIENTED_EDGE('',*,*,#6128,.F.);
#8011=ORIENTED_EDGE('',*,*,#6124,.F.);
#8012=ORIENTED_EDGE('',*,*,#6129,.T.);
#8013=ORIENTED_EDGE('',*,*,#6130,.T.);
#8014=ORIENTED_EDGE('',*,*,#6131,.F.);
#8015=ORIENTED_EDGE('',*,*,#6127,.F.);
#8016=ORIENTED_EDGE('',*,*,#6132,.T.);
#8017=ORIENTED_EDGE('',*,*,#6133,.T.);
#8018=ORIENTED_EDGE('',*,*,#6134,.F.);
#8019=ORIENTED_EDGE('',*,*,#6130,.F.);
#8020=ORIENTED_EDGE('',*,*,#6135,.T.);
#8021=ORIENTED_EDGE('',*,*,#6136,.F.);
#8022=ORIENTED_EDGE('',*,*,#6137,.T.);
#8023=ORIENTED_EDGE('',*,*,#6138,.F.);
#8024=ORIENTED_EDGE('',*,*,#6139,.F.);
#8025=ORIENTED_EDGE('',*,*,#6140,.T.);
#8026=ORIENTED_EDGE('',*,*,#6141,.F.);
#8027=ORIENTED_EDGE('',*,*,#6142,.T.);
#8028=ORIENTED_EDGE('',*,*,#6143,.T.);
#8029=ORIENTED_EDGE('',*,*,#6144,.F.);
#8030=ORIENTED_EDGE('',*,*,#6145,.F.);
#8031=ORIENTED_EDGE('',*,*,#6140,.F.);
#8032=ORIENTED_EDGE('',*,*,#6146,.T.);
#8033=ORIENTED_EDGE('',*,*,#6147,.T.);
#8034=ORIENTED_EDGE('',*,*,#6148,.F.);
#8035=ORIENTED_EDGE('',*,*,#6143,.F.);
#8036=ORIENTED_EDGE('',*,*,#6149,.T.);
#8037=ORIENTED_EDGE('',*,*,#6150,.T.);
#8038=ORIENTED_EDGE('',*,*,#6151,.F.);
#8039=ORIENTED_EDGE('',*,*,#6147,.F.);
#8040=ORIENTED_EDGE('',*,*,#6152,.T.);
#8041=ORIENTED_EDGE('',*,*,#6153,.T.);
#8042=ORIENTED_EDGE('',*,*,#6154,.F.);
#8043=ORIENTED_EDGE('',*,*,#6150,.F.);
#8044=ORIENTED_EDGE('',*,*,#6155,.T.);
#8045=ORIENTED_EDGE('',*,*,#6156,.T.);
#8046=ORIENTED_EDGE('',*,*,#6157,.F.);
#8047=ORIENTED_EDGE('',*,*,#6153,.F.);
#8048=ORIENTED_EDGE('',*,*,#6158,.T.);
#8049=ORIENTED_EDGE('',*,*,#6159,.F.);
#8050=ORIENTED_EDGE('',*,*,#6160,.T.);
#8051=ORIENTED_EDGE('',*,*,#6161,.F.);
#8052=ORIENTED_EDGE('',*,*,#6162,.F.);
#8053=ORIENTED_EDGE('',*,*,#6163,.T.);
#8054=ORIENTED_EDGE('',*,*,#6164,.F.);
#8055=ORIENTED_EDGE('',*,*,#6165,.T.);
#8056=ORIENTED_EDGE('',*,*,#6166,.T.);
#8057=ORIENTED_EDGE('',*,*,#6167,.F.);
#8058=ORIENTED_EDGE('',*,*,#6168,.F.);
#8059=ORIENTED_EDGE('',*,*,#6163,.F.);
#8060=ORIENTED_EDGE('',*,*,#6169,.T.);
#8061=ORIENTED_EDGE('',*,*,#6170,.T.);
#8062=ORIENTED_EDGE('',*,*,#6171,.F.);
#8063=ORIENTED_EDGE('',*,*,#6166,.F.);
#8064=ORIENTED_EDGE('',*,*,#6172,.T.);
#8065=ORIENTED_EDGE('',*,*,#6173,.T.);
#8066=ORIENTED_EDGE('',*,*,#6174,.F.);
#8067=ORIENTED_EDGE('',*,*,#6170,.F.);
#8068=ORIENTED_EDGE('',*,*,#6175,.T.);
#8069=ORIENTED_EDGE('',*,*,#6176,.T.);
#8070=ORIENTED_EDGE('',*,*,#6177,.F.);
#8071=ORIENTED_EDGE('',*,*,#6173,.F.);
#8072=ORIENTED_EDGE('',*,*,#6178,.T.);
#8073=ORIENTED_EDGE('',*,*,#6179,.T.);
#8074=ORIENTED_EDGE('',*,*,#6180,.F.);
#8075=ORIENTED_EDGE('',*,*,#6176,.F.);
#8076=ORIENTED_EDGE('',*,*,#6181,.T.);
#8077=ORIENTED_EDGE('',*,*,#6182,.F.);
#8078=ORIENTED_EDGE('',*,*,#6183,.T.);
#8079=ORIENTED_EDGE('',*,*,#6184,.F.);
#8080=ORIENTED_EDGE('',*,*,#6185,.F.);
#8081=ORIENTED_EDGE('',*,*,#6182,.T.);
#8082=ORIENTED_EDGE('',*,*,#6186,.F.);
#8083=ORIENTED_EDGE('',*,*,#6179,.F.);
#8084=ORIENTED_EDGE('',*,*,#6187,.T.);
#8085=ORIENTED_EDGE('',*,*,#6159,.T.);
#8086=ORIENTED_EDGE('',*,*,#6188,.F.);
#8087=ORIENTED_EDGE('',*,*,#6156,.F.);
#8088=ORIENTED_EDGE('',*,*,#6189,.T.);
#8089=ORIENTED_EDGE('',*,*,#6136,.T.);
#8090=ORIENTED_EDGE('',*,*,#6190,.F.);
#8091=ORIENTED_EDGE('',*,*,#6133,.F.);
#8092=ORIENTED_EDGE('',*,*,#6191,.T.);
#8093=ORIENTED_EDGE('',*,*,#6113,.T.);
#8094=ORIENTED_EDGE('',*,*,#6192,.F.);
#8095=ORIENTED_EDGE('',*,*,#6110,.F.);
#8096=ORIENTED_EDGE('',*,*,#6193,.T.);
#8097=ORIENTED_EDGE('',*,*,#6091,.T.);
#8098=ORIENTED_EDGE('',*,*,#6194,.T.);
#8099=ORIENTED_EDGE('',*,*,#6195,.F.);
#8100=ORIENTED_EDGE('',*,*,#6196,.T.);
#8101=ORIENTED_EDGE('',*,*,#6036,.T.);
#8102=ORIENTED_EDGE('',*,*,#6197,.T.);
#8103=ORIENTED_EDGE('',*,*,#6198,.F.);
#8104=ORIENTED_EDGE('',*,*,#6199,.T.);
#8105=ORIENTED_EDGE('',*,*,#5979,.T.);
#8106=ORIENTED_EDGE('',*,*,#6200,.T.);
#8107=ORIENTED_EDGE('',*,*,#6201,.F.);
#8108=ORIENTED_EDGE('',*,*,#6202,.T.);
#8109=ORIENTED_EDGE('',*,*,#5921,.T.);
#8110=ORIENTED_EDGE('',*,*,#6203,.T.);
#8111=ORIENTED_EDGE('',*,*,#6204,.F.);
#8112=ORIENTED_EDGE('',*,*,#6205,.T.);
#8113=ORIENTED_EDGE('',*,*,#6206,.F.);
#8114=ORIENTED_EDGE('',*,*,#6207,.T.);
#8115=ORIENTED_EDGE('',*,*,#6208,.F.);
#8116=ORIENTED_EDGE('',*,*,#6207,.F.);
#8117=ORIENTED_EDGE('',*,*,#6209,.F.);
#8118=ORIENTED_EDGE('',*,*,#6210,.T.);
#8119=ORIENTED_EDGE('',*,*,#6211,.T.);
#8120=ORIENTED_EDGE('',*,*,#6210,.F.);
#8121=ORIENTED_EDGE('',*,*,#6212,.F.);
#8122=ORIENTED_EDGE('',*,*,#6213,.T.);
#8123=ORIENTED_EDGE('',*,*,#6214,.F.);
#8124=ORIENTED_EDGE('',*,*,#6213,.F.);
#8125=ORIENTED_EDGE('',*,*,#6214,.T.);
#8126=ORIENTED_EDGE('',*,*,#6215,.T.);
#8127=ORIENTED_EDGE('',*,*,#6216,.F.);
#8128=ORIENTED_EDGE('',*,*,#6215,.F.);
#8129=ORIENTED_EDGE('',*,*,#6217,.F.);
#8130=ORIENTED_EDGE('',*,*,#5868,.F.);
#8131=ORIENTED_EDGE('',*,*,#6218,.F.);
#8132=ORIENTED_EDGE('',*,*,#6219,.F.);
#8133=ORIENTED_EDGE('',*,*,#6220,.F.);
#8134=ORIENTED_EDGE('',*,*,#6221,.T.);
#8135=ORIENTED_EDGE('',*,*,#6222,.F.);
#8136=ORIENTED_EDGE('',*,*,#6221,.F.);
#8137=ORIENTED_EDGE('',*,*,#6223,.F.);
#8138=ORIENTED_EDGE('',*,*,#5926,.F.);
#8139=ORIENTED_EDGE('',*,*,#6224,.F.);
#8140=ORIENTED_EDGE('',*,*,#6225,.F.);
#8141=ORIENTED_EDGE('',*,*,#6226,.F.);
#8142=ORIENTED_EDGE('',*,*,#6227,.T.);
#8143=ORIENTED_EDGE('',*,*,#6228,.F.);
#8144=ORIENTED_EDGE('',*,*,#6227,.F.);
#8145=ORIENTED_EDGE('',*,*,#6229,.F.);
#8146=ORIENTED_EDGE('',*,*,#5984,.F.);
#8147=ORIENTED_EDGE('',*,*,#6230,.F.);
#8148=ORIENTED_EDGE('',*,*,#6231,.F.);
#8149=ORIENTED_EDGE('',*,*,#6232,.F.);
#8150=ORIENTED_EDGE('',*,*,#6233,.T.);
#8151=ORIENTED_EDGE('',*,*,#6234,.F.);
#8152=ORIENTED_EDGE('',*,*,#6233,.F.);
#8153=ORIENTED_EDGE('',*,*,#6235,.F.);
#8154=ORIENTED_EDGE('',*,*,#6041,.F.);
#8155=ORIENTED_EDGE('',*,*,#6236,.F.);
#8156=ORIENTED_EDGE('',*,*,#6237,.F.);
#8157=ORIENTED_EDGE('',*,*,#6238,.F.);
#8158=ORIENTED_EDGE('',*,*,#6239,.T.);
#8159=ORIENTED_EDGE('',*,*,#6240,.F.);
#8160=ORIENTED_EDGE('',*,*,#6239,.F.);
#8161=ORIENTED_EDGE('',*,*,#6241,.F.);
#8162=ORIENTED_EDGE('',*,*,#6194,.F.);
#8163=ORIENTED_EDGE('',*,*,#6093,.F.);
#8164=ORIENTED_EDGE('',*,*,#6090,.F.);
#8165=ORIENTED_EDGE('',*,*,#6087,.F.);
#8166=ORIENTED_EDGE('',*,*,#6084,.F.);
#8167=ORIENTED_EDGE('',*,*,#6081,.F.);
#8168=ORIENTED_EDGE('',*,*,#6078,.F.);
#8169=ORIENTED_EDGE('',*,*,#6075,.F.);
#8170=ORIENTED_EDGE('',*,*,#6072,.F.);
#8171=ORIENTED_EDGE('',*,*,#6069,.F.);
#8172=ORIENTED_EDGE('',*,*,#6066,.F.);
#8173=ORIENTED_EDGE('',*,*,#6063,.F.);
#8174=ORIENTED_EDGE('',*,*,#6060,.F.);
#8175=ORIENTED_EDGE('',*,*,#6057,.F.);
#8176=ORIENTED_EDGE('',*,*,#6054,.F.);
#8177=ORIENTED_EDGE('',*,*,#6051,.F.);
#8178=ORIENTED_EDGE('',*,*,#6048,.F.);
#8179=ORIENTED_EDGE('',*,*,#6045,.F.);
#8180=ORIENTED_EDGE('',*,*,#6042,.F.);
#8181=ORIENTED_EDGE('',*,*,#6235,.T.);
#8182=ORIENTED_EDGE('',*,*,#6238,.T.);
#8183=ORIENTED_EDGE('',*,*,#6242,.T.);
#8184=ORIENTED_EDGE('',*,*,#6243,.F.);
#8185=ORIENTED_EDGE('',*,*,#6114,.F.);
#8186=ORIENTED_EDGE('',*,*,#6193,.F.);
#8187=ORIENTED_EDGE('',*,*,#6112,.F.);
#8188=ORIENTED_EDGE('',*,*,#6109,.F.);
#8189=ORIENTED_EDGE('',*,*,#6106,.F.);
#8190=ORIENTED_EDGE('',*,*,#6103,.F.);
#8191=ORIENTED_EDGE('',*,*,#6100,.F.);
#8192=ORIENTED_EDGE('',*,*,#6096,.F.);
#8193=ORIENTED_EDGE('',*,*,#6244,.F.);
#8194=ORIENTED_EDGE('',*,*,#6098,.T.);
#8195=ORIENTED_EDGE('',*,*,#6102,.T.);
#8196=ORIENTED_EDGE('',*,*,#6105,.T.);
#8197=ORIENTED_EDGE('',*,*,#6108,.T.);
#8198=ORIENTED_EDGE('',*,*,#6111,.T.);
#8199=ORIENTED_EDGE('',*,*,#6192,.T.);
#8200=ORIENTED_EDGE('',*,*,#6116,.T.);
#8201=ORIENTED_EDGE('',*,*,#6245,.F.);
#8202=ORIENTED_EDGE('',*,*,#6246,.F.);
#8203=ORIENTED_EDGE('',*,*,#6236,.T.);
#8204=ORIENTED_EDGE('',*,*,#6040,.F.);
#8205=ORIENTED_EDGE('',*,*,#6044,.F.);
#8206=ORIENTED_EDGE('',*,*,#6047,.F.);
#8207=ORIENTED_EDGE('',*,*,#6050,.F.);
#8208=ORIENTED_EDGE('',*,*,#6053,.F.);
#8209=ORIENTED_EDGE('',*,*,#6056,.F.);
#8210=ORIENTED_EDGE('',*,*,#6059,.F.);
#8211=ORIENTED_EDGE('',*,*,#6062,.F.);
#8212=ORIENTED_EDGE('',*,*,#6065,.F.);
#8213=ORIENTED_EDGE('',*,*,#6068,.F.);
#8214=ORIENTED_EDGE('',*,*,#6071,.F.);
#8215=ORIENTED_EDGE('',*,*,#6074,.F.);
#8216=ORIENTED_EDGE('',*,*,#6077,.F.);
#8217=ORIENTED_EDGE('',*,*,#6080,.F.);
#8218=ORIENTED_EDGE('',*,*,#6083,.F.);
#8219=ORIENTED_EDGE('',*,*,#6086,.F.);
#8220=ORIENTED_EDGE('',*,*,#6089,.F.);
#8221=ORIENTED_EDGE('',*,*,#6092,.F.);
#8222=ORIENTED_EDGE('',*,*,#6196,.F.);
#8223=ORIENTED_EDGE('',*,*,#6243,.T.);
#8224=ORIENTED_EDGE('',*,*,#6247,.T.);
#8225=ORIENTED_EDGE('',*,*,#6245,.T.);
#8226=ORIENTED_EDGE('',*,*,#6115,.T.);
#8227=ORIENTED_EDGE('',*,*,#6242,.F.);
#8228=ORIENTED_EDGE('',*,*,#6237,.T.);
#8229=ORIENTED_EDGE('',*,*,#6246,.T.);
#8230=ORIENTED_EDGE('',*,*,#6247,.F.);
#8231=ORIENTED_EDGE('',*,*,#6248,.F.);
#8232=ORIENTED_EDGE('',*,*,#6249,.F.);
#8233=ORIENTED_EDGE('',*,*,#6250,.F.);
#8234=ORIENTED_EDGE('',*,*,#6251,.F.);
#8235=ORIENTED_EDGE('',*,*,#6252,.T.);
#8236=ORIENTED_EDGE('',*,*,#6253,.F.);
#8237=ORIENTED_EDGE('',*,*,#6254,.F.);
#8238=ORIENTED_EDGE('',*,*,#6255,.F.);
#8239=ORIENTED_EDGE('',*,*,#6206,.T.);
#8240=ORIENTED_EDGE('',*,*,#6204,.T.);
#8241=ORIENTED_EDGE('',*,*,#6256,.T.);
#8242=ORIENTED_EDGE('',*,*,#6164,.T.);
#8243=ORIENTED_EDGE('',*,*,#6168,.T.);
#8244=ORIENTED_EDGE('',*,*,#6257,.T.);
#8245=ORIENTED_EDGE('',*,*,#6201,.T.);
#8246=ORIENTED_EDGE('',*,*,#6258,.T.);
#8247=ORIENTED_EDGE('',*,*,#6141,.T.);
#8248=ORIENTED_EDGE('',*,*,#6145,.T.);
#8249=ORIENTED_EDGE('',*,*,#6259,.T.);
#8250=ORIENTED_EDGE('',*,*,#6198,.T.);
#8251=ORIENTED_EDGE('',*,*,#6260,.T.);
#8252=ORIENTED_EDGE('',*,*,#6118,.T.);
#8253=ORIENTED_EDGE('',*,*,#6122,.T.);
#8254=ORIENTED_EDGE('',*,*,#6261,.T.);
#8255=ORIENTED_EDGE('',*,*,#6195,.T.);
#8256=ORIENTED_EDGE('',*,*,#6241,.T.);
#8257=ORIENTED_EDGE('',*,*,#6095,.T.);
#8258=ORIENTED_EDGE('',*,*,#6099,.T.);
#8259=ORIENTED_EDGE('',*,*,#6244,.T.);
#8260=ORIENTED_EDGE('',*,*,#6260,.F.);
#8261=ORIENTED_EDGE('',*,*,#6197,.F.);
#8262=ORIENTED_EDGE('',*,*,#6038,.F.);
#8263=ORIENTED_EDGE('',*,*,#6035,.F.);
#8264=ORIENTED_EDGE('',*,*,#6032,.F.);
#8265=ORIENTED_EDGE('',*,*,#6029,.F.);
#8266=ORIENTED_EDGE('',*,*,#6026,.F.);
#8267=ORIENTED_EDGE('',*,*,#6023,.F.);
#8268=ORIENTED_EDGE('',*,*,#6020,.F.);
#8269=ORIENTED_EDGE('',*,*,#6017,.F.);
#8270=ORIENTED_EDGE('',*,*,#6014,.F.);
#8271=ORIENTED_EDGE('',*,*,#6011,.F.);
#8272=ORIENTED_EDGE('',*,*,#6008,.F.);
#8273=ORIENTED_EDGE('',*,*,#6005,.F.);
#8274=ORIENTED_EDGE('',*,*,#6002,.F.);
#8275=ORIENTED_EDGE('',*,*,#5999,.F.);
#8276=ORIENTED_EDGE('',*,*,#5996,.F.);
#8277=ORIENTED_EDGE('',*,*,#5993,.F.);
#8278=ORIENTED_EDGE('',*,*,#5990,.F.);
#8279=ORIENTED_EDGE('',*,*,#5987,.F.);
#8280=ORIENTED_EDGE('',*,*,#6229,.T.);
#8281=ORIENTED_EDGE('',*,*,#6232,.T.);
#8282=ORIENTED_EDGE('',*,*,#6262,.T.);
#8283=ORIENTED_EDGE('',*,*,#6263,.F.);
#8284=ORIENTED_EDGE('',*,*,#6137,.F.);
#8285=ORIENTED_EDGE('',*,*,#6191,.F.);
#8286=ORIENTED_EDGE('',*,*,#6135,.F.);
#8287=ORIENTED_EDGE('',*,*,#6132,.F.);
#8288=ORIENTED_EDGE('',*,*,#6129,.F.);
#8289=ORIENTED_EDGE('',*,*,#6126,.F.);
#8290=ORIENTED_EDGE('',*,*,#6123,.F.);
#8291=ORIENTED_EDGE('',*,*,#6119,.F.);
#8292=ORIENTED_EDGE('',*,*,#6261,.F.);
#8293=ORIENTED_EDGE('',*,*,#6121,.T.);
#8294=ORIENTED_EDGE('',*,*,#6125,.T.);
#8295=ORIENTED_EDGE('',*,*,#6128,.T.);
#8296=ORIENTED_EDGE('',*,*,#6131,.T.);
#8297=ORIENTED_EDGE('',*,*,#6134,.T.);
#8298=ORIENTED_EDGE('',*,*,#6190,.T.);
#8299=ORIENTED_EDGE('',*,*,#6139,.T.);
#8300=ORIENTED_EDGE('',*,*,#6264,.F.);
#8301=ORIENTED_EDGE('',*,*,#6265,.F.);
#8302=ORIENTED_EDGE('',*,*,#6230,.T.);
#8303=ORIENTED_EDGE('',*,*,#5983,.F.);
#8304=ORIENTED_EDGE('',*,*,#5986,.F.);
#8305=ORIENTED_EDGE('',*,*,#5989,.F.);
#8306=ORIENTED_EDGE('',*,*,#5992,.F.);
#8307=ORIENTED_EDGE('',*,*,#5995,.F.);
#8308=ORIENTED_EDGE('',*,*,#5998,.F.);
#8309=ORIENTED_EDGE('',*,*,#6001,.F.);
#8310=ORIENTED_EDGE('',*,*,#6004,.F.);
#8311=ORIENTED_EDGE('',*,*,#6007,.F.);
#8312=ORIENTED_EDGE('',*,*,#6010,.F.);
#8313=ORIENTED_EDGE('',*,*,#6013,.F.);
#8314=ORIENTED_EDGE('',*,*,#6016,.F.);
#8315=ORIENTED_EDGE('',*,*,#6019,.F.);
#8316=ORIENTED_EDGE('',*,*,#6022,.F.);
#8317=ORIENTED_EDGE('',*,*,#6025,.F.);
#8318=ORIENTED_EDGE('',*,*,#6028,.F.);
#8319=ORIENTED_EDGE('',*,*,#6031,.F.);
#8320=ORIENTED_EDGE('',*,*,#6034,.F.);
#8321=ORIENTED_EDGE('',*,*,#6037,.F.);
#8322=ORIENTED_EDGE('',*,*,#6199,.F.);
#8323=ORIENTED_EDGE('',*,*,#6263,.T.);
#8324=ORIENTED_EDGE('',*,*,#6266,.T.);
#8325=ORIENTED_EDGE('',*,*,#6264,.T.);
#8326=ORIENTED_EDGE('',*,*,#6138,.T.);
#8327=ORIENTED_EDGE('',*,*,#6262,.F.);
#8328=ORIENTED_EDGE('',*,*,#6231,.T.);
#8329=ORIENTED_EDGE('',*,*,#6265,.T.);
#8330=ORIENTED_EDGE('',*,*,#6266,.F.);
#8331=ORIENTED_EDGE('',*,*,#6258,.F.);
#8332=ORIENTED_EDGE('',*,*,#6200,.F.);
#8333=ORIENTED_EDGE('',*,*,#5981,.F.);
#8334=ORIENTED_EDGE('',*,*,#5978,.F.);
#8335=ORIENTED_EDGE('',*,*,#5975,.F.);
#8336=ORIENTED_EDGE('',*,*,#5972,.F.);
#8337=ORIENTED_EDGE('',*,*,#5969,.F.);
#8338=ORIENTED_EDGE('',*,*,#5966,.F.);
#8339=ORIENTED_EDGE('',*,*,#5963,.F.);
#8340=ORIENTED_EDGE('',*,*,#5960,.F.);
#8341=ORIENTED_EDGE('',*,*,#5957,.F.);
#8342=ORIENTED_EDGE('',*,*,#5954,.F.);
#8343=ORIENTED_EDGE('',*,*,#5951,.F.);
#8344=ORIENTED_EDGE('',*,*,#5948,.F.);
#8345=ORIENTED_EDGE('',*,*,#5945,.F.);
#8346=ORIENTED_EDGE('',*,*,#5942,.F.);
#8347=ORIENTED_EDGE('',*,*,#5939,.F.);
#8348=ORIENTED_EDGE('',*,*,#5936,.F.);
#8349=ORIENTED_EDGE('',*,*,#5933,.F.);
#8350=ORIENTED_EDGE('',*,*,#5930,.F.);
#8351=ORIENTED_EDGE('',*,*,#5927,.F.);
#8352=ORIENTED_EDGE('',*,*,#6223,.T.);
#8353=ORIENTED_EDGE('',*,*,#6226,.T.);
#8354=ORIENTED_EDGE('',*,*,#6267,.T.);
#8355=ORIENTED_EDGE('',*,*,#6268,.F.);
#8356=ORIENTED_EDGE('',*,*,#6160,.F.);
#8357=ORIENTED_EDGE('',*,*,#6189,.F.);
#8358=ORIENTED_EDGE('',*,*,#6158,.F.);
#8359=ORIENTED_EDGE('',*,*,#6155,.F.);
#8360=ORIENTED_EDGE('',*,*,#6152,.F.);
#8361=ORIENTED_EDGE('',*,*,#6149,.F.);
#8362=ORIENTED_EDGE('',*,*,#6146,.F.);
#8363=ORIENTED_EDGE('',*,*,#6142,.F.);
#8364=ORIENTED_EDGE('',*,*,#6259,.F.);
#8365=ORIENTED_EDGE('',*,*,#6144,.T.);
#8366=ORIENTED_EDGE('',*,*,#6148,.T.);
#8367=ORIENTED_EDGE('',*,*,#6151,.T.);
#8368=ORIENTED_EDGE('',*,*,#6154,.T.);
#8369=ORIENTED_EDGE('',*,*,#6157,.T.);
#8370=ORIENTED_EDGE('',*,*,#6188,.T.);
#8371=ORIENTED_EDGE('',*,*,#6162,.T.);
#8372=ORIENTED_EDGE('',*,*,#6269,.F.);
#8373=ORIENTED_EDGE('',*,*,#6270,.F.);
#8374=ORIENTED_EDGE('',*,*,#6224,.T.);
#8375=ORIENTED_EDGE('',*,*,#5925,.F.);
#8376=ORIENTED_EDGE('',*,*,#5929,.F.);
#8377=ORIENTED_EDGE('',*,*,#5932,.F.);
#8378=ORIENTED_EDGE('',*,*,#5935,.F.);
#8379=ORIENTED_EDGE('',*,*,#5938,.F.);
#8380=ORIENTED_EDGE('',*,*,#5941,.F.);
#8381=ORIENTED_EDGE('',*,*,#5944,.F.);
#8382=ORIENTED_EDGE('',*,*,#5947,.F.);
#8383=ORIENTED_EDGE('',*,*,#5950,.F.);
#8384=ORIENTED_EDGE('',*,*,#5953,.F.);
#8385=ORIENTED_EDGE('',*,*,#5956,.F.);
#8386=ORIENTED_EDGE('',*,*,#5959,.F.);
#8387=ORIENTED_EDGE('',*,*,#5962,.F.);
#8388=ORIENTED_EDGE('',*,*,#5965,.F.);
#8389=ORIENTED_EDGE('',*,*,#5968,.F.);
#8390=ORIENTED_EDGE('',*,*,#5971,.F.);
#8391=ORIENTED_EDGE('',*,*,#5974,.F.);
#8392=ORIENTED_EDGE('',*,*,#5977,.F.);
#8393=ORIENTED_EDGE('',*,*,#5980,.F.);
#8394=ORIENTED_EDGE('',*,*,#6202,.F.);
#8395=ORIENTED_EDGE('',*,*,#6268,.T.);
#8396=ORIENTED_EDGE('',*,*,#6271,.T.);
#8397=ORIENTED_EDGE('',*,*,#6269,.T.);
#8398=ORIENTED_EDGE('',*,*,#6161,.T.);
#8399=ORIENTED_EDGE('',*,*,#6267,.F.);
#8400=ORIENTED_EDGE('',*,*,#6225,.T.);
#8401=ORIENTED_EDGE('',*,*,#6270,.T.);
#8402=ORIENTED_EDGE('',*,*,#6271,.F.);
#8403=ORIENTED_EDGE('',*,*,#5869,.F.);
#8404=ORIENTED_EDGE('',*,*,#6217,.T.);
#8405=ORIENTED_EDGE('',*,*,#6220,.T.);
#8406=ORIENTED_EDGE('',*,*,#6272,.T.);
#8407=ORIENTED_EDGE('',*,*,#6273,.F.);
#8408=ORIENTED_EDGE('',*,*,#6183,.F.);
#8409=ORIENTED_EDGE('',*,*,#6187,.F.);
#8410=ORIENTED_EDGE('',*,*,#6181,.F.);
#8411=ORIENTED_EDGE('',*,*,#6178,.F.);
#8412=ORIENTED_EDGE('',*,*,#6175,.F.);
#8413=ORIENTED_EDGE('',*,*,#6172,.F.);
#8414=ORIENTED_EDGE('',*,*,#6169,.F.);
#8415=ORIENTED_EDGE('',*,*,#6165,.F.);
#8416=ORIENTED_EDGE('',*,*,#6256,.F.);
#8417=ORIENTED_EDGE('',*,*,#6203,.F.);
#8418=ORIENTED_EDGE('',*,*,#5923,.F.);
#8419=ORIENTED_EDGE('',*,*,#5920,.F.);
#8420=ORIENTED_EDGE('',*,*,#5917,.F.);
#8421=ORIENTED_EDGE('',*,*,#5914,.F.);
#8422=ORIENTED_EDGE('',*,*,#5911,.F.);
#8423=ORIENTED_EDGE('',*,*,#5908,.F.);
#8424=ORIENTED_EDGE('',*,*,#5905,.F.);
#8425=ORIENTED_EDGE('',*,*,#5902,.F.);
#8426=ORIENTED_EDGE('',*,*,#5899,.F.);
#8427=ORIENTED_EDGE('',*,*,#5896,.F.);
#8428=ORIENTED_EDGE('',*,*,#5893,.F.);
#8429=ORIENTED_EDGE('',*,*,#5890,.F.);
#8430=ORIENTED_EDGE('',*,*,#5887,.F.);
#8431=ORIENTED_EDGE('',*,*,#5884,.F.);
#8432=ORIENTED_EDGE('',*,*,#5881,.F.);
#8433=ORIENTED_EDGE('',*,*,#5878,.F.);
#8434=ORIENTED_EDGE('',*,*,#5875,.F.);
#8435=ORIENTED_EDGE('',*,*,#5872,.F.);
#8436=ORIENTED_EDGE('',*,*,#6205,.F.);
#8437=ORIENTED_EDGE('',*,*,#6257,.F.);
#8438=ORIENTED_EDGE('',*,*,#6167,.T.);
#8439=ORIENTED_EDGE('',*,*,#6171,.T.);
#8440=ORIENTED_EDGE('',*,*,#6174,.T.);
#8441=ORIENTED_EDGE('',*,*,#6177,.T.);
#8442=ORIENTED_EDGE('',*,*,#6180,.T.);
#8443=ORIENTED_EDGE('',*,*,#6186,.T.);
#8444=ORIENTED_EDGE('',*,*,#6185,.T.);
#8445=ORIENTED_EDGE('',*,*,#6274,.F.);
#8446=ORIENTED_EDGE('',*,*,#6275,.F.);
#8447=ORIENTED_EDGE('',*,*,#6218,.T.);
#8448=ORIENTED_EDGE('',*,*,#5867,.F.);
#8449=ORIENTED_EDGE('',*,*,#5871,.F.);
#8450=ORIENTED_EDGE('',*,*,#5874,.F.);
#8451=ORIENTED_EDGE('',*,*,#5877,.F.);
#8452=ORIENTED_EDGE('',*,*,#5880,.F.);
#8453=ORIENTED_EDGE('',*,*,#5883,.F.);
#8454=ORIENTED_EDGE('',*,*,#5886,.F.);
#8455=ORIENTED_EDGE('',*,*,#5889,.F.);
#8456=ORIENTED_EDGE('',*,*,#5892,.F.);
#8457=ORIENTED_EDGE('',*,*,#5895,.F.);
#8458=ORIENTED_EDGE('',*,*,#5898,.F.);
#8459=ORIENTED_EDGE('',*,*,#5901,.F.);
#8460=ORIENTED_EDGE('',*,*,#5904,.F.);
#8461=ORIENTED_EDGE('',*,*,#5907,.F.);
#8462=ORIENTED_EDGE('',*,*,#5910,.F.);
#8463=ORIENTED_EDGE('',*,*,#5913,.F.);
#8464=ORIENTED_EDGE('',*,*,#5916,.F.);
#8465=ORIENTED_EDGE('',*,*,#5919,.F.);
#8466=ORIENTED_EDGE('',*,*,#5922,.F.);
#8467=ORIENTED_EDGE('',*,*,#6273,.T.);
#8468=ORIENTED_EDGE('',*,*,#6276,.T.);
#8469=ORIENTED_EDGE('',*,*,#6274,.T.);
#8470=ORIENTED_EDGE('',*,*,#6184,.T.);
#8471=ORIENTED_EDGE('',*,*,#6272,.F.);
#8472=ORIENTED_EDGE('',*,*,#6219,.T.);
#8473=ORIENTED_EDGE('',*,*,#6275,.T.);
#8474=ORIENTED_EDGE('',*,*,#6276,.F.);
#8475=ORIENTED_EDGE('',*,*,#6209,.T.);
#8476=ORIENTED_EDGE('',*,*,#6208,.T.);
#8477=ORIENTED_EDGE('',*,*,#6216,.T.);
#8478=ORIENTED_EDGE('',*,*,#6211,.F.);
#8479=ORIENTED_EDGE('',*,*,#6277,.F.);
#8480=ORIENTED_EDGE('',*,*,#6278,.T.);
#8481=ORIENTED_EDGE('',*,*,#6279,.T.);
#8482=ORIENTED_EDGE('',*,*,#6255,.T.);
#8483=ORIENTED_EDGE('',*,*,#6280,.F.);
#8484=ORIENTED_EDGE('',*,*,#6281,.T.);
#8485=ORIENTED_EDGE('',*,*,#6277,.T.);
#8486=ORIENTED_EDGE('',*,*,#6254,.T.);
#8487=ORIENTED_EDGE('',*,*,#6282,.T.);
#8488=ORIENTED_EDGE('',*,*,#6283,.F.);
#8489=ORIENTED_EDGE('',*,*,#6284,.F.);
#8490=ORIENTED_EDGE('',*,*,#6278,.F.);
#8491=ORIENTED_EDGE('',*,*,#6279,.F.);
#8492=ORIENTED_EDGE('',*,*,#6285,.T.);
#8493=ORIENTED_EDGE('',*,*,#6286,.T.);
#8494=ORIENTED_EDGE('',*,*,#6248,.T.);
#8495=ORIENTED_EDGE('',*,*,#6287,.F.);
#8496=ORIENTED_EDGE('',*,*,#6288,.T.);
#8497=ORIENTED_EDGE('',*,*,#6280,.T.);
#8498=ORIENTED_EDGE('',*,*,#6253,.T.);
#8499=ORIENTED_EDGE('',*,*,#6289,.T.);
#8500=ORIENTED_EDGE('',*,*,#6290,.F.);
#8501=ORIENTED_EDGE('',*,*,#6282,.F.);
#8502=ORIENTED_EDGE('',*,*,#6281,.F.);
#8503=ORIENTED_EDGE('',*,*,#6291,.F.);
#8504=ORIENTED_EDGE('',*,*,#6292,.T.);
#8505=ORIENTED_EDGE('',*,*,#6287,.T.);
#8506=ORIENTED_EDGE('',*,*,#6252,.F.);
#8507=ORIENTED_EDGE('',*,*,#6289,.F.);
#8508=ORIENTED_EDGE('',*,*,#6288,.F.);
#8509=ORIENTED_EDGE('',*,*,#6293,.F.);
#8510=ORIENTED_EDGE('',*,*,#6294,.F.);
#8511=ORIENTED_EDGE('',*,*,#6295,.F.);
#8512=ORIENTED_EDGE('',*,*,#6296,.T.);
#8513=ORIENTED_EDGE('',*,*,#6291,.T.);
#8514=ORIENTED_EDGE('',*,*,#6251,.T.);
#8515=ORIENTED_EDGE('',*,*,#6293,.T.);
#8516=ORIENTED_EDGE('',*,*,#6292,.F.);
#8517=ORIENTED_EDGE('',*,*,#6297,.F.);
#8518=ORIENTED_EDGE('',*,*,#6298,.F.);
#8519=ORIENTED_EDGE('',*,*,#6299,.F.);
#8520=ORIENTED_EDGE('',*,*,#6300,.T.);
#8521=ORIENTED_EDGE('',*,*,#6295,.T.);
#8522=ORIENTED_EDGE('',*,*,#6250,.T.);
#8523=ORIENTED_EDGE('',*,*,#6297,.T.);
#8524=ORIENTED_EDGE('',*,*,#6296,.F.);
#8525=ORIENTED_EDGE('',*,*,#6301,.F.);
#8526=ORIENTED_EDGE('',*,*,#6302,.F.);
#8527=ORIENTED_EDGE('',*,*,#6286,.F.);
#8528=ORIENTED_EDGE('',*,*,#6303,.T.);
#8529=ORIENTED_EDGE('',*,*,#6299,.T.);
#8530=ORIENTED_EDGE('',*,*,#6249,.T.);
#8531=ORIENTED_EDGE('',*,*,#6301,.T.);
#8532=ORIENTED_EDGE('',*,*,#6300,.F.);
#8533=ORIENTED_EDGE('',*,*,#6304,.F.);
#8534=ORIENTED_EDGE('',*,*,#6305,.F.);
#8535=ORIENTED_EDGE('',*,*,#6304,.T.);
#8536=ORIENTED_EDGE('',*,*,#6303,.F.);
#8537=ORIENTED_EDGE('',*,*,#6306,.T.);
#8538=ORIENTED_EDGE('',*,*,#6307,.F.);
#8539=ORIENTED_EDGE('',*,*,#6284,.T.);
#8540=ORIENTED_EDGE('',*,*,#6308,.F.);
#8541=ORIENTED_EDGE('',*,*,#6306,.F.);
#8542=ORIENTED_EDGE('',*,*,#6285,.F.);
#8543=ORIENTED_EDGE('',*,*,#6307,.T.);
#8544=ORIENTED_EDGE('',*,*,#6308,.T.);
#8545=ORIENTED_EDGE('',*,*,#6283,.T.);
#8546=ORIENTED_EDGE('',*,*,#6290,.T.);
#8547=ORIENTED_EDGE('',*,*,#6294,.T.);
#8548=ORIENTED_EDGE('',*,*,#6298,.T.);
#8549=ORIENTED_EDGE('',*,*,#6302,.T.);
#8550=ORIENTED_EDGE('',*,*,#6305,.T.);
#8551=ORIENTED_EDGE('',*,*,#6228,.T.);
#8552=ORIENTED_EDGE('',*,*,#6222,.T.);
#8553=ORIENTED_EDGE('',*,*,#6234,.T.);
#8554=ORIENTED_EDGE('',*,*,#6240,.T.);
#8555=ORIENTED_EDGE('',*,*,#6212,.T.);
#8556=ORIENTED_EDGE('',*,*,#6309,.F.);
#8557=ORIENTED_EDGE('',*,*,#6310,.F.);
#8558=ORIENTED_EDGE('',*,*,#6311,.F.);
#8559=ORIENTED_EDGE('',*,*,#6312,.F.);
#8560=ORIENTED_EDGE('',*,*,#6309,.T.);
#8561=ORIENTED_EDGE('',*,*,#6313,.F.);
#8562=ORIENTED_EDGE('',*,*,#6314,.F.);
#8563=ORIENTED_EDGE('',*,*,#6315,.F.);
#8564=ORIENTED_EDGE('',*,*,#6316,.T.);
#8565=ORIENTED_EDGE('',*,*,#6317,.T.);
#8566=ORIENTED_EDGE('',*,*,#6316,.F.);
#8567=ORIENTED_EDGE('',*,*,#6318,.T.);
#8568=ORIENTED_EDGE('',*,*,#6319,.T.);
#8569=ORIENTED_EDGE('',*,*,#6315,.T.);
#8570=ORIENTED_EDGE('',*,*,#6320,.T.);
#8571=ORIENTED_EDGE('',*,*,#6321,.T.);
#8572=ORIENTED_EDGE('',*,*,#6322,.T.);
#8573=ORIENTED_EDGE('',*,*,#6310,.T.);
#8574=ORIENTED_EDGE('',*,*,#6319,.F.);
#8575=ORIENTED_EDGE('',*,*,#6313,.T.);
#8576=ORIENTED_EDGE('',*,*,#6312,.T.);
#8577=ORIENTED_EDGE('',*,*,#6317,.F.);
#8578=ORIENTED_EDGE('',*,*,#6318,.F.);
#8579=ORIENTED_EDGE('',*,*,#6323,.T.);
#8580=ORIENTED_EDGE('',*,*,#6321,.F.);
#8581=ORIENTED_EDGE('',*,*,#6314,.T.);
#8582=ORIENTED_EDGE('',*,*,#6311,.T.);
#8583=ORIENTED_EDGE('',*,*,#6322,.F.);
#8584=ORIENTED_EDGE('',*,*,#6323,.F.);
#8585=ORIENTED_EDGE('',*,*,#6320,.F.);
#8586=ORIENTED_EDGE('',*,*,#6324,.F.);
#8587=ORIENTED_EDGE('',*,*,#6325,.T.);
#8588=ORIENTED_EDGE('',*,*,#6326,.T.);
#8589=ORIENTED_EDGE('',*,*,#6325,.F.);
#8590=ORIENTED_EDGE('',*,*,#6327,.F.);
#8591=ORIENTED_EDGE('',*,*,#6328,.T.);
#8592=ORIENTED_EDGE('',*,*,#6329,.F.);
#8593=ORIENTED_EDGE('',*,*,#6328,.F.);
#8594=ORIENTED_EDGE('',*,*,#6330,.F.);
#8595=ORIENTED_EDGE('',*,*,#6331,.T.);
#8596=ORIENTED_EDGE('',*,*,#6332,.F.);
#8597=ORIENTED_EDGE('',*,*,#6331,.F.);
#8598=ORIENTED_EDGE('',*,*,#6333,.F.);
#8599=ORIENTED_EDGE('',*,*,#6334,.T.);
#8600=ORIENTED_EDGE('',*,*,#6335,.F.);
#8601=ORIENTED_EDGE('',*,*,#6334,.F.);
#8602=ORIENTED_EDGE('',*,*,#6336,.F.);
#8603=ORIENTED_EDGE('',*,*,#6337,.T.);
#8604=ORIENTED_EDGE('',*,*,#6338,.F.);
#8605=ORIENTED_EDGE('',*,*,#6337,.F.);
#8606=ORIENTED_EDGE('',*,*,#6339,.F.);
#8607=ORIENTED_EDGE('',*,*,#6340,.T.);
#8608=ORIENTED_EDGE('',*,*,#6327,.T.);
#8609=ORIENTED_EDGE('',*,*,#6340,.F.);
#8610=ORIENTED_EDGE('',*,*,#6341,.F.);
#8611=ORIENTED_EDGE('',*,*,#6342,.T.);
#8612=ORIENTED_EDGE('',*,*,#6330,.T.);
#8613=ORIENTED_EDGE('',*,*,#6342,.F.);
#8614=ORIENTED_EDGE('',*,*,#6343,.F.);
#8615=ORIENTED_EDGE('',*,*,#6344,.T.);
#8616=ORIENTED_EDGE('',*,*,#6333,.T.);
#8617=ORIENTED_EDGE('',*,*,#6344,.F.);
#8618=ORIENTED_EDGE('',*,*,#6345,.F.);
#8619=ORIENTED_EDGE('',*,*,#6346,.T.);
#8620=ORIENTED_EDGE('',*,*,#6336,.T.);
#8621=ORIENTED_EDGE('',*,*,#6346,.F.);
#8622=ORIENTED_EDGE('',*,*,#6347,.F.);
#8623=ORIENTED_EDGE('',*,*,#6348,.T.);
#8624=ORIENTED_EDGE('',*,*,#6349,.F.);
#8625=ORIENTED_EDGE('',*,*,#6348,.F.);
#8626=ORIENTED_EDGE('',*,*,#6345,.T.);
#8627=ORIENTED_EDGE('',*,*,#6343,.T.);
#8628=ORIENTED_EDGE('',*,*,#6341,.T.);
#8629=ORIENTED_EDGE('',*,*,#6339,.T.);
#8630=ORIENTED_EDGE('',*,*,#6350,.T.);
#8631=ORIENTED_EDGE('',*,*,#6351,.T.);
#8632=ORIENTED_EDGE('',*,*,#6352,.T.);
#8633=ORIENTED_EDGE('',*,*,#6353,.T.);
#8634=ORIENTED_EDGE('',*,*,#6354,.T.);
#8635=ORIENTED_EDGE('',*,*,#6355,.F.);
#8636=ORIENTED_EDGE('',*,*,#6352,.F.);
#8637=ORIENTED_EDGE('',*,*,#6356,.T.);
#8638=ORIENTED_EDGE('',*,*,#6357,.T.);
#8639=ORIENTED_EDGE('',*,*,#6358,.F.);
#8640=ORIENTED_EDGE('',*,*,#6353,.F.);
#8641=ORIENTED_EDGE('',*,*,#6355,.T.);
#8642=ORIENTED_EDGE('',*,*,#6359,.T.);
#8643=ORIENTED_EDGE('',*,*,#6360,.F.);
#8644=ORIENTED_EDGE('',*,*,#6350,.F.);
#8645=ORIENTED_EDGE('',*,*,#6358,.T.);
#8646=ORIENTED_EDGE('',*,*,#6361,.T.);
#8647=ORIENTED_EDGE('',*,*,#6356,.F.);
#8648=ORIENTED_EDGE('',*,*,#6351,.F.);
#8649=ORIENTED_EDGE('',*,*,#6360,.T.);
#8650=ORIENTED_EDGE('',*,*,#6362,.T.);
#8651=ORIENTED_EDGE('',*,*,#6363,.T.);
#8652=ORIENTED_EDGE('',*,*,#6364,.T.);
#8653=ORIENTED_EDGE('',*,*,#6365,.T.);
#8654=ORIENTED_EDGE('',*,*,#6361,.F.);
#8655=ORIENTED_EDGE('',*,*,#6359,.F.);
#8656=ORIENTED_EDGE('',*,*,#6357,.F.);
#8657=ORIENTED_EDGE('',*,*,#6354,.F.);
#8658=ORIENTED_EDGE('',*,*,#6366,.T.);
#8659=ORIENTED_EDGE('',*,*,#6367,.T.);
#8660=ORIENTED_EDGE('',*,*,#6368,.F.);
#8661=ORIENTED_EDGE('',*,*,#6363,.F.);
#8662=ORIENTED_EDGE('',*,*,#6369,.T.);
#8663=ORIENTED_EDGE('',*,*,#6370,.T.);
#8664=ORIENTED_EDGE('',*,*,#6371,.T.);
#8665=ORIENTED_EDGE('',*,*,#6372,.T.);
#8666=ORIENTED_EDGE('',*,*,#6373,.T.);
#8667=ORIENTED_EDGE('',*,*,#6374,.T.);
#8668=ORIENTED_EDGE('',*,*,#6375,.T.);
#8669=ORIENTED_EDGE('',*,*,#6376,.T.);
#8670=ORIENTED_EDGE('',*,*,#6329,.T.);
#8671=ORIENTED_EDGE('',*,*,#6332,.T.);
#8672=ORIENTED_EDGE('',*,*,#6335,.T.);
#8673=ORIENTED_EDGE('',*,*,#6338,.T.);
#8674=ORIENTED_EDGE('',*,*,#6326,.F.);
#8675=ORIENTED_EDGE('',*,*,#6377,.T.);
#8676=ORIENTED_EDGE('',*,*,#6372,.F.);
#8677=ORIENTED_EDGE('',*,*,#6378,.F.);
#8678=ORIENTED_EDGE('',*,*,#6379,.F.);
#8679=ORIENTED_EDGE('',*,*,#6378,.T.);
#8680=ORIENTED_EDGE('',*,*,#6371,.F.);
#8681=ORIENTED_EDGE('',*,*,#6380,.F.);
#8682=ORIENTED_EDGE('',*,*,#6381,.F.);
#8683=ORIENTED_EDGE('',*,*,#6380,.T.);
#8684=ORIENTED_EDGE('',*,*,#6370,.F.);
#8685=ORIENTED_EDGE('',*,*,#6382,.T.);
#8686=ORIENTED_EDGE('',*,*,#6383,.F.);
#8687=ORIENTED_EDGE('',*,*,#6384,.T.);
#8688=ORIENTED_EDGE('',*,*,#6381,.T.);
#8689=ORIENTED_EDGE('',*,*,#6385,.F.);
#8690=ORIENTED_EDGE('',*,*,#6386,.F.);
#8691=ORIENTED_EDGE('',*,*,#6387,.T.);
#8692=ORIENTED_EDGE('',*,*,#6388,.F.);
#8693=ORIENTED_EDGE('',*,*,#6382,.F.);
#8694=ORIENTED_EDGE('',*,*,#6369,.F.);
#8695=ORIENTED_EDGE('',*,*,#6385,.T.);
#8696=ORIENTED_EDGE('',*,*,#6383,.T.);
#8697=ORIENTED_EDGE('',*,*,#6389,.F.);
#8698=ORIENTED_EDGE('',*,*,#6390,.F.);
#8699=ORIENTED_EDGE('',*,*,#6391,.T.);
#8700=ORIENTED_EDGE('',*,*,#6392,.F.);
#8701=ORIENTED_EDGE('',*,*,#6387,.F.);
#8702=ORIENTED_EDGE('',*,*,#6376,.F.);
#8703=ORIENTED_EDGE('',*,*,#6389,.T.);
#8704=ORIENTED_EDGE('',*,*,#6388,.T.);
#8705=ORIENTED_EDGE('',*,*,#6393,.F.);
#8706=ORIENTED_EDGE('',*,*,#6394,.T.);
#8707=ORIENTED_EDGE('',*,*,#6395,.T.);
#8708=ORIENTED_EDGE('',*,*,#6396,.F.);
#8709=ORIENTED_EDGE('',*,*,#6391,.F.);
#8710=ORIENTED_EDGE('',*,*,#6375,.F.);
#8711=ORIENTED_EDGE('',*,*,#6393,.T.);
#8712=ORIENTED_EDGE('',*,*,#6392,.T.);
#8713=ORIENTED_EDGE('',*,*,#6397,.F.);
#8714=ORIENTED_EDGE('',*,*,#6398,.F.);
#8715=ORIENTED_EDGE('',*,*,#6395,.F.);
#8716=ORIENTED_EDGE('',*,*,#6374,.F.);
#8717=ORIENTED_EDGE('',*,*,#6399,.F.);
#8718=ORIENTED_EDGE('',*,*,#6400,.F.);
#8719=ORIENTED_EDGE('',*,*,#6397,.T.);
#8720=ORIENTED_EDGE('',*,*,#6396,.T.);
#8721=ORIENTED_EDGE('',*,*,#6401,.F.);
#8722=ORIENTED_EDGE('',*,*,#6402,.F.);
#8723=ORIENTED_EDGE('',*,*,#6403,.T.);
#8724=ORIENTED_EDGE('',*,*,#6379,.T.);
#8725=ORIENTED_EDGE('',*,*,#6384,.F.);
#8726=ORIENTED_EDGE('',*,*,#6404,.F.);
#8727=ORIENTED_EDGE('',*,*,#6368,.T.);
#8728=ORIENTED_EDGE('',*,*,#6405,.T.);
#8729=ORIENTED_EDGE('',*,*,#6406,.T.);
#8730=ORIENTED_EDGE('',*,*,#6407,.F.);
#8731=ORIENTED_EDGE('',*,*,#6364,.F.);
#8732=ORIENTED_EDGE('',*,*,#6408,.T.);
#8733=ORIENTED_EDGE('',*,*,#6409,.F.);
#8734=ORIENTED_EDGE('',*,*,#6365,.F.);
#8735=ORIENTED_EDGE('',*,*,#6407,.T.);
#8736=ORIENTED_EDGE('',*,*,#6410,.T.);
#8737=ORIENTED_EDGE('',*,*,#6411,.T.);
#8738=ORIENTED_EDGE('',*,*,#6366,.F.);
#8739=ORIENTED_EDGE('',*,*,#6362,.F.);
#8740=ORIENTED_EDGE('',*,*,#6409,.T.);
#8741=ORIENTED_EDGE('',*,*,#6399,.T.);
#8742=ORIENTED_EDGE('',*,*,#6373,.F.);
#8743=ORIENTED_EDGE('',*,*,#6377,.F.);
#8744=ORIENTED_EDGE('',*,*,#6412,.F.);
#8745=ORIENTED_EDGE('',*,*,#6405,.F.);
#8746=ORIENTED_EDGE('',*,*,#6367,.F.);
#8747=ORIENTED_EDGE('',*,*,#6411,.F.);
#8748=ORIENTED_EDGE('',*,*,#6413,.F.);
#8749=ORIENTED_EDGE('',*,*,#6401,.T.);
#8750=ORIENTED_EDGE('',*,*,#6400,.T.);
#8751=ORIENTED_EDGE('',*,*,#6414,.F.);
#8752=ORIENTED_EDGE('',*,*,#6415,.F.);
#8753=ORIENTED_EDGE('',*,*,#6414,.T.);
#8754=ORIENTED_EDGE('',*,*,#6413,.T.);
#8755=ORIENTED_EDGE('',*,*,#6410,.F.);
#8756=ORIENTED_EDGE('',*,*,#6408,.F.);
#8757=ORIENTED_EDGE('',*,*,#6406,.F.);
#8758=ORIENTED_EDGE('',*,*,#6412,.T.);
#8759=ORIENTED_EDGE('',*,*,#6403,.F.);
#8760=ORIENTED_EDGE('',*,*,#6416,.F.);
#8761=ORIENTED_EDGE('',*,*,#6404,.T.);
#8762=ORIENTED_EDGE('',*,*,#6386,.T.);
#8763=ORIENTED_EDGE('',*,*,#6390,.T.);
#8764=ORIENTED_EDGE('',*,*,#6394,.F.);
#8765=ORIENTED_EDGE('',*,*,#6398,.T.);
#8766=ORIENTED_EDGE('',*,*,#6402,.T.);
#8767=ORIENTED_EDGE('',*,*,#6415,.T.);
#8768=ORIENTED_EDGE('',*,*,#6416,.T.);
#8769=ORIENTED_EDGE('',*,*,#6349,.T.);
#8770=ORIENTED_EDGE('',*,*,#6324,.T.);
#8771=ORIENTED_EDGE('',*,*,#6347,.T.);
#8772=ORIENTED_EDGE('',*,*,#6417,.T.);
#8773=ORIENTED_EDGE('',*,*,#6418,.T.);
#8774=ORIENTED_EDGE('',*,*,#6419,.T.);
#8775=ORIENTED_EDGE('',*,*,#6418,.F.);
#8776=ORIENTED_EDGE('',*,*,#6420,.F.);
#8777=ORIENTED_EDGE('',*,*,#6421,.T.);
#8778=ORIENTED_EDGE('',*,*,#6422,.T.);
#8779=ORIENTED_EDGE('',*,*,#6421,.F.);
#8780=ORIENTED_EDGE('',*,*,#6423,.F.);
#8781=ORIENTED_EDGE('',*,*,#6424,.T.);
#8782=ORIENTED_EDGE('',*,*,#6425,.T.);
#8783=ORIENTED_EDGE('',*,*,#6424,.F.);
#8784=ORIENTED_EDGE('',*,*,#6426,.F.);
#8785=ORIENTED_EDGE('',*,*,#6427,.T.);
#8786=ORIENTED_EDGE('',*,*,#6428,.T.);
#8787=ORIENTED_EDGE('',*,*,#6427,.F.);
#8788=ORIENTED_EDGE('',*,*,#6429,.F.);
#8789=ORIENTED_EDGE('',*,*,#6430,.T.);
#8790=ORIENTED_EDGE('',*,*,#6431,.T.);
#8791=ORIENTED_EDGE('',*,*,#6430,.F.);
#8792=ORIENTED_EDGE('',*,*,#6432,.T.);
#8793=ORIENTED_EDGE('',*,*,#6433,.T.);
#8794=ORIENTED_EDGE('',*,*,#6434,.F.);
#8795=ORIENTED_EDGE('',*,*,#6435,.F.);
#8796=ORIENTED_EDGE('',*,*,#6436,.F.);
#8797=ORIENTED_EDGE('',*,*,#6437,.T.);
#8798=ORIENTED_EDGE('',*,*,#6438,.T.);
#8799=ORIENTED_EDGE('',*,*,#6439,.T.);
#8800=ORIENTED_EDGE('',*,*,#6417,.F.);
#8801=ORIENTED_EDGE('',*,*,#6440,.F.);
#8802=ORIENTED_EDGE('',*,*,#6441,.F.);
#8803=ORIENTED_EDGE('',*,*,#6442,.F.);
#8804=ORIENTED_EDGE('',*,*,#6443,.F.);
#8805=ORIENTED_EDGE('',*,*,#6444,.T.);
#8806=ORIENTED_EDGE('',*,*,#6445,.T.);
#8807=ORIENTED_EDGE('',*,*,#6446,.T.);
#8808=ORIENTED_EDGE('',*,*,#6447,.F.);
#8809=ORIENTED_EDGE('',*,*,#6425,.F.);
#8810=ORIENTED_EDGE('',*,*,#6431,.F.);
#8811=ORIENTED_EDGE('',*,*,#6428,.F.);
#8812=ORIENTED_EDGE('',*,*,#6422,.F.);
#8813=ORIENTED_EDGE('',*,*,#6419,.F.);
#8814=ORIENTED_EDGE('',*,*,#6441,.T.);
#8815=ORIENTED_EDGE('',*,*,#6448,.F.);
#8816=ORIENTED_EDGE('',*,*,#6439,.F.);
#8817=ORIENTED_EDGE('',*,*,#6449,.T.);
#8818=ORIENTED_EDGE('',*,*,#6440,.T.);
#8819=ORIENTED_EDGE('',*,*,#6450,.F.);
#8820=ORIENTED_EDGE('',*,*,#6432,.F.);
#8821=ORIENTED_EDGE('',*,*,#6448,.T.);
#8822=ORIENTED_EDGE('',*,*,#6442,.T.);
#8823=ORIENTED_EDGE('',*,*,#6449,.F.);
#8824=ORIENTED_EDGE('',*,*,#6438,.F.);
#8825=ORIENTED_EDGE('',*,*,#6451,.T.);
#8826=ORIENTED_EDGE('',*,*,#6446,.F.);
#8827=ORIENTED_EDGE('',*,*,#6452,.F.);
#8828=ORIENTED_EDGE('',*,*,#6434,.T.);
#8829=ORIENTED_EDGE('',*,*,#6453,.T.);
#8830=ORIENTED_EDGE('',*,*,#6444,.F.);
#8831=ORIENTED_EDGE('',*,*,#6454,.F.);
#8832=ORIENTED_EDGE('',*,*,#6436,.T.);
#8833=ORIENTED_EDGE('',*,*,#6455,.T.);
#8834=ORIENTED_EDGE('',*,*,#6443,.T.);
#8835=ORIENTED_EDGE('',*,*,#6451,.F.);
#8836=ORIENTED_EDGE('',*,*,#6437,.F.);
#8837=ORIENTED_EDGE('',*,*,#6454,.T.);
#8838=ORIENTED_EDGE('',*,*,#6445,.F.);
#8839=ORIENTED_EDGE('',*,*,#6455,.F.);
#8840=ORIENTED_EDGE('',*,*,#6435,.T.);
#8841=ORIENTED_EDGE('',*,*,#6452,.T.);
#8842=ORIENTED_EDGE('',*,*,#6447,.T.);
#8843=ORIENTED_EDGE('',*,*,#6453,.F.);
#8844=ORIENTED_EDGE('',*,*,#6433,.F.);
#8845=ORIENTED_EDGE('',*,*,#6450,.T.);
#8846=ORIENTED_EDGE('',*,*,#6420,.T.);
#8847=ORIENTED_EDGE('',*,*,#6423,.T.);
#8848=ORIENTED_EDGE('',*,*,#6426,.T.);
#8849=ORIENTED_EDGE('',*,*,#6429,.T.);
#8850=ORIENTED_EDGE('',*,*,#6456,.T.);
#8851=ORIENTED_EDGE('',*,*,#6457,.T.);
#8852=ORIENTED_EDGE('',*,*,#6458,.T.);
#8853=ORIENTED_EDGE('',*,*,#6457,.F.);
#8854=ORIENTED_EDGE('',*,*,#6459,.F.);
#8855=ORIENTED_EDGE('',*,*,#6460,.T.);
#8856=ORIENTED_EDGE('',*,*,#6456,.F.);
#8857=ORIENTED_EDGE('',*,*,#6460,.F.);
#8858=ORIENTED_EDGE('',*,*,#6458,.F.);
#8859=ORIENTED_EDGE('',*,*,#6461,.T.);
#8860=ORIENTED_EDGE('',*,*,#6459,.T.);
#8861=ORIENTED_EDGE('',*,*,#6462,.T.);
#8862=ORIENTED_EDGE('',*,*,#6463,.T.);
#8863=ORIENTED_EDGE('',*,*,#6462,.F.);
#8864=ORIENTED_EDGE('',*,*,#6463,.F.);
#8865=ORIENTED_EDGE('',*,*,#6464,.T.);
#8866=ORIENTED_EDGE('',*,*,#6461,.F.);
#8867=ORIENTED_EDGE('',*,*,#6465,.T.);
#8868=ORIENTED_EDGE('',*,*,#6464,.F.);
#8869=ORIENTED_EDGE('',*,*,#6465,.F.);
#8870=ORIENTED_EDGE('',*,*,#6466,.T.);
#8871=ORIENTED_EDGE('',*,*,#6467,.T.);
#8872=ORIENTED_EDGE('',*,*,#6468,.F.);
#8873=ORIENTED_EDGE('',*,*,#6467,.F.);
#8874=ORIENTED_EDGE('',*,*,#6469,.F.);
#8875=ORIENTED_EDGE('',*,*,#6470,.T.);
#8876=ORIENTED_EDGE('',*,*,#6471,.T.);
#8877=ORIENTED_EDGE('',*,*,#6470,.F.);
#8878=ORIENTED_EDGE('',*,*,#6469,.T.);
#8879=ORIENTED_EDGE('',*,*,#6468,.T.);
#8880=ORIENTED_EDGE('',*,*,#6471,.F.);
#8881=ORIENTED_EDGE('',*,*,#6466,.F.);
#8882=ORIENTED_EDGE('',*,*,#6472,.F.);
#8883=ORIENTED_EDGE('',*,*,#6473,.T.);
#8884=ORIENTED_EDGE('',*,*,#6474,.F.);
#8885=ORIENTED_EDGE('',*,*,#6473,.F.);
#8886=ORIENTED_EDGE('',*,*,#6475,.F.);
#8887=ORIENTED_EDGE('',*,*,#6476,.T.);
#8888=ORIENTED_EDGE('',*,*,#6477,.F.);
#8889=ORIENTED_EDGE('',*,*,#6476,.F.);
#8890=ORIENTED_EDGE('',*,*,#6478,.F.);
#8891=ORIENTED_EDGE('',*,*,#6479,.F.);
#8892=ORIENTED_EDGE('',*,*,#6480,.F.);
#8893=ORIENTED_EDGE('',*,*,#6481,.F.);
#8894=ORIENTED_EDGE('',*,*,#6480,.T.);
#8895=ORIENTED_EDGE('',*,*,#6482,.F.);
#8896=ORIENTED_EDGE('',*,*,#6483,.T.);
#8897=ORIENTED_EDGE('',*,*,#6484,.F.);
#8898=ORIENTED_EDGE('',*,*,#6485,.T.);
#8899=ORIENTED_EDGE('',*,*,#6486,.T.);
#8900=ORIENTED_EDGE('',*,*,#6487,.F.);
#8901=ORIENTED_EDGE('',*,*,#6486,.F.);
#8902=ORIENTED_EDGE('',*,*,#6488,.T.);
#8903=ORIENTED_EDGE('',*,*,#6489,.T.);
#8904=ORIENTED_EDGE('',*,*,#6490,.T.);
#8905=ORIENTED_EDGE('',*,*,#6482,.T.);
#8906=ORIENTED_EDGE('',*,*,#6479,.T.);
#8907=ORIENTED_EDGE('',*,*,#6491,.T.);
#8908=ORIENTED_EDGE('',*,*,#6478,.T.);
#8909=ORIENTED_EDGE('',*,*,#6492,.F.);
#8910=ORIENTED_EDGE('',*,*,#6493,.F.);
#8911=ORIENTED_EDGE('',*,*,#6491,.F.);
#8912=ORIENTED_EDGE('',*,*,#6493,.T.);
#8913=ORIENTED_EDGE('',*,*,#6494,.F.);
#8914=ORIENTED_EDGE('',*,*,#6495,.F.);
#8915=ORIENTED_EDGE('',*,*,#6496,.F.);
#8916=ORIENTED_EDGE('',*,*,#6488,.F.);
#8917=ORIENTED_EDGE('',*,*,#6485,.F.);
#8918=ORIENTED_EDGE('',*,*,#6496,.T.);
#8919=ORIENTED_EDGE('',*,*,#6497,.F.);
#8920=ORIENTED_EDGE('',*,*,#6498,.F.);
#8921=ORIENTED_EDGE('',*,*,#6489,.F.);
#8922=ORIENTED_EDGE('',*,*,#6498,.T.);
#8923=ORIENTED_EDGE('',*,*,#6499,.F.);
#8924=ORIENTED_EDGE('',*,*,#6483,.F.);
#8925=ORIENTED_EDGE('',*,*,#6490,.F.);
#8926=ORIENTED_EDGE('',*,*,#6500,.F.);
#8927=ORIENTED_EDGE('',*,*,#6477,.T.);
#8928=ORIENTED_EDGE('',*,*,#6495,.T.);
#8929=ORIENTED_EDGE('',*,*,#6501,.T.);
#8930=ORIENTED_EDGE('',*,*,#6500,.T.);
#8931=ORIENTED_EDGE('',*,*,#6501,.F.);
#8932=ORIENTED_EDGE('',*,*,#6494,.T.);
#8933=ORIENTED_EDGE('',*,*,#6492,.T.);
#8934=ORIENTED_EDGE('',*,*,#6481,.T.);
#8935=ORIENTED_EDGE('',*,*,#6484,.T.);
#8936=ORIENTED_EDGE('',*,*,#6499,.T.);
#8937=ORIENTED_EDGE('',*,*,#6497,.T.);
#8938=ORIENTED_EDGE('',*,*,#6487,.T.);
#8939=ORIENTED_EDGE('',*,*,#6474,.T.);
#8940=ORIENTED_EDGE('',*,*,#6475,.T.);
#8941=ORIENTED_EDGE('',*,*,#6502,.T.);
#8942=ORIENTED_EDGE('',*,*,#6472,.T.);
#8943=ORIENTED_EDGE('',*,*,#6502,.F.);
#8944=ORIENTED_EDGE('',*,*,#6503,.F.);
#8945=ORIENTED_EDGE('',*,*,#6504,.T.);
#8946=ORIENTED_EDGE('',*,*,#6505,.T.);
#8947=ORIENTED_EDGE('',*,*,#6504,.F.);
#8948=ORIENTED_EDGE('',*,*,#6506,.F.);
#8949=ORIENTED_EDGE('',*,*,#6507,.T.);
#8950=ORIENTED_EDGE('',*,*,#6503,.T.);
#8951=ORIENTED_EDGE('',*,*,#6507,.F.);
#8952=ORIENTED_EDGE('',*,*,#6508,.F.);
#8953=ORIENTED_EDGE('',*,*,#6509,.T.);
#8954=ORIENTED_EDGE('',*,*,#6506,.T.);
#8955=ORIENTED_EDGE('',*,*,#6509,.F.);
#8956=ORIENTED_EDGE('',*,*,#6510,.F.);
#8957=ORIENTED_EDGE('',*,*,#6511,.T.);
#8958=ORIENTED_EDGE('',*,*,#6512,.T.);
#8959=ORIENTED_EDGE('',*,*,#6511,.F.);
#8960=ORIENTED_EDGE('',*,*,#6513,.F.);
#8961=ORIENTED_EDGE('',*,*,#6514,.F.);
#8962=ORIENTED_EDGE('',*,*,#6515,.T.);
#8963=ORIENTED_EDGE('',*,*,#6510,.T.);
#8964=ORIENTED_EDGE('',*,*,#6515,.F.);
#8965=ORIENTED_EDGE('',*,*,#6513,.T.);
#8966=ORIENTED_EDGE('',*,*,#6514,.T.);
#8967=ORIENTED_EDGE('',*,*,#6516,.T.);
#8968=ORIENTED_EDGE('',*,*,#6517,.F.);
#8969=ORIENTED_EDGE('',*,*,#6516,.F.);
#8970=ORIENTED_EDGE('',*,*,#6512,.F.);
#8971=ORIENTED_EDGE('',*,*,#6508,.T.);
#8972=ORIENTED_EDGE('',*,*,#6517,.T.);
#8973=ORIENTED_EDGE('',*,*,#6505,.F.);
#8974=ORIENTED_EDGE('',*,*,#6518,.F.);
#8975=ORIENTED_EDGE('',*,*,#6519,.T.);
#8976=ORIENTED_EDGE('',*,*,#6520,.T.);
#8977=ORIENTED_EDGE('',*,*,#6519,.F.);
#8978=ORIENTED_EDGE('',*,*,#6520,.F.);
#8979=ORIENTED_EDGE('',*,*,#6521,.T.);
#8980=ORIENTED_EDGE('',*,*,#6522,.T.);
#8981=ORIENTED_EDGE('',*,*,#6521,.F.);
#8982=ORIENTED_EDGE('',*,*,#6523,.F.);
#8983=ORIENTED_EDGE('',*,*,#6524,.T.);
#8984=ORIENTED_EDGE('',*,*,#6525,.T.);
#8985=ORIENTED_EDGE('',*,*,#6524,.F.);
#8986=ORIENTED_EDGE('',*,*,#6525,.F.);
#8987=ORIENTED_EDGE('',*,*,#6526,.T.);
#8988=ORIENTED_EDGE('',*,*,#6527,.T.);
#8989=ORIENTED_EDGE('',*,*,#6526,.F.);
#8990=ORIENTED_EDGE('',*,*,#6518,.T.);
#8991=ORIENTED_EDGE('',*,*,#6527,.F.);
#8992=ORIENTED_EDGE('',*,*,#6522,.F.);
#8993=ORIENTED_EDGE('',*,*,#6523,.T.);
#8994=ORIENTED_EDGE('',*,*,#6528,.F.);
#8995=ORIENTED_EDGE('',*,*,#6529,.T.);
#8996=ORIENTED_EDGE('',*,*,#6530,.T.);
#8997=ORIENTED_EDGE('',*,*,#6529,.F.);
#8998=ORIENTED_EDGE('',*,*,#6531,.F.);
#8999=ORIENTED_EDGE('',*,*,#6532,.F.);
#9000=ORIENTED_EDGE('',*,*,#6533,.T.);
#9001=ORIENTED_EDGE('',*,*,#6528,.T.);
#9002=ORIENTED_EDGE('',*,*,#6533,.F.);
#9003=ORIENTED_EDGE('',*,*,#6531,.T.);
#9004=ORIENTED_EDGE('',*,*,#6532,.T.);
#9005=ORIENTED_EDGE('',*,*,#6534,.T.);
#9006=ORIENTED_EDGE('',*,*,#6535,.F.);
#9007=ORIENTED_EDGE('',*,*,#6534,.F.);
#9008=ORIENTED_EDGE('',*,*,#6536,.F.);
#9009=ORIENTED_EDGE('',*,*,#6537,.T.);
#9010=ORIENTED_EDGE('',*,*,#6538,.T.);
#9011=ORIENTED_EDGE('',*,*,#6537,.F.);
#9012=ORIENTED_EDGE('',*,*,#6539,.F.);
#9013=ORIENTED_EDGE('',*,*,#6540,.T.);
#9014=ORIENTED_EDGE('',*,*,#6536,.T.);
#9015=ORIENTED_EDGE('',*,*,#6540,.F.);
#9016=ORIENTED_EDGE('',*,*,#6541,.F.);
#9017=ORIENTED_EDGE('',*,*,#6542,.T.);
#9018=ORIENTED_EDGE('',*,*,#6543,.T.);
#9019=ORIENTED_EDGE('',*,*,#6542,.F.);
#9020=ORIENTED_EDGE('',*,*,#6544,.F.);
#9021=ORIENTED_EDGE('',*,*,#6545,.T.);
#9022=ORIENTED_EDGE('',*,*,#6541,.T.);
#9023=ORIENTED_EDGE('',*,*,#6545,.F.);
#9024=ORIENTED_EDGE('',*,*,#6544,.T.);
#9025=ORIENTED_EDGE('',*,*,#6530,.F.);
#9026=ORIENTED_EDGE('',*,*,#6539,.T.);
#9027=ORIENTED_EDGE('',*,*,#6543,.F.);
#9028=ORIENTED_EDGE('',*,*,#6538,.F.);
#9029=ORIENTED_EDGE('',*,*,#6535,.T.);
#9030=ORIENTED_EDGE('',*,*,#6546,.T.);
#9031=ORIENTED_EDGE('',*,*,#6546,.F.);
#9032=ORIENTED_EDGE('',*,*,#6547,.T.);
#9033=ORIENTED_EDGE('',*,*,#6547,.F.);
#9034=ORIENTED_EDGE('',*,*,#6548,.T.);
#9035=ORIENTED_EDGE('',*,*,#6548,.F.);
#9036=ORIENTED_EDGE('',*,*,#6549,.T.);
#9037=ORIENTED_EDGE('',*,*,#6549,.F.);
#9038=ORIENTED_EDGE('',*,*,#6550,.T.);
#9039=ORIENTED_EDGE('',*,*,#6550,.F.);
#9040=ORIENTED_EDGE('',*,*,#6551,.T.);
#9041=ORIENTED_EDGE('',*,*,#6551,.F.);
#9042=ORIENTED_EDGE('',*,*,#6552,.T.);
#9043=ORIENTED_EDGE('',*,*,#6552,.F.);
#9044=ORIENTED_EDGE('',*,*,#6553,.T.);
#9045=ORIENTED_EDGE('',*,*,#6553,.F.);
#9046=ORIENTED_EDGE('',*,*,#6554,.T.);
#9047=ORIENTED_EDGE('',*,*,#6554,.F.);
#9048=ORIENTED_EDGE('',*,*,#6555,.T.);
#9049=ORIENTED_EDGE('',*,*,#6555,.F.);
#9050=ORIENTED_EDGE('',*,*,#6556,.T.);
#9051=ORIENTED_EDGE('',*,*,#6557,.T.);
#9052=ORIENTED_EDGE('',*,*,#6558,.T.);
#9053=ORIENTED_EDGE('',*,*,#6559,.F.);
#9054=ORIENTED_EDGE('',*,*,#6560,.T.);
#9055=ORIENTED_EDGE('',*,*,#6561,.T.);
#9056=ORIENTED_EDGE('',*,*,#6562,.T.);
#9057=ORIENTED_EDGE('',*,*,#6563,.F.);
#9058=ORIENTED_EDGE('',*,*,#6564,.F.);
#9059=ORIENTED_EDGE('',*,*,#6565,.F.);
#9060=ORIENTED_EDGE('',*,*,#6566,.T.);
#9061=ORIENTED_EDGE('',*,*,#6567,.T.);
#9062=ORIENTED_EDGE('',*,*,#6568,.T.);
#9063=ORIENTED_EDGE('',*,*,#6569,.T.);
#9064=ORIENTED_EDGE('',*,*,#6570,.F.);
#9065=ORIENTED_EDGE('',*,*,#6571,.F.);
#9066=ORIENTED_EDGE('',*,*,#6572,.F.);
#9067=ORIENTED_EDGE('',*,*,#6573,.F.);
#9068=ORIENTED_EDGE('',*,*,#6574,.T.);
#9069=ORIENTED_EDGE('',*,*,#6575,.T.);
#9070=ORIENTED_EDGE('',*,*,#6576,.T.);
#9071=ORIENTED_EDGE('',*,*,#6577,.T.);
#9072=ORIENTED_EDGE('',*,*,#6578,.F.);
#9073=ORIENTED_EDGE('',*,*,#6577,.F.);
#9074=ORIENTED_EDGE('',*,*,#6579,.T.);
#9075=ORIENTED_EDGE('',*,*,#6580,.T.);
#9076=ORIENTED_EDGE('',*,*,#6581,.F.);
#9077=ORIENTED_EDGE('',*,*,#6582,.F.);
#9078=ORIENTED_EDGE('',*,*,#6583,.T.);
#9079=ORIENTED_EDGE('',*,*,#6584,.T.);
#9080=ORIENTED_EDGE('',*,*,#6585,.T.);
#9081=ORIENTED_EDGE('',*,*,#6586,.F.);
#9082=ORIENTED_EDGE('',*,*,#6587,.T.);
#9083=ORIENTED_EDGE('',*,*,#6581,.T.);
#9084=ORIENTED_EDGE('',*,*,#6588,.T.);
#9085=ORIENTED_EDGE('',*,*,#6584,.F.);
#9086=ORIENTED_EDGE('',*,*,#6589,.F.);
#9087=ORIENTED_EDGE('',*,*,#6590,.T.);
#9088=ORIENTED_EDGE('',*,*,#6591,.T.);
#9089=ORIENTED_EDGE('',*,*,#6574,.F.);
#9090=ORIENTED_EDGE('',*,*,#6592,.F.);
#9091=ORIENTED_EDGE('',*,*,#6593,.T.);
#9092=ORIENTED_EDGE('',*,*,#6594,.T.);
#9093=ORIENTED_EDGE('',*,*,#6590,.F.);
#9094=ORIENTED_EDGE('',*,*,#6595,.T.);
#9095=ORIENTED_EDGE('',*,*,#6596,.T.);
#9096=ORIENTED_EDGE('',*,*,#6597,.T.);
#9097=ORIENTED_EDGE('',*,*,#6593,.F.);
#9098=ORIENTED_EDGE('',*,*,#6598,.T.);
#9099=ORIENTED_EDGE('',*,*,#6599,.T.);
#9100=ORIENTED_EDGE('',*,*,#6600,.T.);
#9101=ORIENTED_EDGE('',*,*,#6596,.F.);
#9102=ORIENTED_EDGE('',*,*,#6601,.F.);
#9103=ORIENTED_EDGE('',*,*,#6602,.T.);
#9104=ORIENTED_EDGE('',*,*,#6603,.T.);
#9105=ORIENTED_EDGE('',*,*,#6599,.F.);
#9106=ORIENTED_EDGE('',*,*,#6604,.F.);
#9107=ORIENTED_EDGE('',*,*,#6605,.T.);
#9108=ORIENTED_EDGE('',*,*,#6606,.T.);
#9109=ORIENTED_EDGE('',*,*,#6602,.F.);
#9110=ORIENTED_EDGE('',*,*,#6607,.F.);
#9111=ORIENTED_EDGE('',*,*,#6608,.T.);
#9112=ORIENTED_EDGE('',*,*,#6609,.T.);
#9113=ORIENTED_EDGE('',*,*,#6605,.F.);
#9114=ORIENTED_EDGE('',*,*,#6610,.F.);
#9115=ORIENTED_EDGE('',*,*,#6611,.T.);
#9116=ORIENTED_EDGE('',*,*,#6612,.T.);
#9117=ORIENTED_EDGE('',*,*,#6608,.F.);
#9118=ORIENTED_EDGE('',*,*,#6613,.T.);
#9119=ORIENTED_EDGE('',*,*,#6614,.T.);
#9120=ORIENTED_EDGE('',*,*,#6615,.T.);
#9121=ORIENTED_EDGE('',*,*,#6611,.F.);
#9122=ORIENTED_EDGE('',*,*,#6616,.F.);
#9123=ORIENTED_EDGE('',*,*,#6617,.T.);
#9124=ORIENTED_EDGE('',*,*,#6618,.T.);
#9125=ORIENTED_EDGE('',*,*,#6614,.F.);
#9126=ORIENTED_EDGE('',*,*,#6619,.F.);
#9127=ORIENTED_EDGE('',*,*,#6586,.T.);
#9128=ORIENTED_EDGE('',*,*,#6620,.T.);
#9129=ORIENTED_EDGE('',*,*,#6617,.F.);
#9130=ORIENTED_EDGE('',*,*,#6621,.T.);
#9131=ORIENTED_EDGE('',*,*,#6622,.T.);
#9132=ORIENTED_EDGE('',*,*,#6623,.T.);
#9133=ORIENTED_EDGE('',*,*,#6624,.F.);
#9134=ORIENTED_EDGE('',*,*,#6625,.T.);
#9135=ORIENTED_EDGE('',*,*,#6570,.T.);
#9136=ORIENTED_EDGE('',*,*,#6626,.T.);
#9137=ORIENTED_EDGE('',*,*,#6622,.F.);
#9138=ORIENTED_EDGE('',*,*,#6627,.F.);
#9139=ORIENTED_EDGE('',*,*,#6563,.T.);
#9140=ORIENTED_EDGE('',*,*,#6628,.T.);
#9141=ORIENTED_EDGE('',*,*,#6566,.F.);
#9142=ORIENTED_EDGE('',*,*,#6629,.T.);
#9143=ORIENTED_EDGE('',*,*,#6630,.T.);
#9144=ORIENTED_EDGE('',*,*,#6631,.T.);
#9145=ORIENTED_EDGE('',*,*,#6632,.F.);
#9146=ORIENTED_EDGE('',*,*,#6633,.F.);
#9147=ORIENTED_EDGE('',*,*,#6634,.T.);
#9148=ORIENTED_EDGE('',*,*,#6635,.T.);
#9149=ORIENTED_EDGE('',*,*,#6630,.F.);
#9150=ORIENTED_EDGE('',*,*,#6636,.F.);
#9151=ORIENTED_EDGE('',*,*,#6624,.T.);
#9152=ORIENTED_EDGE('',*,*,#6637,.T.);
#9153=ORIENTED_EDGE('',*,*,#6634,.F.);
#9154=ORIENTED_EDGE('',*,*,#6638,.T.);
#9155=ORIENTED_EDGE('',*,*,#6639,.T.);
#9156=ORIENTED_EDGE('',*,*,#6640,.T.);
#9157=ORIENTED_EDGE('',*,*,#6641,.F.);
#9158=ORIENTED_EDGE('',*,*,#6642,.T.);
#9159=ORIENTED_EDGE('',*,*,#6572,.T.);
#9160=ORIENTED_EDGE('',*,*,#6643,.T.);
#9161=ORIENTED_EDGE('',*,*,#6639,.F.);
#9162=ORIENTED_EDGE('',*,*,#6644,.F.);
#9163=ORIENTED_EDGE('',*,*,#6645,.T.);
#9164=ORIENTED_EDGE('',*,*,#6646,.T.);
#9165=ORIENTED_EDGE('',*,*,#6568,.F.);
#9166=ORIENTED_EDGE('',*,*,#6647,.F.);
#9167=ORIENTED_EDGE('',*,*,#6648,.T.);
#9168=ORIENTED_EDGE('',*,*,#6649,.T.);
#9169=ORIENTED_EDGE('',*,*,#6645,.F.);
#9170=ORIENTED_EDGE('',*,*,#6650,.T.);
#9171=ORIENTED_EDGE('',*,*,#6651,.T.);
#9172=ORIENTED_EDGE('',*,*,#6652,.T.);
#9173=ORIENTED_EDGE('',*,*,#6648,.F.);
#9174=ORIENTED_EDGE('',*,*,#6653,.T.);
#9175=ORIENTED_EDGE('',*,*,#6654,.T.);
#9176=ORIENTED_EDGE('',*,*,#6655,.T.);
#9177=ORIENTED_EDGE('',*,*,#6651,.F.);
#9178=ORIENTED_EDGE('',*,*,#6656,.F.);
#9179=ORIENTED_EDGE('',*,*,#6657,.T.);
#9180=ORIENTED_EDGE('',*,*,#6658,.T.);
#9181=ORIENTED_EDGE('',*,*,#6654,.F.);
#9182=ORIENTED_EDGE('',*,*,#6659,.F.);
#9183=ORIENTED_EDGE('',*,*,#6660,.T.);
#9184=ORIENTED_EDGE('',*,*,#6661,.T.);
#9185=ORIENTED_EDGE('',*,*,#6657,.F.);
#9186=ORIENTED_EDGE('',*,*,#6662,.F.);
#9187=ORIENTED_EDGE('',*,*,#6663,.T.);
#9188=ORIENTED_EDGE('',*,*,#6664,.T.);
#9189=ORIENTED_EDGE('',*,*,#6660,.F.);
#9190=ORIENTED_EDGE('',*,*,#6665,.F.);
#9191=ORIENTED_EDGE('',*,*,#6666,.T.);
#9192=ORIENTED_EDGE('',*,*,#6667,.T.);
#9193=ORIENTED_EDGE('',*,*,#6663,.F.);
#9194=ORIENTED_EDGE('',*,*,#6668,.T.);
#9195=ORIENTED_EDGE('',*,*,#6669,.T.);
#9196=ORIENTED_EDGE('',*,*,#6670,.T.);
#9197=ORIENTED_EDGE('',*,*,#6666,.F.);
#9198=ORIENTED_EDGE('',*,*,#6671,.F.);
#9199=ORIENTED_EDGE('',*,*,#6672,.T.);
#9200=ORIENTED_EDGE('',*,*,#6673,.T.);
#9201=ORIENTED_EDGE('',*,*,#6669,.F.);
#9202=ORIENTED_EDGE('',*,*,#6674,.F.);
#9203=ORIENTED_EDGE('',*,*,#6641,.T.);
#9204=ORIENTED_EDGE('',*,*,#6675,.T.);
#9205=ORIENTED_EDGE('',*,*,#6672,.F.);
#9206=ORIENTED_EDGE('',*,*,#6676,.T.);
#9207=ORIENTED_EDGE('',*,*,#6564,.T.);
#9208=ORIENTED_EDGE('',*,*,#6677,.T.);
#9209=ORIENTED_EDGE('',*,*,#6557,.F.);
#9210=ORIENTED_EDGE('',*,*,#6678,.F.);
#9211=ORIENTED_EDGE('',*,*,#6679,.T.);
#9212=ORIENTED_EDGE('',*,*,#6680,.T.);
#9213=ORIENTED_EDGE('',*,*,#6579,.F.);
#9214=ORIENTED_EDGE('',*,*,#6681,.F.);
#9215=ORIENTED_EDGE('',*,*,#6682,.T.);
#9216=ORIENTED_EDGE('',*,*,#6683,.T.);
#9217=ORIENTED_EDGE('',*,*,#6679,.F.);
#9218=ORIENTED_EDGE('',*,*,#6684,.T.);
#9219=ORIENTED_EDGE('',*,*,#6685,.T.);
#9220=ORIENTED_EDGE('',*,*,#6686,.T.);
#9221=ORIENTED_EDGE('',*,*,#6682,.F.);
#9222=ORIENTED_EDGE('',*,*,#6687,.T.);
#9223=ORIENTED_EDGE('',*,*,#6688,.T.);
#9224=ORIENTED_EDGE('',*,*,#6689,.T.);
#9225=ORIENTED_EDGE('',*,*,#6685,.F.);
#9226=ORIENTED_EDGE('',*,*,#6690,.F.);
#9227=ORIENTED_EDGE('',*,*,#6691,.T.);
#9228=ORIENTED_EDGE('',*,*,#6692,.T.);
#9229=ORIENTED_EDGE('',*,*,#6688,.F.);
#9230=ORIENTED_EDGE('',*,*,#6693,.F.);
#9231=ORIENTED_EDGE('',*,*,#6559,.T.);
#9232=ORIENTED_EDGE('',*,*,#6694,.T.);
#9233=ORIENTED_EDGE('',*,*,#6695,.F.);
#9234=ORIENTED_EDGE('',*,*,#6696,.F.);
#9235=ORIENTED_EDGE('',*,*,#6695,.T.);
#9236=ORIENTED_EDGE('',*,*,#6697,.F.);
#9237=ORIENTED_EDGE('',*,*,#6698,.F.);
#9238=ORIENTED_EDGE('',*,*,#6699,.T.);
#9239=ORIENTED_EDGE('',*,*,#6690,.T.);
#9240=ORIENTED_EDGE('',*,*,#6687,.F.);
#9241=ORIENTED_EDGE('',*,*,#6684,.F.);
#9242=ORIENTED_EDGE('',*,*,#6681,.T.);
#9243=ORIENTED_EDGE('',*,*,#6678,.T.);
#9244=ORIENTED_EDGE('',*,*,#6582,.T.);
#9245=ORIENTED_EDGE('',*,*,#6587,.F.);
#9246=ORIENTED_EDGE('',*,*,#6583,.F.);
#9247=ORIENTED_EDGE('',*,*,#6619,.T.);
#9248=ORIENTED_EDGE('',*,*,#6616,.T.);
#9249=ORIENTED_EDGE('',*,*,#6613,.F.);
#9250=ORIENTED_EDGE('',*,*,#6610,.T.);
#9251=ORIENTED_EDGE('',*,*,#6607,.T.);
#9252=ORIENTED_EDGE('',*,*,#6604,.T.);
#9253=ORIENTED_EDGE('',*,*,#6601,.T.);
#9254=ORIENTED_EDGE('',*,*,#6598,.F.);
#9255=ORIENTED_EDGE('',*,*,#6595,.F.);
#9256=ORIENTED_EDGE('',*,*,#6592,.T.);
#9257=ORIENTED_EDGE('',*,*,#6589,.T.);
#9258=ORIENTED_EDGE('',*,*,#6573,.T.);
#9259=ORIENTED_EDGE('',*,*,#6642,.F.);
#9260=ORIENTED_EDGE('',*,*,#6638,.F.);
#9261=ORIENTED_EDGE('',*,*,#6674,.T.);
#9262=ORIENTED_EDGE('',*,*,#6671,.T.);
#9263=ORIENTED_EDGE('',*,*,#6668,.F.);
#9264=ORIENTED_EDGE('',*,*,#6665,.T.);
#9265=ORIENTED_EDGE('',*,*,#6662,.T.);
#9266=ORIENTED_EDGE('',*,*,#6659,.T.);
#9267=ORIENTED_EDGE('',*,*,#6656,.T.);
#9268=ORIENTED_EDGE('',*,*,#6653,.F.);
#9269=ORIENTED_EDGE('',*,*,#6650,.F.);
#9270=ORIENTED_EDGE('',*,*,#6647,.T.);
#9271=ORIENTED_EDGE('',*,*,#6644,.T.);
#9272=ORIENTED_EDGE('',*,*,#6571,.T.);
#9273=ORIENTED_EDGE('',*,*,#6625,.F.);
#9274=ORIENTED_EDGE('',*,*,#6621,.F.);
#9275=ORIENTED_EDGE('',*,*,#6636,.T.);
#9276=ORIENTED_EDGE('',*,*,#6633,.T.);
#9277=ORIENTED_EDGE('',*,*,#6629,.F.);
#9278=ORIENTED_EDGE('',*,*,#6700,.F.);
#9279=ORIENTED_EDGE('',*,*,#6701,.T.);
#9280=ORIENTED_EDGE('',*,*,#6702,.F.);
#9281=ORIENTED_EDGE('',*,*,#6703,.F.);
#9282=ORIENTED_EDGE('',*,*,#6704,.T.);
#9283=ORIENTED_EDGE('',*,*,#6705,.T.);
#9284=ORIENTED_EDGE('',*,*,#6706,.F.);
#9285=ORIENTED_EDGE('',*,*,#6707,.F.);
#9286=ORIENTED_EDGE('',*,*,#6708,.F.);
#9287=ORIENTED_EDGE('',*,*,#6709,.T.);
#9288=ORIENTED_EDGE('',*,*,#6710,.T.);
#9289=ORIENTED_EDGE('',*,*,#6711,.F.);
#9290=ORIENTED_EDGE('',*,*,#6712,.F.);
#9291=ORIENTED_EDGE('',*,*,#6713,.F.);
#9292=ORIENTED_EDGE('',*,*,#6714,.F.);
#9293=ORIENTED_EDGE('',*,*,#6715,.T.);
#9294=ORIENTED_EDGE('',*,*,#6716,.F.);
#9295=ORIENTED_EDGE('',*,*,#6717,.F.);
#9296=ORIENTED_EDGE('',*,*,#6718,.T.);
#9297=ORIENTED_EDGE('',*,*,#6719,.T.);
#9298=ORIENTED_EDGE('',*,*,#6720,.F.);
#9299=ORIENTED_EDGE('',*,*,#6721,.F.);
#9300=ORIENTED_EDGE('',*,*,#6722,.F.);
#9301=ORIENTED_EDGE('',*,*,#6723,.T.);
#9302=ORIENTED_EDGE('',*,*,#6724,.T.);
#9303=ORIENTED_EDGE('',*,*,#6725,.F.);
#9304=ORIENTED_EDGE('',*,*,#6726,.F.);
#9305=ORIENTED_EDGE('',*,*,#6727,.F.);
#9306=ORIENTED_EDGE('',*,*,#6728,.F.);
#9307=ORIENTED_EDGE('',*,*,#6729,.T.);
#9308=ORIENTED_EDGE('',*,*,#6730,.F.);
#9309=ORIENTED_EDGE('',*,*,#6731,.F.);
#9310=ORIENTED_EDGE('',*,*,#6732,.T.);
#9311=ORIENTED_EDGE('',*,*,#6733,.T.);
#9312=ORIENTED_EDGE('',*,*,#6734,.F.);
#9313=ORIENTED_EDGE('',*,*,#6735,.F.);
#9314=ORIENTED_EDGE('',*,*,#6736,.F.);
#9315=ORIENTED_EDGE('',*,*,#6737,.T.);
#9316=ORIENTED_EDGE('',*,*,#6738,.T.);
#9317=ORIENTED_EDGE('',*,*,#6739,.F.);
#9318=ORIENTED_EDGE('',*,*,#6693,.T.);
#9319=ORIENTED_EDGE('',*,*,#6696,.T.);
#9320=ORIENTED_EDGE('',*,*,#6740,.T.);
#9321=ORIENTED_EDGE('',*,*,#6741,.F.);
#9322=ORIENTED_EDGE('',*,*,#6742,.F.);
#9323=ORIENTED_EDGE('',*,*,#6743,.T.);
#9324=ORIENTED_EDGE('',*,*,#6744,.T.);
#9325=ORIENTED_EDGE('',*,*,#6560,.F.);
#9326=ORIENTED_EDGE('',*,*,#6627,.T.);
#9327=ORIENTED_EDGE('',*,*,#6565,.T.);
#9328=ORIENTED_EDGE('',*,*,#6676,.F.);
#9329=ORIENTED_EDGE('',*,*,#6556,.F.);
#9330=ORIENTED_EDGE('',*,*,#6578,.T.);
#9331=ORIENTED_EDGE('',*,*,#6745,.F.);
#9332=ORIENTED_EDGE('',*,*,#6744,.F.);
#9333=ORIENTED_EDGE('',*,*,#6746,.T.);
#9334=ORIENTED_EDGE('',*,*,#6747,.T.);
#9335=ORIENTED_EDGE('',*,*,#6561,.F.);
#9336=ORIENTED_EDGE('',*,*,#6743,.F.);
#9337=ORIENTED_EDGE('',*,*,#6748,.T.);
#9338=ORIENTED_EDGE('',*,*,#6749,.F.);
#9339=ORIENTED_EDGE('',*,*,#6746,.F.);
#9340=ORIENTED_EDGE('',*,*,#6750,.T.);
#9341=ORIENTED_EDGE('',*,*,#6751,.F.);
#9342=ORIENTED_EDGE('',*,*,#6752,.F.);
#9343=ORIENTED_EDGE('',*,*,#6741,.T.);
#9344=ORIENTED_EDGE('',*,*,#6753,.F.);
#9345=ORIENTED_EDGE('',*,*,#6706,.T.);
#9346=ORIENTED_EDGE('',*,*,#6754,.T.);
#9347=ORIENTED_EDGE('',*,*,#6755,.F.);
#9348=ORIENTED_EDGE('',*,*,#6756,.T.);
#9349=ORIENTED_EDGE('',*,*,#6757,.F.);
#9350=ORIENTED_EDGE('',*,*,#6758,.F.);
#9351=ORIENTED_EDGE('',*,*,#6720,.T.);
#9352=ORIENTED_EDGE('',*,*,#6745,.T.);
#9353=ORIENTED_EDGE('',*,*,#6759,.T.);
#9354=ORIENTED_EDGE('',*,*,#6760,.F.);
#9355=ORIENTED_EDGE('',*,*,#6759,.F.);
#9356=ORIENTED_EDGE('',*,*,#6761,.F.);
#9357=ORIENTED_EDGE('',*,*,#6734,.T.);
#9358=ORIENTED_EDGE('',*,*,#6762,.T.);
#9359=ORIENTED_EDGE('',*,*,#6763,.F.);
#9360=ORIENTED_EDGE('',*,*,#6732,.F.);
#9361=ORIENTED_EDGE('',*,*,#6764,.T.);
#9362=ORIENTED_EDGE('',*,*,#6765,.F.);
#9363=ORIENTED_EDGE('',*,*,#6766,.F.);
#9364=ORIENTED_EDGE('',*,*,#6733,.F.);
#9365=ORIENTED_EDGE('',*,*,#6766,.T.);
#9366=ORIENTED_EDGE('',*,*,#6767,.F.);
#9367=ORIENTED_EDGE('',*,*,#6762,.F.);
#9368=ORIENTED_EDGE('',*,*,#6721,.T.);
#9369=ORIENTED_EDGE('',*,*,#6758,.T.);
#9370=ORIENTED_EDGE('',*,*,#6768,.F.);
#9371=ORIENTED_EDGE('',*,*,#6769,.F.);
#9372=ORIENTED_EDGE('',*,*,#6722,.T.);
#9373=ORIENTED_EDGE('',*,*,#6769,.T.);
#9374=ORIENTED_EDGE('',*,*,#6770,.F.);
#9375=ORIENTED_EDGE('',*,*,#6771,.F.);
#9376=ORIENTED_EDGE('',*,*,#6723,.F.);
#9377=ORIENTED_EDGE('',*,*,#6771,.T.);
#9378=ORIENTED_EDGE('',*,*,#6772,.F.);
#9379=ORIENTED_EDGE('',*,*,#6773,.F.);
#9380=ORIENTED_EDGE('',*,*,#6724,.F.);
#9381=ORIENTED_EDGE('',*,*,#6773,.T.);
#9382=ORIENTED_EDGE('',*,*,#6774,.F.);
#9383=ORIENTED_EDGE('',*,*,#6775,.F.);
#9384=ORIENTED_EDGE('',*,*,#6725,.T.);
#9385=ORIENTED_EDGE('',*,*,#6775,.T.);
#9386=ORIENTED_EDGE('',*,*,#6776,.F.);
#9387=ORIENTED_EDGE('',*,*,#6777,.F.);
#9388=ORIENTED_EDGE('',*,*,#6726,.T.);
#9389=ORIENTED_EDGE('',*,*,#6777,.T.);
#9390=ORIENTED_EDGE('',*,*,#6778,.F.);
#9391=ORIENTED_EDGE('',*,*,#6779,.F.);
#9392=ORIENTED_EDGE('',*,*,#6727,.T.);
#9393=ORIENTED_EDGE('',*,*,#6779,.T.);
#9394=ORIENTED_EDGE('',*,*,#6780,.F.);
#9395=ORIENTED_EDGE('',*,*,#6781,.F.);
#9396=ORIENTED_EDGE('',*,*,#6728,.T.);
#9397=ORIENTED_EDGE('',*,*,#6781,.T.);
#9398=ORIENTED_EDGE('',*,*,#6782,.F.);
#9399=ORIENTED_EDGE('',*,*,#6783,.F.);
#9400=ORIENTED_EDGE('',*,*,#6729,.F.);
#9401=ORIENTED_EDGE('',*,*,#6783,.T.);
#9402=ORIENTED_EDGE('',*,*,#6784,.F.);
#9403=ORIENTED_EDGE('',*,*,#6785,.F.);
#9404=ORIENTED_EDGE('',*,*,#6730,.T.);
#9405=ORIENTED_EDGE('',*,*,#6785,.T.);
#9406=ORIENTED_EDGE('',*,*,#6786,.F.);
#9407=ORIENTED_EDGE('',*,*,#6787,.F.);
#9408=ORIENTED_EDGE('',*,*,#6731,.T.);
#9409=ORIENTED_EDGE('',*,*,#6787,.T.);
#9410=ORIENTED_EDGE('',*,*,#6788,.F.);
#9411=ORIENTED_EDGE('',*,*,#6764,.F.);
#9412=ORIENTED_EDGE('',*,*,#6704,.F.);
#9413=ORIENTED_EDGE('',*,*,#6789,.T.);
#9414=ORIENTED_EDGE('',*,*,#6790,.F.);
#9415=ORIENTED_EDGE('',*,*,#6791,.F.);
#9416=ORIENTED_EDGE('',*,*,#6705,.F.);
#9417=ORIENTED_EDGE('',*,*,#6791,.T.);
#9418=ORIENTED_EDGE('',*,*,#6792,.F.);
#9419=ORIENTED_EDGE('',*,*,#6754,.F.);
#9420=ORIENTED_EDGE('',*,*,#6742,.T.);
#9421=ORIENTED_EDGE('',*,*,#6752,.T.);
#9422=ORIENTED_EDGE('',*,*,#6793,.F.);
#9423=ORIENTED_EDGE('',*,*,#6748,.F.);
#9424=ORIENTED_EDGE('',*,*,#6700,.T.);
#9425=ORIENTED_EDGE('',*,*,#6632,.T.);
#9426=ORIENTED_EDGE('',*,*,#6794,.F.);
#9427=ORIENTED_EDGE('',*,*,#6795,.F.);
#9428=ORIENTED_EDGE('',*,*,#6701,.F.);
#9429=ORIENTED_EDGE('',*,*,#6795,.T.);
#9430=ORIENTED_EDGE('',*,*,#6796,.F.);
#9431=ORIENTED_EDGE('',*,*,#6797,.F.);
#9432=ORIENTED_EDGE('',*,*,#6702,.T.);
#9433=ORIENTED_EDGE('',*,*,#6797,.T.);
#9434=ORIENTED_EDGE('',*,*,#6798,.F.);
#9435=ORIENTED_EDGE('',*,*,#6799,.F.);
#9436=ORIENTED_EDGE('',*,*,#6703,.T.);
#9437=ORIENTED_EDGE('',*,*,#6799,.T.);
#9438=ORIENTED_EDGE('',*,*,#6800,.F.);
#9439=ORIENTED_EDGE('',*,*,#6789,.F.);
#9440=ORIENTED_EDGE('',*,*,#6718,.F.);
#9441=ORIENTED_EDGE('',*,*,#6801,.T.);
#9442=ORIENTED_EDGE('',*,*,#6802,.F.);
#9443=ORIENTED_EDGE('',*,*,#6803,.F.);
#9444=ORIENTED_EDGE('',*,*,#6719,.F.);
#9445=ORIENTED_EDGE('',*,*,#6803,.T.);
#9446=ORIENTED_EDGE('',*,*,#6804,.F.);
#9447=ORIENTED_EDGE('',*,*,#6756,.F.);
#9448=ORIENTED_EDGE('',*,*,#6707,.T.);
#9449=ORIENTED_EDGE('',*,*,#6753,.T.);
#9450=ORIENTED_EDGE('',*,*,#6805,.F.);
#9451=ORIENTED_EDGE('',*,*,#6806,.F.);
#9452=ORIENTED_EDGE('',*,*,#6708,.T.);
#9453=ORIENTED_EDGE('',*,*,#6806,.T.);
#9454=ORIENTED_EDGE('',*,*,#6807,.F.);
#9455=ORIENTED_EDGE('',*,*,#6808,.F.);
#9456=ORIENTED_EDGE('',*,*,#6709,.F.);
#9457=ORIENTED_EDGE('',*,*,#6808,.T.);
#9458=ORIENTED_EDGE('',*,*,#6809,.F.);
#9459=ORIENTED_EDGE('',*,*,#6810,.F.);
#9460=ORIENTED_EDGE('',*,*,#6710,.F.);
#9461=ORIENTED_EDGE('',*,*,#6810,.T.);
#9462=ORIENTED_EDGE('',*,*,#6811,.F.);
#9463=ORIENTED_EDGE('',*,*,#6812,.F.);
#9464=ORIENTED_EDGE('',*,*,#6711,.T.);
#9465=ORIENTED_EDGE('',*,*,#6812,.T.);
#9466=ORIENTED_EDGE('',*,*,#6813,.F.);
#9467=ORIENTED_EDGE('',*,*,#6814,.F.);
#9468=ORIENTED_EDGE('',*,*,#6712,.T.);
#9469=ORIENTED_EDGE('',*,*,#6814,.T.);
#9470=ORIENTED_EDGE('',*,*,#6815,.F.);
#9471=ORIENTED_EDGE('',*,*,#6816,.F.);
#9472=ORIENTED_EDGE('',*,*,#6713,.T.);
#9473=ORIENTED_EDGE('',*,*,#6816,.T.);
#9474=ORIENTED_EDGE('',*,*,#6817,.F.);
#9475=ORIENTED_EDGE('',*,*,#6818,.F.);
#9476=ORIENTED_EDGE('',*,*,#6714,.T.);
#9477=ORIENTED_EDGE('',*,*,#6818,.T.);
#9478=ORIENTED_EDGE('',*,*,#6819,.F.);
#9479=ORIENTED_EDGE('',*,*,#6820,.F.);
#9480=ORIENTED_EDGE('',*,*,#6715,.F.);
#9481=ORIENTED_EDGE('',*,*,#6820,.T.);
#9482=ORIENTED_EDGE('',*,*,#6821,.F.);
#9483=ORIENTED_EDGE('',*,*,#6822,.F.);
#9484=ORIENTED_EDGE('',*,*,#6716,.T.);
#9485=ORIENTED_EDGE('',*,*,#6822,.T.);
#9486=ORIENTED_EDGE('',*,*,#6823,.F.);
#9487=ORIENTED_EDGE('',*,*,#6824,.F.);
#9488=ORIENTED_EDGE('',*,*,#6717,.T.);
#9489=ORIENTED_EDGE('',*,*,#6824,.T.);
#9490=ORIENTED_EDGE('',*,*,#6825,.F.);
#9491=ORIENTED_EDGE('',*,*,#6801,.F.);
#9492=ORIENTED_EDGE('',*,*,#6740,.F.);
#9493=ORIENTED_EDGE('',*,*,#6698,.T.);
#9494=ORIENTED_EDGE('',*,*,#6826,.F.);
#9495=ORIENTED_EDGE('',*,*,#6750,.F.);
#9496=ORIENTED_EDGE('',*,*,#6735,.T.);
#9497=ORIENTED_EDGE('',*,*,#6761,.T.);
#9498=ORIENTED_EDGE('',*,*,#6827,.F.);
#9499=ORIENTED_EDGE('',*,*,#6828,.F.);
#9500=ORIENTED_EDGE('',*,*,#6736,.T.);
#9501=ORIENTED_EDGE('',*,*,#6828,.T.);
#9502=ORIENTED_EDGE('',*,*,#6829,.F.);
#9503=ORIENTED_EDGE('',*,*,#6830,.F.);
#9504=ORIENTED_EDGE('',*,*,#6737,.F.);
#9505=ORIENTED_EDGE('',*,*,#6830,.T.);
#9506=ORIENTED_EDGE('',*,*,#6831,.F.);
#9507=ORIENTED_EDGE('',*,*,#6832,.F.);
#9508=ORIENTED_EDGE('',*,*,#6738,.F.);
#9509=ORIENTED_EDGE('',*,*,#6832,.T.);
#9510=ORIENTED_EDGE('',*,*,#6833,.F.);
#9511=ORIENTED_EDGE('',*,*,#6834,.F.);
#9512=ORIENTED_EDGE('',*,*,#6739,.T.);
#9513=ORIENTED_EDGE('',*,*,#6834,.T.);
#9514=ORIENTED_EDGE('',*,*,#6835,.F.);
#9515=ORIENTED_EDGE('',*,*,#6836,.F.);
#9516=ORIENTED_EDGE('',*,*,#6699,.F.);
#9517=ORIENTED_EDGE('',*,*,#6836,.T.);
#9518=ORIENTED_EDGE('',*,*,#6837,.T.);
#9519=ORIENTED_EDGE('',*,*,#6691,.F.);
#9520=ORIENTED_EDGE('',*,*,#6837,.F.);
#9521=ORIENTED_EDGE('',*,*,#6835,.T.);
#9522=ORIENTED_EDGE('',*,*,#6833,.T.);
#9523=ORIENTED_EDGE('',*,*,#6831,.T.);
#9524=ORIENTED_EDGE('',*,*,#6829,.T.);
#9525=ORIENTED_EDGE('',*,*,#6827,.T.);
#9526=ORIENTED_EDGE('',*,*,#6763,.T.);
#9527=ORIENTED_EDGE('',*,*,#6767,.T.);
#9528=ORIENTED_EDGE('',*,*,#6765,.T.);
#9529=ORIENTED_EDGE('',*,*,#6788,.T.);
#9530=ORIENTED_EDGE('',*,*,#6786,.T.);
#9531=ORIENTED_EDGE('',*,*,#6784,.T.);
#9532=ORIENTED_EDGE('',*,*,#6782,.T.);
#9533=ORIENTED_EDGE('',*,*,#6780,.T.);
#9534=ORIENTED_EDGE('',*,*,#6778,.T.);
#9535=ORIENTED_EDGE('',*,*,#6776,.T.);
#9536=ORIENTED_EDGE('',*,*,#6774,.T.);
#9537=ORIENTED_EDGE('',*,*,#6772,.T.);
#9538=ORIENTED_EDGE('',*,*,#6770,.T.);
#9539=ORIENTED_EDGE('',*,*,#6768,.T.);
#9540=ORIENTED_EDGE('',*,*,#6757,.T.);
#9541=ORIENTED_EDGE('',*,*,#6804,.T.);
#9542=ORIENTED_EDGE('',*,*,#6802,.T.);
#9543=ORIENTED_EDGE('',*,*,#6825,.T.);
#9544=ORIENTED_EDGE('',*,*,#6823,.T.);
#9545=ORIENTED_EDGE('',*,*,#6821,.T.);
#9546=ORIENTED_EDGE('',*,*,#6819,.T.);
#9547=ORIENTED_EDGE('',*,*,#6817,.T.);
#9548=ORIENTED_EDGE('',*,*,#6815,.T.);
#9549=ORIENTED_EDGE('',*,*,#6813,.T.);
#9550=ORIENTED_EDGE('',*,*,#6811,.T.);
#9551=ORIENTED_EDGE('',*,*,#6809,.T.);
#9552=ORIENTED_EDGE('',*,*,#6807,.T.);
#9553=ORIENTED_EDGE('',*,*,#6805,.T.);
#9554=ORIENTED_EDGE('',*,*,#6755,.T.);
#9555=ORIENTED_EDGE('',*,*,#6792,.T.);
#9556=ORIENTED_EDGE('',*,*,#6790,.T.);
#9557=ORIENTED_EDGE('',*,*,#6800,.T.);
#9558=ORIENTED_EDGE('',*,*,#6798,.T.);
#9559=ORIENTED_EDGE('',*,*,#6796,.T.);
#9560=ORIENTED_EDGE('',*,*,#6794,.T.);
#9561=ORIENTED_EDGE('',*,*,#6631,.F.);
#9562=ORIENTED_EDGE('',*,*,#6635,.F.);
#9563=ORIENTED_EDGE('',*,*,#6637,.F.);
#9564=ORIENTED_EDGE('',*,*,#6623,.F.);
#9565=ORIENTED_EDGE('',*,*,#6626,.F.);
#9566=ORIENTED_EDGE('',*,*,#6569,.F.);
#9567=ORIENTED_EDGE('',*,*,#6646,.F.);
#9568=ORIENTED_EDGE('',*,*,#6649,.F.);
#9569=ORIENTED_EDGE('',*,*,#6652,.F.);
#9570=ORIENTED_EDGE('',*,*,#6655,.F.);
#9571=ORIENTED_EDGE('',*,*,#6658,.F.);
#9572=ORIENTED_EDGE('',*,*,#6661,.F.);
#9573=ORIENTED_EDGE('',*,*,#6664,.F.);
#9574=ORIENTED_EDGE('',*,*,#6667,.F.);
#9575=ORIENTED_EDGE('',*,*,#6670,.F.);
#9576=ORIENTED_EDGE('',*,*,#6673,.F.);
#9577=ORIENTED_EDGE('',*,*,#6675,.F.);
#9578=ORIENTED_EDGE('',*,*,#6640,.F.);
#9579=ORIENTED_EDGE('',*,*,#6643,.F.);
#9580=ORIENTED_EDGE('',*,*,#6575,.F.);
#9581=ORIENTED_EDGE('',*,*,#6591,.F.);
#9582=ORIENTED_EDGE('',*,*,#6594,.F.);
#9583=ORIENTED_EDGE('',*,*,#6597,.F.);
#9584=ORIENTED_EDGE('',*,*,#6600,.F.);
#9585=ORIENTED_EDGE('',*,*,#6603,.F.);
#9586=ORIENTED_EDGE('',*,*,#6606,.F.);
#9587=ORIENTED_EDGE('',*,*,#6609,.F.);
#9588=ORIENTED_EDGE('',*,*,#6612,.F.);
#9589=ORIENTED_EDGE('',*,*,#6615,.F.);
#9590=ORIENTED_EDGE('',*,*,#6618,.F.);
#9591=ORIENTED_EDGE('',*,*,#6620,.F.);
#9592=ORIENTED_EDGE('',*,*,#6585,.F.);
#9593=ORIENTED_EDGE('',*,*,#6588,.F.);
#9594=ORIENTED_EDGE('',*,*,#6580,.F.);
#9595=ORIENTED_EDGE('',*,*,#6680,.F.);
#9596=ORIENTED_EDGE('',*,*,#6683,.F.);
#9597=ORIENTED_EDGE('',*,*,#6686,.F.);
#9598=ORIENTED_EDGE('',*,*,#6689,.F.);
#9599=ORIENTED_EDGE('',*,*,#6692,.F.);
#9600=ORIENTED_EDGE('',*,*,#6576,.F.);
#9601=ORIENTED_EDGE('',*,*,#6694,.F.);
#9602=ORIENTED_EDGE('',*,*,#6558,.F.);
#9603=ORIENTED_EDGE('',*,*,#6677,.F.);
#9604=ORIENTED_EDGE('',*,*,#6567,.F.);
#9605=ORIENTED_EDGE('',*,*,#6628,.F.);
#9606=ORIENTED_EDGE('',*,*,#6562,.F.);
#9607=ORIENTED_EDGE('',*,*,#6747,.F.);
#9608=ORIENTED_EDGE('',*,*,#6749,.T.);
#9609=ORIENTED_EDGE('',*,*,#6793,.T.);
#9610=ORIENTED_EDGE('',*,*,#6751,.T.);
#9611=ORIENTED_EDGE('',*,*,#6826,.T.);
#9612=ORIENTED_EDGE('',*,*,#6697,.T.);
#9613=ORIENTED_EDGE('',*,*,#6760,.T.);
#9614=ORIENTED_EDGE('',*,*,#6838,.T.);
#9615=ORIENTED_EDGE('',*,*,#6839,.T.);
#9616=ORIENTED_EDGE('',*,*,#6840,.F.);
#9617=ORIENTED_EDGE('',*,*,#6841,.T.);
#9618=ORIENTED_EDGE('',*,*,#6842,.F.);
#9619=ORIENTED_EDGE('',*,*,#6841,.F.);
#9620=ORIENTED_EDGE('',*,*,#6843,.T.);
#9621=ORIENTED_EDGE('',*,*,#6842,.T.);
#9622=ORIENTED_EDGE('',*,*,#6844,.F.);
#9623=ORIENTED_EDGE('',*,*,#6840,.T.);
#9624=ORIENTED_EDGE('',*,*,#6843,.F.);
#9625=ORIENTED_EDGE('',*,*,#6845,.T.);
#9626=ORIENTED_EDGE('',*,*,#6846,.T.);
#9627=ORIENTED_EDGE('',*,*,#6845,.F.);
#9628=ORIENTED_EDGE('',*,*,#6838,.F.);
#9629=ORIENTED_EDGE('',*,*,#6847,.T.);
#9630=ORIENTED_EDGE('',*,*,#6844,.T.);
#9631=ORIENTED_EDGE('',*,*,#6847,.F.);
#9632=ORIENTED_EDGE('',*,*,#6846,.F.);
#9633=ORIENTED_EDGE('',*,*,#6848,.F.);
#9634=ORIENTED_EDGE('',*,*,#6848,.T.);
#9635=ORIENTED_EDGE('',*,*,#6849,.T.);
#9636=ORIENTED_EDGE('',*,*,#6839,.F.);
#9637=ORIENTED_EDGE('',*,*,#6849,.F.);
#9638=ORIENTED_EDGE('',*,*,#6850,.T.);
#9639=ORIENTED_EDGE('',*,*,#6851,.T.);
#9640=ORIENTED_EDGE('',*,*,#6852,.F.);
#9641=ORIENTED_EDGE('',*,*,#6851,.F.);
#9642=ORIENTED_EDGE('',*,*,#6853,.T.);
#9643=ORIENTED_EDGE('',*,*,#6854,.T.);
#9644=ORIENTED_EDGE('',*,*,#6855,.F.);
#9645=ORIENTED_EDGE('',*,*,#6856,.F.);
#9646=ORIENTED_EDGE('',*,*,#6857,.T.);
#9647=ORIENTED_EDGE('',*,*,#6856,.T.);
#9648=ORIENTED_EDGE('',*,*,#6858,.F.);
#9649=ORIENTED_EDGE('',*,*,#6859,.F.);
#9650=ORIENTED_EDGE('',*,*,#6860,.T.);
#9651=ORIENTED_EDGE('',*,*,#6859,.T.);
#9652=ORIENTED_EDGE('',*,*,#6861,.F.);
#9653=ORIENTED_EDGE('',*,*,#6862,.F.);
#9654=ORIENTED_EDGE('',*,*,#6863,.T.);
#9655=ORIENTED_EDGE('',*,*,#6862,.T.);
#9656=ORIENTED_EDGE('',*,*,#6864,.F.);
#9657=ORIENTED_EDGE('',*,*,#6854,.F.);
#9658=ORIENTED_EDGE('',*,*,#6865,.T.);
#9659=ORIENTED_EDGE('',*,*,#6866,.T.);
#9660=ORIENTED_EDGE('',*,*,#6867,.F.);
#9661=ORIENTED_EDGE('',*,*,#6868,.F.);
#9662=ORIENTED_EDGE('',*,*,#6869,.T.);
#9663=ORIENTED_EDGE('',*,*,#6868,.T.);
#9664=ORIENTED_EDGE('',*,*,#6870,.F.);
#9665=ORIENTED_EDGE('',*,*,#6871,.F.);
#9666=ORIENTED_EDGE('',*,*,#6872,.T.);
#9667=ORIENTED_EDGE('',*,*,#6871,.T.);
#9668=ORIENTED_EDGE('',*,*,#6873,.F.);
#9669=ORIENTED_EDGE('',*,*,#6874,.F.);
#9670=ORIENTED_EDGE('',*,*,#6875,.T.);
#9671=ORIENTED_EDGE('',*,*,#6874,.T.);
#9672=ORIENTED_EDGE('',*,*,#6876,.F.);
#9673=ORIENTED_EDGE('',*,*,#6866,.F.);
#9674=ORIENTED_EDGE('',*,*,#6877,.T.);
#9675=ORIENTED_EDGE('',*,*,#6878,.T.);
#9676=ORIENTED_EDGE('',*,*,#6879,.F.);
#9677=ORIENTED_EDGE('',*,*,#6878,.F.);
#9678=ORIENTED_EDGE('',*,*,#6880,.T.);
#9679=ORIENTED_EDGE('',*,*,#6881,.T.);
#9680=ORIENTED_EDGE('',*,*,#6882,.F.);
#9681=ORIENTED_EDGE('',*,*,#6881,.F.);
#9682=ORIENTED_EDGE('',*,*,#6883,.T.);
#9683=ORIENTED_EDGE('',*,*,#6884,.T.);
#9684=ORIENTED_EDGE('',*,*,#6885,.F.);
#9685=ORIENTED_EDGE('',*,*,#6886,.F.);
#9686=ORIENTED_EDGE('',*,*,#6887,.T.);
#9687=ORIENTED_EDGE('',*,*,#6886,.T.);
#9688=ORIENTED_EDGE('',*,*,#6888,.F.);
#9689=ORIENTED_EDGE('',*,*,#6889,.F.);
#9690=ORIENTED_EDGE('',*,*,#6890,.T.);
#9691=ORIENTED_EDGE('',*,*,#6889,.T.);
#9692=ORIENTED_EDGE('',*,*,#6891,.F.);
#9693=ORIENTED_EDGE('',*,*,#6892,.F.);
#9694=ORIENTED_EDGE('',*,*,#6893,.T.);
#9695=ORIENTED_EDGE('',*,*,#6892,.T.);
#9696=ORIENTED_EDGE('',*,*,#6894,.F.);
#9697=ORIENTED_EDGE('',*,*,#6884,.F.);
#9698=ORIENTED_EDGE('',*,*,#6895,.T.);
#9699=ORIENTED_EDGE('',*,*,#6896,.T.);
#9700=ORIENTED_EDGE('',*,*,#6897,.F.);
#9701=ORIENTED_EDGE('',*,*,#6896,.F.);
#9702=ORIENTED_EDGE('',*,*,#6898,.T.);
#9703=ORIENTED_EDGE('',*,*,#6899,.T.);
#9704=ORIENTED_EDGE('',*,*,#6900,.F.);
#9705=ORIENTED_EDGE('',*,*,#6899,.F.);
#9706=ORIENTED_EDGE('',*,*,#6901,.F.);
#9707=ORIENTED_EDGE('',*,*,#6902,.T.);
#9708=ORIENTED_EDGE('',*,*,#6903,.F.);
#9709=ORIENTED_EDGE('',*,*,#6904,.F.);
#9710=ORIENTED_EDGE('',*,*,#6905,.F.);
#9711=ORIENTED_EDGE('',*,*,#6904,.T.);
#9712=ORIENTED_EDGE('',*,*,#6906,.F.);
#9713=ORIENTED_EDGE('',*,*,#6907,.F.);
#9714=ORIENTED_EDGE('',*,*,#6908,.F.);
#9715=ORIENTED_EDGE('',*,*,#6907,.T.);
#9716=ORIENTED_EDGE('',*,*,#6909,.F.);
#9717=ORIENTED_EDGE('',*,*,#6910,.F.);
#9718=ORIENTED_EDGE('',*,*,#6911,.F.);
#9719=ORIENTED_EDGE('',*,*,#6910,.T.);
#9720=ORIENTED_EDGE('',*,*,#6912,.F.);
#9721=ORIENTED_EDGE('',*,*,#6913,.F.);
#9722=ORIENTED_EDGE('',*,*,#6914,.F.);
#9723=ORIENTED_EDGE('',*,*,#6913,.T.);
#9724=ORIENTED_EDGE('',*,*,#6915,.F.);
#9725=ORIENTED_EDGE('',*,*,#6916,.F.);
#9726=ORIENTED_EDGE('',*,*,#6917,.F.);
#9727=ORIENTED_EDGE('',*,*,#6916,.T.);
#9728=ORIENTED_EDGE('',*,*,#6918,.F.);
#9729=ORIENTED_EDGE('',*,*,#6919,.F.);
#9730=ORIENTED_EDGE('',*,*,#6920,.F.);
#9731=ORIENTED_EDGE('',*,*,#6919,.T.);
#9732=ORIENTED_EDGE('',*,*,#6921,.F.);
#9733=ORIENTED_EDGE('',*,*,#6922,.F.);
#9734=ORIENTED_EDGE('',*,*,#6923,.F.);
#9735=ORIENTED_EDGE('',*,*,#6922,.T.);
#9736=ORIENTED_EDGE('',*,*,#6924,.F.);
#9737=ORIENTED_EDGE('',*,*,#6925,.F.);
#9738=ORIENTED_EDGE('',*,*,#6926,.F.);
#9739=ORIENTED_EDGE('',*,*,#6925,.T.);
#9740=ORIENTED_EDGE('',*,*,#6927,.F.);
#9741=ORIENTED_EDGE('',*,*,#6928,.F.);
#9742=ORIENTED_EDGE('',*,*,#6929,.T.);
#9743=ORIENTED_EDGE('',*,*,#6928,.T.);
#9744=ORIENTED_EDGE('',*,*,#6930,.F.);
#9745=ORIENTED_EDGE('',*,*,#6931,.F.);
#9746=ORIENTED_EDGE('',*,*,#6932,.F.);
#9747=ORIENTED_EDGE('',*,*,#6931,.T.);
#9748=ORIENTED_EDGE('',*,*,#6933,.F.);
#9749=ORIENTED_EDGE('',*,*,#6934,.F.);
#9750=ORIENTED_EDGE('',*,*,#6935,.T.);
#9751=ORIENTED_EDGE('',*,*,#6934,.T.);
#9752=ORIENTED_EDGE('',*,*,#6936,.F.);
#9753=ORIENTED_EDGE('',*,*,#6937,.F.);
#9754=ORIENTED_EDGE('',*,*,#6938,.F.);
#9755=ORIENTED_EDGE('',*,*,#6937,.T.);
#9756=ORIENTED_EDGE('',*,*,#6939,.F.);
#9757=ORIENTED_EDGE('',*,*,#6940,.F.);
#9758=ORIENTED_EDGE('',*,*,#6941,.T.);
#9759=ORIENTED_EDGE('',*,*,#6940,.T.);
#9760=ORIENTED_EDGE('',*,*,#6942,.F.);
#9761=ORIENTED_EDGE('',*,*,#6943,.F.);
#9762=ORIENTED_EDGE('',*,*,#6944,.F.);
#9763=ORIENTED_EDGE('',*,*,#6943,.T.);
#9764=ORIENTED_EDGE('',*,*,#6945,.F.);
#9765=ORIENTED_EDGE('',*,*,#6946,.F.);
#9766=ORIENTED_EDGE('',*,*,#6947,.T.);
#9767=ORIENTED_EDGE('',*,*,#6946,.T.);
#9768=ORIENTED_EDGE('',*,*,#6948,.F.);
#9769=ORIENTED_EDGE('',*,*,#6902,.F.);
#9770=ORIENTED_EDGE('',*,*,#6948,.T.);
#9771=ORIENTED_EDGE('',*,*,#6945,.T.);
#9772=ORIENTED_EDGE('',*,*,#6942,.T.);
#9773=ORIENTED_EDGE('',*,*,#6939,.T.);
#9774=ORIENTED_EDGE('',*,*,#6936,.T.);
#9775=ORIENTED_EDGE('',*,*,#6933,.T.);
#9776=ORIENTED_EDGE('',*,*,#6930,.T.);
#9777=ORIENTED_EDGE('',*,*,#6927,.T.);
#9778=ORIENTED_EDGE('',*,*,#6924,.T.);
#9779=ORIENTED_EDGE('',*,*,#6921,.T.);
#9780=ORIENTED_EDGE('',*,*,#6918,.T.);
#9781=ORIENTED_EDGE('',*,*,#6915,.T.);
#9782=ORIENTED_EDGE('',*,*,#6912,.T.);
#9783=ORIENTED_EDGE('',*,*,#6909,.T.);
#9784=ORIENTED_EDGE('',*,*,#6906,.T.);
#9785=ORIENTED_EDGE('',*,*,#6903,.T.);
#9786=ORIENTED_EDGE('',*,*,#6900,.T.);
#9787=ORIENTED_EDGE('',*,*,#6897,.T.);
#9788=ORIENTED_EDGE('',*,*,#6894,.T.);
#9789=ORIENTED_EDGE('',*,*,#6891,.T.);
#9790=ORIENTED_EDGE('',*,*,#6888,.T.);
#9791=ORIENTED_EDGE('',*,*,#6885,.T.);
#9792=ORIENTED_EDGE('',*,*,#6882,.T.);
#9793=ORIENTED_EDGE('',*,*,#6879,.T.);
#9794=ORIENTED_EDGE('',*,*,#6876,.T.);
#9795=ORIENTED_EDGE('',*,*,#6873,.T.);
#9796=ORIENTED_EDGE('',*,*,#6870,.T.);
#9797=ORIENTED_EDGE('',*,*,#6867,.T.);
#9798=ORIENTED_EDGE('',*,*,#6864,.T.);
#9799=ORIENTED_EDGE('',*,*,#6861,.T.);
#9800=ORIENTED_EDGE('',*,*,#6858,.T.);
#9801=ORIENTED_EDGE('',*,*,#6855,.T.);
#9802=ORIENTED_EDGE('',*,*,#6852,.T.);
#9803=ORIENTED_EDGE('',*,*,#6947,.F.);
#9804=ORIENTED_EDGE('',*,*,#6901,.T.);
#9805=ORIENTED_EDGE('',*,*,#6905,.T.);
#9806=ORIENTED_EDGE('',*,*,#6908,.T.);
#9807=ORIENTED_EDGE('',*,*,#6911,.T.);
#9808=ORIENTED_EDGE('',*,*,#6914,.T.);
#9809=ORIENTED_EDGE('',*,*,#6917,.T.);
#9810=ORIENTED_EDGE('',*,*,#6920,.T.);
#9811=ORIENTED_EDGE('',*,*,#6923,.T.);
#9812=ORIENTED_EDGE('',*,*,#6926,.T.);
#9813=ORIENTED_EDGE('',*,*,#6929,.F.);
#9814=ORIENTED_EDGE('',*,*,#6932,.T.);
#9815=ORIENTED_EDGE('',*,*,#6935,.F.);
#9816=ORIENTED_EDGE('',*,*,#6938,.T.);
#9817=ORIENTED_EDGE('',*,*,#6941,.F.);
#9818=ORIENTED_EDGE('',*,*,#6944,.T.);
#9819=ORIENTED_EDGE('',*,*,#6898,.F.);
#9820=ORIENTED_EDGE('',*,*,#6895,.F.);
#9821=ORIENTED_EDGE('',*,*,#6893,.F.);
#9822=ORIENTED_EDGE('',*,*,#6883,.F.);
#9823=ORIENTED_EDGE('',*,*,#6887,.F.);
#9824=ORIENTED_EDGE('',*,*,#6890,.F.);
#9825=ORIENTED_EDGE('',*,*,#6880,.F.);
#9826=ORIENTED_EDGE('',*,*,#6877,.F.);
#9827=ORIENTED_EDGE('',*,*,#6875,.F.);
#9828=ORIENTED_EDGE('',*,*,#6865,.F.);
#9829=ORIENTED_EDGE('',*,*,#6869,.F.);
#9830=ORIENTED_EDGE('',*,*,#6872,.F.);
#9831=ORIENTED_EDGE('',*,*,#6863,.F.);
#9832=ORIENTED_EDGE('',*,*,#6853,.F.);
#9833=ORIENTED_EDGE('',*,*,#6857,.F.);
#9834=ORIENTED_EDGE('',*,*,#6860,.F.);
#9835=ORIENTED_EDGE('',*,*,#6850,.F.);
#9836=ORIENTED_EDGE('',*,*,#6949,.F.);
#9837=ORIENTED_EDGE('',*,*,#6950,.T.);
#9838=ORIENTED_EDGE('',*,*,#6951,.F.);
#9839=ORIENTED_EDGE('',*,*,#6950,.F.);
#9840=ORIENTED_EDGE('',*,*,#6952,.F.);
#9841=ORIENTED_EDGE('',*,*,#6953,.F.);
#9842=ORIENTED_EDGE('',*,*,#6954,.F.);
#9843=ORIENTED_EDGE('',*,*,#6955,.T.);
#9844=ORIENTED_EDGE('',*,*,#6956,.F.);
#9845=ORIENTED_EDGE('',*,*,#6957,.F.);
#9846=ORIENTED_EDGE('',*,*,#6958,.F.);
#9847=ORIENTED_EDGE('',*,*,#6955,.F.);
#9848=ORIENTED_EDGE('',*,*,#6959,.F.);
#9849=ORIENTED_EDGE('',*,*,#6960,.T.);
#9850=ORIENTED_EDGE('',*,*,#6956,.T.);
#9851=ORIENTED_EDGE('',*,*,#6958,.T.);
#9852=ORIENTED_EDGE('',*,*,#6961,.T.);
#9853=ORIENTED_EDGE('',*,*,#6962,.F.);
#9854=ORIENTED_EDGE('',*,*,#6961,.F.);
#9855=ORIENTED_EDGE('',*,*,#6957,.T.);
#9856=ORIENTED_EDGE('',*,*,#6960,.F.);
#9857=ORIENTED_EDGE('',*,*,#6949,.T.);
#9858=ORIENTED_EDGE('',*,*,#6959,.T.);
#9859=ORIENTED_EDGE('',*,*,#6963,.T.);
#9860=ORIENTED_EDGE('',*,*,#6964,.F.);
#9861=ORIENTED_EDGE('',*,*,#6965,.T.);
#9862=ORIENTED_EDGE('',*,*,#6966,.F.);
#9863=ORIENTED_EDGE('',*,*,#6967,.T.);
#9864=ORIENTED_EDGE('',*,*,#6964,.T.);
#9865=ORIENTED_EDGE('',*,*,#6967,.F.);
#9866=ORIENTED_EDGE('',*,*,#6966,.T.);
#9867=ORIENTED_EDGE('',*,*,#6962,.T.);
#9868=ORIENTED_EDGE('',*,*,#6965,.F.);
#9869=ORIENTED_EDGE('',*,*,#6968,.T.);
#9870=ORIENTED_EDGE('',*,*,#6969,.F.);
#9871=ORIENTED_EDGE('',*,*,#6968,.F.);
#9872=ORIENTED_EDGE('',*,*,#6970,.T.);
#9873=ORIENTED_EDGE('',*,*,#6971,.T.);
#9874=ORIENTED_EDGE('',*,*,#6952,.T.);
#9875=ORIENTED_EDGE('',*,*,#6954,.T.);
#9876=ORIENTED_EDGE('',*,*,#6972,.T.);
#9877=ORIENTED_EDGE('',*,*,#6963,.F.);
#9878=ORIENTED_EDGE('',*,*,#6972,.F.);
#9879=ORIENTED_EDGE('',*,*,#6953,.T.);
#9880=ORIENTED_EDGE('',*,*,#6971,.F.);
#9881=ORIENTED_EDGE('',*,*,#6951,.T.);
#9882=ORIENTED_EDGE('',*,*,#6973,.F.);
#9883=ORIENTED_EDGE('',*,*,#6974,.T.);
#9884=ORIENTED_EDGE('',*,*,#6975,.T.);
#9885=ORIENTED_EDGE('',*,*,#6974,.F.);
#9886=ORIENTED_EDGE('',*,*,#6973,.T.);
#9887=ORIENTED_EDGE('',*,*,#6969,.T.);
#9888=ORIENTED_EDGE('',*,*,#6975,.F.);
#9889=ORIENTED_EDGE('',*,*,#6970,.F.);
#9890=ORIENTED_EDGE('',*,*,#6976,.T.);
#9891=ORIENTED_EDGE('',*,*,#6977,.T.);
#9892=ORIENTED_EDGE('',*,*,#6978,.T.);
#9893=ORIENTED_EDGE('',*,*,#6979,.T.);
#9894=ORIENTED_EDGE('',*,*,#6980,.T.);
#9895=ORIENTED_EDGE('',*,*,#6981,.T.);
#9896=ORIENTED_EDGE('',*,*,#6982,.T.);
#9897=ORIENTED_EDGE('',*,*,#6983,.T.);
#9898=ORIENTED_EDGE('',*,*,#6984,.F.);
#9899=ORIENTED_EDGE('',*,*,#6985,.F.);
#9900=ORIENTED_EDGE('',*,*,#6986,.F.);
#9901=ORIENTED_EDGE('',*,*,#6981,.F.);
#9902=ORIENTED_EDGE('',*,*,#6986,.T.);
#9903=ORIENTED_EDGE('',*,*,#6987,.F.);
#9904=ORIENTED_EDGE('',*,*,#6988,.F.);
#9905=ORIENTED_EDGE('',*,*,#6982,.F.);
#9906=ORIENTED_EDGE('',*,*,#6988,.T.);
#9907=ORIENTED_EDGE('',*,*,#6989,.F.);
#9908=ORIENTED_EDGE('',*,*,#6990,.F.);
#9909=ORIENTED_EDGE('',*,*,#6983,.F.);
#9910=ORIENTED_EDGE('',*,*,#6990,.T.);
#9911=ORIENTED_EDGE('',*,*,#6991,.F.);
#9912=ORIENTED_EDGE('',*,*,#6984,.T.);
#9913=ORIENTED_EDGE('',*,*,#6980,.F.);
#9914=ORIENTED_EDGE('',*,*,#6992,.F.);
#9915=ORIENTED_EDGE('',*,*,#6993,.F.);
#9916=ORIENTED_EDGE('',*,*,#6994,.F.);
#9917=ORIENTED_EDGE('',*,*,#6977,.F.);
#9918=ORIENTED_EDGE('',*,*,#6994,.T.);
#9919=ORIENTED_EDGE('',*,*,#6995,.F.);
#9920=ORIENTED_EDGE('',*,*,#6996,.F.);
#9921=ORIENTED_EDGE('',*,*,#6978,.F.);
#9922=ORIENTED_EDGE('',*,*,#6996,.T.);
#9923=ORIENTED_EDGE('',*,*,#6997,.F.);
#9924=ORIENTED_EDGE('',*,*,#6998,.F.);
#9925=ORIENTED_EDGE('',*,*,#6979,.F.);
#9926=ORIENTED_EDGE('',*,*,#6998,.T.);
#9927=ORIENTED_EDGE('',*,*,#6999,.F.);
#9928=ORIENTED_EDGE('',*,*,#6992,.T.);
#9929=ORIENTED_EDGE('',*,*,#6976,.F.);
#9930=ORIENTED_EDGE('',*,*,#6999,.T.);
#9931=ORIENTED_EDGE('',*,*,#6997,.T.);
#9932=ORIENTED_EDGE('',*,*,#6995,.T.);
#9933=ORIENTED_EDGE('',*,*,#6993,.T.);
#9934=ORIENTED_EDGE('',*,*,#6991,.T.);
#9935=ORIENTED_EDGE('',*,*,#6989,.T.);
#9936=ORIENTED_EDGE('',*,*,#6987,.T.);
#9937=ORIENTED_EDGE('',*,*,#6985,.T.);
#9938=ORIENTED_EDGE('',*,*,#7000,.T.);
#9939=ORIENTED_EDGE('',*,*,#7001,.T.);
#9940=ORIENTED_EDGE('',*,*,#7002,.F.);
#9941=ORIENTED_EDGE('',*,*,#7001,.F.);
#9942=ORIENTED_EDGE('',*,*,#7003,.T.);
#9943=ORIENTED_EDGE('',*,*,#7004,.T.);
#9944=ORIENTED_EDGE('',*,*,#7005,.F.);
#9945=ORIENTED_EDGE('',*,*,#7006,.F.);
#9946=ORIENTED_EDGE('',*,*,#7007,.T.);
#9947=ORIENTED_EDGE('',*,*,#7006,.T.);
#9948=ORIENTED_EDGE('',*,*,#7008,.F.);
#9949=ORIENTED_EDGE('',*,*,#7009,.F.);
#9950=ORIENTED_EDGE('',*,*,#7010,.T.);
#9951=ORIENTED_EDGE('',*,*,#7009,.T.);
#9952=ORIENTED_EDGE('',*,*,#7011,.F.);
#9953=ORIENTED_EDGE('',*,*,#7012,.F.);
#9954=ORIENTED_EDGE('',*,*,#7013,.T.);
#9955=ORIENTED_EDGE('',*,*,#7012,.T.);
#9956=ORIENTED_EDGE('',*,*,#7014,.F.);
#9957=ORIENTED_EDGE('',*,*,#7004,.F.);
#9958=ORIENTED_EDGE('',*,*,#7015,.T.);
#9959=ORIENTED_EDGE('',*,*,#7016,.T.);
#9960=ORIENTED_EDGE('',*,*,#7017,.F.);
#9961=ORIENTED_EDGE('',*,*,#7016,.F.);
#9962=ORIENTED_EDGE('',*,*,#7018,.T.);
#9963=ORIENTED_EDGE('',*,*,#7019,.T.);
#9964=ORIENTED_EDGE('',*,*,#7020,.F.);
#9965=ORIENTED_EDGE('',*,*,#7019,.F.);
#9966=ORIENTED_EDGE('',*,*,#7021,.T.);
#9967=ORIENTED_EDGE('',*,*,#7022,.T.);
#9968=ORIENTED_EDGE('',*,*,#7023,.F.);
#9969=ORIENTED_EDGE('',*,*,#7022,.F.);
#9970=ORIENTED_EDGE('',*,*,#7024,.T.);
#9971=ORIENTED_EDGE('',*,*,#7025,.T.);
#9972=ORIENTED_EDGE('',*,*,#7026,.F.);
#9973=ORIENTED_EDGE('',*,*,#7025,.F.);
#9974=ORIENTED_EDGE('',*,*,#7027,.T.);
#9975=ORIENTED_EDGE('',*,*,#7028,.T.);
#9976=ORIENTED_EDGE('',*,*,#7029,.F.);
#9977=ORIENTED_EDGE('',*,*,#7028,.F.);
#9978=ORIENTED_EDGE('',*,*,#7030,.T.);
#9979=ORIENTED_EDGE('',*,*,#7031,.T.);
#9980=ORIENTED_EDGE('',*,*,#7032,.F.);
#9981=ORIENTED_EDGE('',*,*,#7033,.F.);
#9982=ORIENTED_EDGE('',*,*,#7034,.T.);
#9983=ORIENTED_EDGE('',*,*,#7033,.T.);
#9984=ORIENTED_EDGE('',*,*,#7035,.F.);
#9985=ORIENTED_EDGE('',*,*,#7036,.F.);
#9986=ORIENTED_EDGE('',*,*,#7037,.T.);
#9987=ORIENTED_EDGE('',*,*,#7036,.T.);
#9988=ORIENTED_EDGE('',*,*,#7038,.F.);
#9989=ORIENTED_EDGE('',*,*,#7039,.F.);
#9990=ORIENTED_EDGE('',*,*,#7040,.T.);
#9991=ORIENTED_EDGE('',*,*,#7039,.T.);
#9992=ORIENTED_EDGE('',*,*,#7041,.F.);
#9993=ORIENTED_EDGE('',*,*,#7031,.F.);
#9994=ORIENTED_EDGE('',*,*,#7042,.T.);
#9995=ORIENTED_EDGE('',*,*,#7043,.T.);
#9996=ORIENTED_EDGE('',*,*,#7044,.F.);
#9997=ORIENTED_EDGE('',*,*,#7045,.F.);
#9998=ORIENTED_EDGE('',*,*,#7046,.T.);
#9999=ORIENTED_EDGE('',*,*,#7045,.T.);
#10000=ORIENTED_EDGE('',*,*,#7047,.F.);
#10001=ORIENTED_EDGE('',*,*,#7048,.F.);
#10002=ORIENTED_EDGE('',*,*,#7049,.T.);
#10003=ORIENTED_EDGE('',*,*,#7048,.T.);
#10004=ORIENTED_EDGE('',*,*,#7050,.F.);
#10005=ORIENTED_EDGE('',*,*,#7051,.F.);
#10006=ORIENTED_EDGE('',*,*,#7052,.T.);
#10007=ORIENTED_EDGE('',*,*,#7051,.T.);
#10008=ORIENTED_EDGE('',*,*,#7053,.F.);
#10009=ORIENTED_EDGE('',*,*,#7043,.F.);
#10010=ORIENTED_EDGE('',*,*,#7054,.T.);
#10011=ORIENTED_EDGE('',*,*,#7055,.T.);
#10012=ORIENTED_EDGE('',*,*,#7056,.F.);
#10013=ORIENTED_EDGE('',*,*,#7055,.F.);
#10014=ORIENTED_EDGE('',*,*,#7057,.T.);
#10015=ORIENTED_EDGE('',*,*,#7058,.T.);
#10016=ORIENTED_EDGE('',*,*,#7059,.F.);
#10017=ORIENTED_EDGE('',*,*,#7058,.F.);
#10018=ORIENTED_EDGE('',*,*,#7060,.T.);
#10019=ORIENTED_EDGE('',*,*,#7061,.T.);
#10020=ORIENTED_EDGE('',*,*,#7062,.F.);
#10021=ORIENTED_EDGE('',*,*,#7061,.F.);
#10022=ORIENTED_EDGE('',*,*,#7063,.T.);
#10023=ORIENTED_EDGE('',*,*,#7064,.T.);
#10024=ORIENTED_EDGE('',*,*,#7065,.F.);
#10025=ORIENTED_EDGE('',*,*,#7064,.F.);
#10026=ORIENTED_EDGE('',*,*,#7066,.T.);
#10027=ORIENTED_EDGE('',*,*,#7067,.T.);
#10028=ORIENTED_EDGE('',*,*,#7068,.F.);
#10029=ORIENTED_EDGE('',*,*,#7067,.F.);
#10030=ORIENTED_EDGE('',*,*,#7069,.T.);
#10031=ORIENTED_EDGE('',*,*,#7070,.T.);
#10032=ORIENTED_EDGE('',*,*,#7071,.F.);
#10033=ORIENTED_EDGE('',*,*,#7072,.F.);
#10034=ORIENTED_EDGE('',*,*,#7073,.T.);
#10035=ORIENTED_EDGE('',*,*,#7072,.T.);
#10036=ORIENTED_EDGE('',*,*,#7074,.F.);
#10037=ORIENTED_EDGE('',*,*,#7075,.F.);
#10038=ORIENTED_EDGE('',*,*,#7076,.T.);
#10039=ORIENTED_EDGE('',*,*,#7075,.T.);
#10040=ORIENTED_EDGE('',*,*,#7077,.F.);
#10041=ORIENTED_EDGE('',*,*,#7078,.F.);
#10042=ORIENTED_EDGE('',*,*,#7079,.T.);
#10043=ORIENTED_EDGE('',*,*,#7078,.T.);
#10044=ORIENTED_EDGE('',*,*,#7080,.F.);
#10045=ORIENTED_EDGE('',*,*,#7070,.F.);
#10046=ORIENTED_EDGE('',*,*,#7081,.T.);
#10047=ORIENTED_EDGE('',*,*,#7082,.T.);
#10048=ORIENTED_EDGE('',*,*,#7083,.F.);
#10049=ORIENTED_EDGE('',*,*,#7082,.F.);
#10050=ORIENTED_EDGE('',*,*,#7084,.T.);
#10051=ORIENTED_EDGE('',*,*,#7085,.T.);
#10052=ORIENTED_EDGE('',*,*,#7086,.F.);
#10053=ORIENTED_EDGE('',*,*,#7085,.F.);
#10054=ORIENTED_EDGE('',*,*,#7087,.T.);
#10055=ORIENTED_EDGE('',*,*,#7088,.T.);
#10056=ORIENTED_EDGE('',*,*,#7089,.F.);
#10057=ORIENTED_EDGE('',*,*,#7090,.F.);
#10058=ORIENTED_EDGE('',*,*,#7091,.T.);
#10059=ORIENTED_EDGE('',*,*,#7090,.T.);
#10060=ORIENTED_EDGE('',*,*,#7092,.F.);
#10061=ORIENTED_EDGE('',*,*,#7093,.F.);
#10062=ORIENTED_EDGE('',*,*,#7094,.T.);
#10063=ORIENTED_EDGE('',*,*,#7093,.T.);
#10064=ORIENTED_EDGE('',*,*,#7095,.F.);
#10065=ORIENTED_EDGE('',*,*,#7096,.F.);
#10066=ORIENTED_EDGE('',*,*,#7097,.T.);
#10067=ORIENTED_EDGE('',*,*,#7096,.T.);
#10068=ORIENTED_EDGE('',*,*,#7098,.F.);
#10069=ORIENTED_EDGE('',*,*,#7088,.F.);
#10070=ORIENTED_EDGE('',*,*,#7099,.T.);
#10071=ORIENTED_EDGE('',*,*,#7100,.T.);
#10072=ORIENTED_EDGE('',*,*,#7101,.F.);
#10073=ORIENTED_EDGE('',*,*,#7102,.F.);
#10074=ORIENTED_EDGE('',*,*,#7103,.T.);
#10075=ORIENTED_EDGE('',*,*,#7102,.T.);
#10076=ORIENTED_EDGE('',*,*,#7104,.F.);
#10077=ORIENTED_EDGE('',*,*,#7105,.F.);
#10078=ORIENTED_EDGE('',*,*,#7106,.T.);
#10079=ORIENTED_EDGE('',*,*,#7105,.T.);
#10080=ORIENTED_EDGE('',*,*,#7107,.F.);
#10081=ORIENTED_EDGE('',*,*,#7108,.F.);
#10082=ORIENTED_EDGE('',*,*,#7109,.T.);
#10083=ORIENTED_EDGE('',*,*,#7108,.T.);
#10084=ORIENTED_EDGE('',*,*,#7110,.F.);
#10085=ORIENTED_EDGE('',*,*,#7100,.F.);
#10086=ORIENTED_EDGE('',*,*,#7111,.T.);
#10087=ORIENTED_EDGE('',*,*,#7112,.T.);
#10088=ORIENTED_EDGE('',*,*,#7113,.F.);
#10089=ORIENTED_EDGE('',*,*,#7114,.F.);
#10090=ORIENTED_EDGE('',*,*,#7115,.T.);
#10091=ORIENTED_EDGE('',*,*,#7114,.T.);
#10092=ORIENTED_EDGE('',*,*,#7116,.F.);
#10093=ORIENTED_EDGE('',*,*,#7117,.F.);
#10094=ORIENTED_EDGE('',*,*,#7118,.T.);
#10095=ORIENTED_EDGE('',*,*,#7117,.T.);
#10096=ORIENTED_EDGE('',*,*,#7119,.F.);
#10097=ORIENTED_EDGE('',*,*,#7120,.F.);
#10098=ORIENTED_EDGE('',*,*,#7121,.T.);
#10099=ORIENTED_EDGE('',*,*,#7120,.T.);
#10100=ORIENTED_EDGE('',*,*,#7122,.F.);
#10101=ORIENTED_EDGE('',*,*,#7112,.F.);
#10102=ORIENTED_EDGE('',*,*,#7123,.T.);
#10103=ORIENTED_EDGE('',*,*,#7124,.T.);
#10104=ORIENTED_EDGE('',*,*,#7125,.F.);
#10105=ORIENTED_EDGE('',*,*,#7126,.F.);
#10106=ORIENTED_EDGE('',*,*,#7127,.T.);
#10107=ORIENTED_EDGE('',*,*,#7126,.T.);
#10108=ORIENTED_EDGE('',*,*,#7128,.F.);
#10109=ORIENTED_EDGE('',*,*,#7129,.F.);
#10110=ORIENTED_EDGE('',*,*,#7130,.T.);
#10111=ORIENTED_EDGE('',*,*,#7129,.T.);
#10112=ORIENTED_EDGE('',*,*,#7131,.F.);
#10113=ORIENTED_EDGE('',*,*,#7132,.F.);
#10114=ORIENTED_EDGE('',*,*,#7133,.T.);
#10115=ORIENTED_EDGE('',*,*,#7132,.T.);
#10116=ORIENTED_EDGE('',*,*,#7134,.F.);
#10117=ORIENTED_EDGE('',*,*,#7124,.F.);
#10118=ORIENTED_EDGE('',*,*,#7135,.T.);
#10119=ORIENTED_EDGE('',*,*,#7136,.T.);
#10120=ORIENTED_EDGE('',*,*,#7137,.F.);
#10121=ORIENTED_EDGE('',*,*,#7136,.F.);
#10122=ORIENTED_EDGE('',*,*,#7138,.T.);
#10123=ORIENTED_EDGE('',*,*,#7139,.T.);
#10124=ORIENTED_EDGE('',*,*,#7140,.F.);
#10125=ORIENTED_EDGE('',*,*,#7139,.F.);
#10126=ORIENTED_EDGE('',*,*,#7141,.F.);
#10127=ORIENTED_EDGE('',*,*,#7142,.T.);
#10128=ORIENTED_EDGE('',*,*,#7143,.F.);
#10129=ORIENTED_EDGE('',*,*,#7144,.F.);
#10130=ORIENTED_EDGE('',*,*,#7145,.T.);
#10131=ORIENTED_EDGE('',*,*,#7144,.T.);
#10132=ORIENTED_EDGE('',*,*,#7146,.F.);
#10133=ORIENTED_EDGE('',*,*,#7147,.F.);
#10134=ORIENTED_EDGE('',*,*,#7148,.F.);
#10135=ORIENTED_EDGE('',*,*,#7147,.T.);
#10136=ORIENTED_EDGE('',*,*,#7149,.F.);
#10137=ORIENTED_EDGE('',*,*,#7150,.F.);
#10138=ORIENTED_EDGE('',*,*,#7151,.T.);
#10139=ORIENTED_EDGE('',*,*,#7150,.T.);
#10140=ORIENTED_EDGE('',*,*,#7152,.F.);
#10141=ORIENTED_EDGE('',*,*,#7153,.F.);
#10142=ORIENTED_EDGE('',*,*,#7154,.F.);
#10143=ORIENTED_EDGE('',*,*,#7153,.T.);
#10144=ORIENTED_EDGE('',*,*,#7155,.F.);
#10145=ORIENTED_EDGE('',*,*,#7156,.F.);
#10146=ORIENTED_EDGE('',*,*,#7157,.T.);
#10147=ORIENTED_EDGE('',*,*,#7156,.T.);
#10148=ORIENTED_EDGE('',*,*,#7158,.F.);
#10149=ORIENTED_EDGE('',*,*,#7159,.F.);
#10150=ORIENTED_EDGE('',*,*,#7160,.F.);
#10151=ORIENTED_EDGE('',*,*,#7159,.T.);
#10152=ORIENTED_EDGE('',*,*,#7161,.F.);
#10153=ORIENTED_EDGE('',*,*,#7162,.F.);
#10154=ORIENTED_EDGE('',*,*,#7163,.T.);
#10155=ORIENTED_EDGE('',*,*,#7162,.T.);
#10156=ORIENTED_EDGE('',*,*,#7164,.F.);
#10157=ORIENTED_EDGE('',*,*,#7142,.F.);
#10158=ORIENTED_EDGE('',*,*,#7164,.T.);
#10159=ORIENTED_EDGE('',*,*,#7161,.T.);
#10160=ORIENTED_EDGE('',*,*,#7158,.T.);
#10161=ORIENTED_EDGE('',*,*,#7155,.T.);
#10162=ORIENTED_EDGE('',*,*,#7152,.T.);
#10163=ORIENTED_EDGE('',*,*,#7149,.T.);
#10164=ORIENTED_EDGE('',*,*,#7146,.T.);
#10165=ORIENTED_EDGE('',*,*,#7143,.T.);
#10166=ORIENTED_EDGE('',*,*,#7140,.T.);
#10167=ORIENTED_EDGE('',*,*,#7137,.T.);
#10168=ORIENTED_EDGE('',*,*,#7134,.T.);
#10169=ORIENTED_EDGE('',*,*,#7131,.T.);
#10170=ORIENTED_EDGE('',*,*,#7128,.T.);
#10171=ORIENTED_EDGE('',*,*,#7125,.T.);
#10172=ORIENTED_EDGE('',*,*,#7122,.T.);
#10173=ORIENTED_EDGE('',*,*,#7119,.T.);
#10174=ORIENTED_EDGE('',*,*,#7116,.T.);
#10175=ORIENTED_EDGE('',*,*,#7113,.T.);
#10176=ORIENTED_EDGE('',*,*,#7110,.T.);
#10177=ORIENTED_EDGE('',*,*,#7107,.T.);
#10178=ORIENTED_EDGE('',*,*,#7104,.T.);
#10179=ORIENTED_EDGE('',*,*,#7101,.T.);
#10180=ORIENTED_EDGE('',*,*,#7098,.T.);
#10181=ORIENTED_EDGE('',*,*,#7095,.T.);
#10182=ORIENTED_EDGE('',*,*,#7092,.T.);
#10183=ORIENTED_EDGE('',*,*,#7089,.T.);
#10184=ORIENTED_EDGE('',*,*,#7086,.T.);
#10185=ORIENTED_EDGE('',*,*,#7083,.T.);
#10186=ORIENTED_EDGE('',*,*,#7080,.T.);
#10187=ORIENTED_EDGE('',*,*,#7077,.T.);
#10188=ORIENTED_EDGE('',*,*,#7074,.T.);
#10189=ORIENTED_EDGE('',*,*,#7071,.T.);
#10190=ORIENTED_EDGE('',*,*,#7068,.T.);
#10191=ORIENTED_EDGE('',*,*,#7065,.T.);
#10192=ORIENTED_EDGE('',*,*,#7062,.T.);
#10193=ORIENTED_EDGE('',*,*,#7059,.T.);
#10194=ORIENTED_EDGE('',*,*,#7056,.T.);
#10195=ORIENTED_EDGE('',*,*,#7053,.T.);
#10196=ORIENTED_EDGE('',*,*,#7050,.T.);
#10197=ORIENTED_EDGE('',*,*,#7047,.T.);
#10198=ORIENTED_EDGE('',*,*,#7044,.T.);
#10199=ORIENTED_EDGE('',*,*,#7041,.T.);
#10200=ORIENTED_EDGE('',*,*,#7038,.T.);
#10201=ORIENTED_EDGE('',*,*,#7035,.T.);
#10202=ORIENTED_EDGE('',*,*,#7032,.T.);
#10203=ORIENTED_EDGE('',*,*,#7029,.T.);
#10204=ORIENTED_EDGE('',*,*,#7026,.T.);
#10205=ORIENTED_EDGE('',*,*,#7023,.T.);
#10206=ORIENTED_EDGE('',*,*,#7020,.T.);
#10207=ORIENTED_EDGE('',*,*,#7017,.T.);
#10208=ORIENTED_EDGE('',*,*,#7014,.T.);
#10209=ORIENTED_EDGE('',*,*,#7011,.T.);
#10210=ORIENTED_EDGE('',*,*,#7008,.T.);
#10211=ORIENTED_EDGE('',*,*,#7005,.T.);
#10212=ORIENTED_EDGE('',*,*,#7002,.T.);
#10213=ORIENTED_EDGE('',*,*,#7163,.F.);
#10214=ORIENTED_EDGE('',*,*,#7141,.T.);
#10215=ORIENTED_EDGE('',*,*,#7145,.F.);
#10216=ORIENTED_EDGE('',*,*,#7148,.T.);
#10217=ORIENTED_EDGE('',*,*,#7151,.F.);
#10218=ORIENTED_EDGE('',*,*,#7154,.T.);
#10219=ORIENTED_EDGE('',*,*,#7157,.F.);
#10220=ORIENTED_EDGE('',*,*,#7160,.T.);
#10221=ORIENTED_EDGE('',*,*,#7138,.F.);
#10222=ORIENTED_EDGE('',*,*,#7135,.F.);
#10223=ORIENTED_EDGE('',*,*,#7133,.F.);
#10224=ORIENTED_EDGE('',*,*,#7123,.F.);
#10225=ORIENTED_EDGE('',*,*,#7127,.F.);
#10226=ORIENTED_EDGE('',*,*,#7130,.F.);
#10227=ORIENTED_EDGE('',*,*,#7121,.F.);
#10228=ORIENTED_EDGE('',*,*,#7111,.F.);
#10229=ORIENTED_EDGE('',*,*,#7115,.F.);
#10230=ORIENTED_EDGE('',*,*,#7118,.F.);
#10231=ORIENTED_EDGE('',*,*,#7109,.F.);
#10232=ORIENTED_EDGE('',*,*,#7099,.F.);
#10233=ORIENTED_EDGE('',*,*,#7103,.F.);
#10234=ORIENTED_EDGE('',*,*,#7106,.F.);
#10235=ORIENTED_EDGE('',*,*,#7097,.F.);
#10236=ORIENTED_EDGE('',*,*,#7087,.F.);
#10237=ORIENTED_EDGE('',*,*,#7091,.F.);
#10238=ORIENTED_EDGE('',*,*,#7094,.F.);
#10239=ORIENTED_EDGE('',*,*,#7084,.F.);
#10240=ORIENTED_EDGE('',*,*,#7081,.F.);
#10241=ORIENTED_EDGE('',*,*,#7079,.F.);
#10242=ORIENTED_EDGE('',*,*,#7069,.F.);
#10243=ORIENTED_EDGE('',*,*,#7073,.F.);
#10244=ORIENTED_EDGE('',*,*,#7076,.F.);
#10245=ORIENTED_EDGE('',*,*,#7066,.F.);
#10246=ORIENTED_EDGE('',*,*,#7063,.F.);
#10247=ORIENTED_EDGE('',*,*,#7060,.F.);
#10248=ORIENTED_EDGE('',*,*,#7057,.F.);
#10249=ORIENTED_EDGE('',*,*,#7054,.F.);
#10250=ORIENTED_EDGE('',*,*,#7052,.F.);
#10251=ORIENTED_EDGE('',*,*,#7042,.F.);
#10252=ORIENTED_EDGE('',*,*,#7046,.F.);
#10253=ORIENTED_EDGE('',*,*,#7049,.F.);
#10254=ORIENTED_EDGE('',*,*,#7040,.F.);
#10255=ORIENTED_EDGE('',*,*,#7030,.F.);
#10256=ORIENTED_EDGE('',*,*,#7034,.F.);
#10257=ORIENTED_EDGE('',*,*,#7037,.F.);
#10258=ORIENTED_EDGE('',*,*,#7027,.F.);
#10259=ORIENTED_EDGE('',*,*,#7024,.F.);
#10260=ORIENTED_EDGE('',*,*,#7021,.F.);
#10261=ORIENTED_EDGE('',*,*,#7018,.F.);
#10262=ORIENTED_EDGE('',*,*,#7015,.F.);
#10263=ORIENTED_EDGE('',*,*,#7013,.F.);
#10264=ORIENTED_EDGE('',*,*,#7003,.F.);
#10265=ORIENTED_EDGE('',*,*,#7007,.F.);
#10266=ORIENTED_EDGE('',*,*,#7010,.F.);
#10267=ORIENTED_EDGE('',*,*,#7000,.F.);
#10268=ORIENTED_EDGE('',*,*,#7165,.F.);
#10269=ORIENTED_EDGE('',*,*,#7166,.T.);
#10270=ORIENTED_EDGE('',*,*,#7167,.F.);
#10271=ORIENTED_EDGE('',*,*,#7166,.F.);
#10272=ORIENTED_EDGE('',*,*,#7168,.F.);
#10273=ORIENTED_EDGE('',*,*,#7169,.T.);
#10274=ORIENTED_EDGE('',*,*,#7170,.F.);
#10275=ORIENTED_EDGE('',*,*,#7169,.F.);
#10276=ORIENTED_EDGE('',*,*,#7171,.F.);
#10277=ORIENTED_EDGE('',*,*,#7172,.T.);
#10278=ORIENTED_EDGE('',*,*,#7173,.F.);
#10279=ORIENTED_EDGE('',*,*,#7172,.F.);
#10280=ORIENTED_EDGE('',*,*,#7174,.F.);
#10281=ORIENTED_EDGE('',*,*,#7175,.T.);
#10282=ORIENTED_EDGE('',*,*,#7176,.F.);
#10283=ORIENTED_EDGE('',*,*,#7175,.F.);
#10284=ORIENTED_EDGE('',*,*,#7177,.F.);
#10285=ORIENTED_EDGE('',*,*,#7178,.T.);
#10286=ORIENTED_EDGE('',*,*,#7179,.F.);
#10287=ORIENTED_EDGE('',*,*,#7178,.F.);
#10288=ORIENTED_EDGE('',*,*,#7180,.F.);
#10289=ORIENTED_EDGE('',*,*,#7181,.T.);
#10290=ORIENTED_EDGE('',*,*,#7182,.F.);
#10291=ORIENTED_EDGE('',*,*,#7183,.F.);
#10292=ORIENTED_EDGE('',*,*,#7184,.T.);
#10293=ORIENTED_EDGE('',*,*,#7183,.T.);
#10294=ORIENTED_EDGE('',*,*,#7185,.F.);
#10295=ORIENTED_EDGE('',*,*,#7186,.F.);
#10296=ORIENTED_EDGE('',*,*,#7187,.F.);
#10297=ORIENTED_EDGE('',*,*,#7186,.T.);
#10298=ORIENTED_EDGE('',*,*,#7188,.F.);
#10299=ORIENTED_EDGE('',*,*,#7189,.F.);
#10300=ORIENTED_EDGE('',*,*,#7190,.T.);
#10301=ORIENTED_EDGE('',*,*,#7189,.T.);
#10302=ORIENTED_EDGE('',*,*,#7191,.F.);
#10303=ORIENTED_EDGE('',*,*,#7192,.F.);
#10304=ORIENTED_EDGE('',*,*,#7193,.F.);
#10305=ORIENTED_EDGE('',*,*,#7192,.T.);
#10306=ORIENTED_EDGE('',*,*,#7194,.F.);
#10307=ORIENTED_EDGE('',*,*,#7195,.F.);
#10308=ORIENTED_EDGE('',*,*,#7196,.T.);
#10309=ORIENTED_EDGE('',*,*,#7195,.T.);
#10310=ORIENTED_EDGE('',*,*,#7197,.F.);
#10311=ORIENTED_EDGE('',*,*,#7198,.F.);
#10312=ORIENTED_EDGE('',*,*,#7199,.F.);
#10313=ORIENTED_EDGE('',*,*,#7198,.T.);
#10314=ORIENTED_EDGE('',*,*,#7200,.F.);
#10315=ORIENTED_EDGE('',*,*,#7201,.F.);
#10316=ORIENTED_EDGE('',*,*,#7202,.T.);
#10317=ORIENTED_EDGE('',*,*,#7201,.T.);
#10318=ORIENTED_EDGE('',*,*,#7203,.F.);
#10319=ORIENTED_EDGE('',*,*,#7181,.F.);
#10320=ORIENTED_EDGE('',*,*,#7202,.F.);
#10321=ORIENTED_EDGE('',*,*,#7180,.T.);
#10322=ORIENTED_EDGE('',*,*,#7184,.F.);
#10323=ORIENTED_EDGE('',*,*,#7187,.T.);
#10324=ORIENTED_EDGE('',*,*,#7190,.F.);
#10325=ORIENTED_EDGE('',*,*,#7193,.T.);
#10326=ORIENTED_EDGE('',*,*,#7196,.F.);
#10327=ORIENTED_EDGE('',*,*,#7199,.T.);
#10328=ORIENTED_EDGE('',*,*,#7177,.T.);
#10329=ORIENTED_EDGE('',*,*,#7174,.T.);
#10330=ORIENTED_EDGE('',*,*,#7171,.T.);
#10331=ORIENTED_EDGE('',*,*,#7168,.T.);
#10332=ORIENTED_EDGE('',*,*,#7165,.T.);
#10333=ORIENTED_EDGE('',*,*,#7203,.T.);
#10334=ORIENTED_EDGE('',*,*,#7200,.T.);
#10335=ORIENTED_EDGE('',*,*,#7197,.T.);
#10336=ORIENTED_EDGE('',*,*,#7194,.T.);
#10337=ORIENTED_EDGE('',*,*,#7191,.T.);
#10338=ORIENTED_EDGE('',*,*,#7188,.T.);
#10339=ORIENTED_EDGE('',*,*,#7185,.T.);
#10340=ORIENTED_EDGE('',*,*,#7182,.T.);
#10341=ORIENTED_EDGE('',*,*,#7179,.T.);
#10342=ORIENTED_EDGE('',*,*,#7176,.T.);
#10343=ORIENTED_EDGE('',*,*,#7173,.T.);
#10344=ORIENTED_EDGE('',*,*,#7170,.T.);
#10345=ORIENTED_EDGE('',*,*,#7167,.T.);
#10346=ORIENTED_EDGE('',*,*,#7204,.F.);
#10347=ORIENTED_EDGE('',*,*,#7205,.T.);
#10348=ORIENTED_EDGE('',*,*,#7206,.F.);
#10349=ORIENTED_EDGE('',*,*,#7205,.F.);
#10350=ORIENTED_EDGE('',*,*,#7207,.T.);
#10351=ORIENTED_EDGE('',*,*,#7208,.T.);
#10352=ORIENTED_EDGE('',*,*,#7209,.T.);
#10353=ORIENTED_EDGE('',*,*,#7208,.F.);
#10354=ORIENTED_EDGE('',*,*,#7210,.T.);
#10355=ORIENTED_EDGE('',*,*,#7209,.F.);
#10356=ORIENTED_EDGE('',*,*,#7204,.T.);
#10357=ORIENTED_EDGE('',*,*,#7211,.T.);
#10358=ORIENTED_EDGE('',*,*,#7207,.F.);
#10359=ORIENTED_EDGE('',*,*,#7211,.F.);
#10360=ORIENTED_EDGE('',*,*,#7212,.F.);
#10361=ORIENTED_EDGE('',*,*,#7213,.F.);
#10362=ORIENTED_EDGE('',*,*,#7214,.T.);
#10363=ORIENTED_EDGE('',*,*,#7214,.F.);
#10364=ORIENTED_EDGE('',*,*,#7215,.F.);
#10365=ORIENTED_EDGE('',*,*,#7216,.T.);
#10366=ORIENTED_EDGE('',*,*,#7216,.F.);
#10367=ORIENTED_EDGE('',*,*,#7217,.F.);
#10368=ORIENTED_EDGE('',*,*,#7218,.T.);
#10369=ORIENTED_EDGE('',*,*,#7218,.F.);
#10370=ORIENTED_EDGE('',*,*,#7219,.F.);
#10371=ORIENTED_EDGE('',*,*,#7220,.T.);
#10372=ORIENTED_EDGE('',*,*,#7220,.F.);
#10373=ORIENTED_EDGE('',*,*,#7221,.F.);
#10374=ORIENTED_EDGE('',*,*,#7222,.T.);
#10375=ORIENTED_EDGE('',*,*,#7222,.F.);
#10376=ORIENTED_EDGE('',*,*,#7223,.F.);
#10377=ORIENTED_EDGE('',*,*,#7212,.T.);
#10378=ORIENTED_EDGE('',*,*,#7224,.F.);
#10379=ORIENTED_EDGE('',*,*,#7225,.T.);
#10380=ORIENTED_EDGE('',*,*,#7213,.T.);
#10381=ORIENTED_EDGE('',*,*,#7226,.F.);
#10382=ORIENTED_EDGE('',*,*,#7227,.F.);
#10383=ORIENTED_EDGE('',*,*,#7228,.T.);
#10384=ORIENTED_EDGE('',*,*,#7215,.T.);
#10385=ORIENTED_EDGE('',*,*,#7225,.F.);
#10386=ORIENTED_EDGE('',*,*,#7229,.F.);
#10387=ORIENTED_EDGE('',*,*,#7230,.T.);
#10388=ORIENTED_EDGE('',*,*,#7217,.T.);
#10389=ORIENTED_EDGE('',*,*,#7228,.F.);
#10390=ORIENTED_EDGE('',*,*,#7231,.F.);
#10391=ORIENTED_EDGE('',*,*,#7232,.T.);
#10392=ORIENTED_EDGE('',*,*,#7219,.T.);
#10393=ORIENTED_EDGE('',*,*,#7230,.F.);
#10394=ORIENTED_EDGE('',*,*,#7233,.F.);
#10395=ORIENTED_EDGE('',*,*,#7234,.T.);
#10396=ORIENTED_EDGE('',*,*,#7221,.T.);
#10397=ORIENTED_EDGE('',*,*,#7232,.F.);
#10398=ORIENTED_EDGE('',*,*,#7235,.F.);
#10399=ORIENTED_EDGE('',*,*,#7226,.T.);
#10400=ORIENTED_EDGE('',*,*,#7223,.T.);
#10401=ORIENTED_EDGE('',*,*,#7234,.F.);
#10402=ORIENTED_EDGE('',*,*,#7206,.T.);
#10403=ORIENTED_EDGE('',*,*,#7236,.F.);
#10404=ORIENTED_EDGE('',*,*,#7224,.T.);
#10405=ORIENTED_EDGE('',*,*,#7235,.T.);
#10406=ORIENTED_EDGE('',*,*,#7233,.T.);
#10407=ORIENTED_EDGE('',*,*,#7231,.T.);
#10408=ORIENTED_EDGE('',*,*,#7229,.T.);
#10409=ORIENTED_EDGE('',*,*,#7227,.T.);
#10410=ORIENTED_EDGE('',*,*,#7236,.T.);
#10411=ORIENTED_EDGE('',*,*,#7237,.T.);
#10412=ORIENTED_EDGE('',*,*,#7210,.F.);
#10413=ORIENTED_EDGE('',*,*,#7237,.F.);
#10414=CYLINDRICAL_SURFACE('',#11440,3.175);
#10415=CYLINDRICAL_SURFACE('',#11476,3.175);
#10416=CYLINDRICAL_SURFACE('',#11512,3.175);
#10417=CYLINDRICAL_SURFACE('',#11548,3.175);
#10418=CYLINDRICAL_SURFACE('',#11584,1.905);
#10419=CYLINDRICAL_SURFACE('',#11586,1.905);
#10420=CYLINDRICAL_SURFACE('',#11587,1.905);
#10421=CYLINDRICAL_SURFACE('',#11588,1.905);
#10422=CYLINDRICAL_SURFACE('',#11589,1.905);
#10423=CYLINDRICAL_SURFACE('',#11590,1.905);
#10424=CYLINDRICAL_SURFACE('',#11591,1.905);
#10425=CYLINDRICAL_SURFACE('',#11592,1.905);
#10426=CYLINDRICAL_SURFACE('',#11593,1.905);
#10427=CYLINDRICAL_SURFACE('',#11594,1.905);
#10428=CYLINDRICAL_SURFACE('',#11595,1.905);
#10429=CYLINDRICAL_SURFACE('',#11596,1.905);
#10430=CYLINDRICAL_SURFACE('',#11597,1.905);
#10431=CYLINDRICAL_SURFACE('',#11598,1.905);
#10432=CYLINDRICAL_SURFACE('',#11599,1.905);
#10433=CYLINDRICAL_SURFACE('',#11600,1.905);
#10434=CYLINDRICAL_SURFACE('',#11601,1.905);
#10435=CYLINDRICAL_SURFACE('',#11602,1.905);
#10436=CYLINDRICAL_SURFACE('',#11603,1.905);
#10437=CYLINDRICAL_SURFACE('',#11604,1.905);
#10438=CYLINDRICAL_SURFACE('',#11606,1.905);
#10439=CYLINDRICAL_SURFACE('',#11607,1.905);
#10440=CYLINDRICAL_SURFACE('',#11608,1.905);
#10441=CYLINDRICAL_SURFACE('',#11609,1.905);
#10442=CYLINDRICAL_SURFACE('',#11610,1.905);
#10443=CYLINDRICAL_SURFACE('',#11611,1.905);
#10444=CYLINDRICAL_SURFACE('',#11612,1.905);
#10445=CYLINDRICAL_SURFACE('',#11613,1.905);
#10446=CYLINDRICAL_SURFACE('',#11614,1.905);
#10447=CYLINDRICAL_SURFACE('',#11615,1.905);
#10448=CYLINDRICAL_SURFACE('',#11616,1.905);
#10449=CYLINDRICAL_SURFACE('',#11617,1.905);
#10450=CYLINDRICAL_SURFACE('',#11618,1.905);
#10451=CYLINDRICAL_SURFACE('',#11619,1.905);
#10452=CYLINDRICAL_SURFACE('',#11620,1.905);
#10453=CYLINDRICAL_SURFACE('',#11621,1.905);
#10454=CYLINDRICAL_SURFACE('',#11622,1.905);
#10455=CYLINDRICAL_SURFACE('',#11623,1.905);
#10456=CYLINDRICAL_SURFACE('',#11624,1.905);
#10457=CYLINDRICAL_SURFACE('',#11626,1.905);
#10458=CYLINDRICAL_SURFACE('',#11627,1.905);
#10459=CYLINDRICAL_SURFACE('',#11628,1.905);
#10460=CYLINDRICAL_SURFACE('',#11629,1.905);
#10461=CYLINDRICAL_SURFACE('',#11630,1.905);
#10462=CYLINDRICAL_SURFACE('',#11631,1.905);
#10463=CYLINDRICAL_SURFACE('',#11632,1.905);
#10464=CYLINDRICAL_SURFACE('',#11633,1.905);
#10465=CYLINDRICAL_SURFACE('',#11634,1.905);
#10466=CYLINDRICAL_SURFACE('',#11635,1.905);
#10467=CYLINDRICAL_SURFACE('',#11636,1.905);
#10468=CYLINDRICAL_SURFACE('',#11637,1.905);
#10469=CYLINDRICAL_SURFACE('',#11638,1.905);
#10470=CYLINDRICAL_SURFACE('',#11639,1.905);
#10471=CYLINDRICAL_SURFACE('',#11640,1.905);
#10472=CYLINDRICAL_SURFACE('',#11641,1.905);
#10473=CYLINDRICAL_SURFACE('',#11642,1.905);
#10474=CYLINDRICAL_SURFACE('',#11643,1.905);
#10475=CYLINDRICAL_SURFACE('',#11644,1.905);
#10476=CYLINDRICAL_SURFACE('',#11646,1.905);
#10477=CYLINDRICAL_SURFACE('',#11647,1.905);
#10478=CYLINDRICAL_SURFACE('',#11648,1.905);
#10479=CYLINDRICAL_SURFACE('',#11649,1.905);
#10480=CYLINDRICAL_SURFACE('',#11650,1.905);
#10481=CYLINDRICAL_SURFACE('',#11651,1.905);
#10482=CYLINDRICAL_SURFACE('',#11652,1.905);
#10483=CYLINDRICAL_SURFACE('',#11653,1.905);
#10484=CYLINDRICAL_SURFACE('',#11654,1.905);
#10485=CYLINDRICAL_SURFACE('',#11655,1.905);
#10486=CYLINDRICAL_SURFACE('',#11656,1.905);
#10487=CYLINDRICAL_SURFACE('',#11657,1.905);
#10488=CYLINDRICAL_SURFACE('',#11658,1.905);
#10489=CYLINDRICAL_SURFACE('',#11659,1.905);
#10490=CYLINDRICAL_SURFACE('',#11660,1.905);
#10491=CYLINDRICAL_SURFACE('',#11661,1.905);
#10492=CYLINDRICAL_SURFACE('',#11662,1.905);
#10493=CYLINDRICAL_SURFACE('',#11663,1.93206329386826);
#10494=CYLINDRICAL_SURFACE('',#11665,1.93206329386826);
#10495=CYLINDRICAL_SURFACE('',#11667,1.93206329386826);
#10496=CYLINDRICAL_SURFACE('',#11668,1.93206329386826);
#10497=CYLINDRICAL_SURFACE('',#11669,1.93206329386826);
#10498=CYLINDRICAL_SURFACE('',#11670,1.93206329386826);
#10499=CYLINDRICAL_SURFACE('',#11671,1.93206329386826);
#10500=CYLINDRICAL_SURFACE('',#11672,1.93206329386825);
#10501=CYLINDRICAL_SURFACE('',#11674,1.93206329386825);
#10502=CYLINDRICAL_SURFACE('',#11676,1.93206329386825);
#10503=CYLINDRICAL_SURFACE('',#11677,1.93206329386825);
#10504=CYLINDRICAL_SURFACE('',#11678,1.93206329386825);
#10505=CYLINDRICAL_SURFACE('',#11679,1.93206329386825);
#10506=CYLINDRICAL_SURFACE('',#11680,1.93206329386825);
#10507=CYLINDRICAL_SURFACE('',#11681,1.93206329386826);
#10508=CYLINDRICAL_SURFACE('',#11683,1.93206329386826);
#10509=CYLINDRICAL_SURFACE('',#11685,1.93206329386826);
#10510=CYLINDRICAL_SURFACE('',#11686,1.93206329386826);
#10511=CYLINDRICAL_SURFACE('',#11687,1.93206329386826);
#10512=CYLINDRICAL_SURFACE('',#11688,1.93206329386826);
#10513=CYLINDRICAL_SURFACE('',#11689,1.93206329386826);
#10514=CYLINDRICAL_SURFACE('',#11690,1.93206329386822);
#10515=CYLINDRICAL_SURFACE('',#11692,1.93206329386822);
#10516=CYLINDRICAL_SURFACE('',#11694,1.93206329386822);
#10517=CYLINDRICAL_SURFACE('',#11695,1.93206329386822);
#10518=CYLINDRICAL_SURFACE('',#11696,1.93206329386822);
#10519=CYLINDRICAL_SURFACE('',#11697,1.93206329386822);
#10520=CYLINDRICAL_SURFACE('',#11698,1.93206329386822);
#10521=CYLINDRICAL_SURFACE('',#11699,1.93206329386822);
#10522=CYLINDRICAL_SURFACE('',#11700,1.93206329386826);
#10523=CYLINDRICAL_SURFACE('',#11701,1.93206329386825);
#10524=CYLINDRICAL_SURFACE('',#11702,1.93206329386826);
#10525=CYLINDRICAL_SURFACE('',#11703,1.905);
#10526=CYLINDRICAL_SURFACE('',#11705,1.905);
#10527=CYLINDRICAL_SURFACE('',#11707,1.905);
#10528=CYLINDRICAL_SURFACE('',#11709,1.905);
#10529=CYLINDRICAL_SURFACE('',#11711,2.62699999999999);
#10530=CYLINDRICAL_SURFACE('',#11714,3.76999999999999);
#10531=CYLINDRICAL_SURFACE('',#11720,10.985);
#10532=CYLINDRICAL_SURFACE('',#11751,0.762);
#10533=CYLINDRICAL_SURFACE('',#11756,0.761999999999999);
#10534=CYLINDRICAL_SURFACE('',#11759,0.762);
#10535=CYLINDRICAL_SURFACE('',#11762,0.761999999999999);
#10536=CYLINDRICAL_SURFACE('',#11765,0.762);
#10537=CYLINDRICAL_SURFACE('',#11768,0.762000000000001);
#10538=CYLINDRICAL_SURFACE('',#11770,0.762);
#10539=CYLINDRICAL_SURFACE('',#11772,0.762000000000001);
#10540=CYLINDRICAL_SURFACE('',#11782,2.5);
#10541=CYLINDRICAL_SURFACE('',#11789,5.16699999999999);
#10542=CYLINDRICAL_SURFACE('',#11804,3.175);
#10543=CYLINDRICAL_SURFACE('',#11806,3.175);
#10544=CYLINDRICAL_SURFACE('',#11808,3.175);
#10545=CYLINDRICAL_SURFACE('',#11810,3.175);
#10546=CYLINDRICAL_SURFACE('',#11812,2.62699999999999);
#10547=CYLINDRICAL_SURFACE('',#11827,0.762);
#10548=CYLINDRICAL_SURFACE('',#11830,0.761999999999999);
#10549=CYLINDRICAL_SURFACE('',#11832,0.762);
#10550=CYLINDRICAL_SURFACE('',#11835,0.761999999999999);
#10551=CYLINDRICAL_SURFACE('',#11838,0.762);
#10552=CYLINDRICAL_SURFACE('',#11841,0.761999999999999);
#10553=CYLINDRICAL_SURFACE('',#11844,0.762);
#10554=CYLINDRICAL_SURFACE('',#11853,0.761999999999999);
#10555=CYLINDRICAL_SURFACE('',#11858,2.62699999999999);
#10556=CYLINDRICAL_SURFACE('',#11861,1.905);
#10557=CYLINDRICAL_SURFACE('',#11864,1.905);
#10558=CYLINDRICAL_SURFACE('',#11867,1.905);
#10559=CYLINDRICAL_SURFACE('',#11870,1.905);
#10560=CYLINDRICAL_SURFACE('',#11892,11.9505);
#10561=CYLINDRICAL_SURFACE('',#11900,8.00000000000001);
#10562=CYLINDRICAL_SURFACE('',#11902,2.5);
#10563=CYLINDRICAL_SURFACE('',#11905,4.49999999999999);
#10564=CYLINDRICAL_SURFACE('',#11929,2.117);
#10565=CYLINDRICAL_SURFACE('',#11931,5.73351648351648);
#10566=CYLINDRICAL_SURFACE('',#11937,5.73351648351648);
#10567=CYLINDRICAL_SURFACE('',#11942,8.);
#10568=CYLINDRICAL_SURFACE('',#11949,4.76648351648352);
#10569=CYLINDRICAL_SURFACE('',#11955,3.26912128048043);
#10570=CYLINDRICAL_SURFACE('',#11965,2.5);
#10571=CYLINDRICAL_SURFACE('',#11970,4.76648351648352);
#10572=CYLINDRICAL_SURFACE('',#11976,3.26912128048043);
#10573=CYLINDRICAL_SURFACE('',#12015,2.1);
#10574=CYLINDRICAL_SURFACE('',#12027,0.500000000000003);
#10575=CYLINDRICAL_SURFACE('',#12048,0.500000000000003);
#10576=CYLINDRICAL_SURFACE('',#12072,2.1);
#10577=CYLINDRICAL_SURFACE('',#12083,0.500000000000003);
#10578=CYLINDRICAL_SURFACE('',#12104,0.500000000000003);
#10579=CYLINDRICAL_SURFACE('',#12122,9.15);
#10580=CYLINDRICAL_SURFACE('',#12129,10.75);
#10581=CYLINDRICAL_SURFACE('',#12131,10.75);
#10582=CYLINDRICAL_SURFACE('',#12134,3.17500000000003);
#10583=CYLINDRICAL_SURFACE('',#12136,2.155);
#10584=CYLINDRICAL_SURFACE('',#12147,2.155);
#10585=CYLINDRICAL_SURFACE('',#12150,2.155);
#10586=CYLINDRICAL_SURFACE('',#12157,11.493);
#10587=CYLINDRICAL_SURFACE('',#12160,2.155);
#10588=CYLINDRICAL_SURFACE('',#12172,5.);
#10589=CYLINDRICAL_SURFACE('',#12176,5.00000000000002);
#10590=CYLINDRICAL_SURFACE('',#12180,5.);
#10591=CYLINDRICAL_SURFACE('',#12184,4.99999999999999);
#10592=CYLINDRICAL_SURFACE('',#12190,1.5);
#10593=CYLINDRICAL_SURFACE('',#12191,1.5);
#10594=CYLINDRICAL_SURFACE('',#12192,6.00000000000002);
#10595=CYLINDRICAL_SURFACE('',#12200,10.75);
#10596=CYLINDRICAL_SURFACE('',#12203,9.15);
#10597=CYLINDRICAL_SURFACE('',#12205,3.17500000000003);
#10598=CYLINDRICAL_SURFACE('',#12207,10.75);
#10599=CYLINDRICAL_SURFACE('',#12219,9.5);
#10600=CYLINDRICAL_SURFACE('',#12222,9.5);
#10601=CYLINDRICAL_SURFACE('',#12225,11.5);
#10602=CYLINDRICAL_SURFACE('',#12228,11.5);
#10603=CYLINDRICAL_SURFACE('',#12232,2.5);
#10604=CYLINDRICAL_SURFACE('',#12236,1.3925055570925);
#10605=CYLINDRICAL_SURFACE('',#12240,1.3925055570925);
#10606=CYLINDRICAL_SURFACE('',#12243,2.46675107308807);
#10607=CYLINDRICAL_SURFACE('',#12246,2.46675107308807);
#10608=CYLINDRICAL_SURFACE('',#12249,2.46675107308807);
#10609=CYLINDRICAL_SURFACE('',#12252,2.46675107308807);
#10610=CYLINDRICAL_SURFACE('',#12255,2.46675107308807);
#10611=CYLINDRICAL_SURFACE('',#12259,2.69990459756453);
#10612=CYLINDRICAL_SURFACE('',#12263,2.69990459756453);
#10613=CYLINDRICAL_SURFACE('',#12267,1.3925055570925);
#10614=CYLINDRICAL_SURFACE('',#12271,1.3925055570925);
#10615=CYLINDRICAL_SURFACE('',#12274,2.5);
#10616=CYLINDRICAL_SURFACE('',#12277,2.46675107308807);
#10617=CYLINDRICAL_SURFACE('',#12280,2.5);
#10618=CYLINDRICAL_SURFACE('',#12283,2.46675107308807);
#10619=CYLINDRICAL_SURFACE('',#12286,2.46675107308807);
#10620=CYLINDRICAL_SURFACE('',#12290,1.3925055570925);
#10621=CYLINDRICAL_SURFACE('',#12294,1.3925055570925);
#10622=CYLINDRICAL_SURFACE('',#12297,2.5);
#10623=CYLINDRICAL_SURFACE('',#12300,2.46675107308807);
#10624=CYLINDRICAL_SURFACE('',#12304,1.3925055570925);
#10625=CYLINDRICAL_SURFACE('',#12308,1.3925055570925);
#10626=CYLINDRICAL_SURFACE('',#12312,1.3925055570925);
#10627=CYLINDRICAL_SURFACE('',#12316,1.3925055570925);
#10628=CYLINDRICAL_SURFACE('',#12320,1.3925055570925);
#10629=CYLINDRICAL_SURFACE('',#12324,1.3925055570925);
#10630=CYLINDRICAL_SURFACE('',#12328,2.69990459756453);
#10631=CYLINDRICAL_SURFACE('',#12332,2.69990459756453);
#10632=CYLINDRICAL_SURFACE('',#12335,2.46675107308807);
#10633=CYLINDRICAL_SURFACE('',#12338,2.46675107308807);
#10634=CYLINDRICAL_SURFACE('',#12342,3.00000000000004);
#10635=CYLINDRICAL_SURFACE('',#12346,3.00000000000003);
#10636=CYLINDRICAL_SURFACE('',#12350,3.00000000000004);
#10637=CYLINDRICAL_SURFACE('',#12354,3.00000000000004);
#10638=CYLINDRICAL_SURFACE('',#12360,2.50000000000001);
#10639=CYLINDRICAL_SURFACE('',#12363,2.50000000000001);
#10640=CYLINDRICAL_SURFACE('',#12366,3.17500000000003);
#10641=CYLINDRICAL_SURFACE('',#12369,2.50000000000001);
#10642=CYLINDRICAL_SURFACE('',#12372,2.50000000000001);
#10643=CYLINDRICAL_SURFACE('',#12375,4.99999999999993);
#10644=CYLINDRICAL_SURFACE('',#12379,4.99999999999993);
#10645=CYLINDRICAL_SURFACE('',#12383,5.);
#10646=CYLINDRICAL_SURFACE('',#12387,5.);
#10647=CYLINDRICAL_SURFACE('',#12403,2.4505);
#10648=ADVANCED_FACE('',(#1027),#10414,.T.);
#10649=ADVANCED_FACE('',(#1028),#1019,.T.);
#10650=ADVANCED_FACE('',(#1029),#390,.T.);
#10651=ADVANCED_FACE('',(#1030),#391,.T.);
#10652=ADVANCED_FACE('',(#1031),#392,.T.);
#10653=ADVANCED_FACE('',(#1032),#393,.F.);
#10654=ADVANCED_FACE('',(#1033),#394,.T.);
#10655=ADVANCED_FACE('',(#1034),#395,.F.);
#10656=ADVANCED_FACE('',(#1035),#396,.T.);
#10657=ADVANCED_FACE('',(#1036),#397,.F.);
#10658=ADVANCED_FACE('',(#1037),#398,.T.);
#10659=ADVANCED_FACE('',(#1038),#399,.T.);
#10660=ADVANCED_FACE('',(#1039),#400,.T.);
#10661=ADVANCED_FACE('',(#1040),#401,.T.);
#10662=ADVANCED_FACE('',(#1041),#402,.T.);
#10663=ADVANCED_FACE('',(#1042),#403,.T.);
#10664=ADVANCED_FACE('',(#1043),#404,.F.);
#10665=ADVANCED_FACE('',(#1044),#405,.F.);
#10666=ADVANCED_FACE('',(#1045),#406,.T.);
#10667=ADVANCED_FACE('',(#1046),#407,.T.);
#10668=ADVANCED_FACE('',(#1047),#10415,.T.);
#10669=ADVANCED_FACE('',(#1048),#1020,.T.);
#10670=ADVANCED_FACE('',(#1049),#408,.T.);
#10671=ADVANCED_FACE('',(#1050),#409,.T.);
#10672=ADVANCED_FACE('',(#1051),#410,.T.);
#10673=ADVANCED_FACE('',(#1052),#411,.F.);
#10674=ADVANCED_FACE('',(#1053),#412,.T.);
#10675=ADVANCED_FACE('',(#1054),#413,.F.);
#10676=ADVANCED_FACE('',(#1055),#414,.T.);
#10677=ADVANCED_FACE('',(#1056),#415,.F.);
#10678=ADVANCED_FACE('',(#1057),#416,.T.);
#10679=ADVANCED_FACE('',(#1058),#417,.T.);
#10680=ADVANCED_FACE('',(#1059),#418,.T.);
#10681=ADVANCED_FACE('',(#1060),#419,.T.);
#10682=ADVANCED_FACE('',(#1061),#420,.T.);
#10683=ADVANCED_FACE('',(#1062),#421,.T.);
#10684=ADVANCED_FACE('',(#1063),#422,.F.);
#10685=ADVANCED_FACE('',(#1064),#423,.F.);
#10686=ADVANCED_FACE('',(#1065),#424,.T.);
#10687=ADVANCED_FACE('',(#1066),#425,.T.);
#10688=ADVANCED_FACE('',(#1067),#10416,.T.);
#10689=ADVANCED_FACE('',(#1068),#1021,.T.);
#10690=ADVANCED_FACE('',(#1069),#426,.T.);
#10691=ADVANCED_FACE('',(#1070),#427,.T.);
#10692=ADVANCED_FACE('',(#1071),#428,.T.);
#10693=ADVANCED_FACE('',(#1072),#429,.F.);
#10694=ADVANCED_FACE('',(#1073),#430,.T.);
#10695=ADVANCED_FACE('',(#1074),#431,.F.);
#10696=ADVANCED_FACE('',(#1075),#432,.T.);
#10697=ADVANCED_FACE('',(#1076),#433,.F.);
#10698=ADVANCED_FACE('',(#1077),#434,.T.);
#10699=ADVANCED_FACE('',(#1078),#435,.T.);
#10700=ADVANCED_FACE('',(#1079),#436,.T.);
#10701=ADVANCED_FACE('',(#1080),#437,.T.);
#10702=ADVANCED_FACE('',(#1081),#438,.T.);
#10703=ADVANCED_FACE('',(#1082),#439,.T.);
#10704=ADVANCED_FACE('',(#1083),#440,.F.);
#10705=ADVANCED_FACE('',(#1084),#441,.F.);
#10706=ADVANCED_FACE('',(#1085),#442,.T.);
#10707=ADVANCED_FACE('',(#1086),#443,.T.);
#10708=ADVANCED_FACE('',(#1087),#10417,.T.);
#10709=ADVANCED_FACE('',(#1088),#1022,.T.);
#10710=ADVANCED_FACE('',(#1089),#444,.T.);
#10711=ADVANCED_FACE('',(#1090),#445,.T.);
#10712=ADVANCED_FACE('',(#1091),#446,.T.);
#10713=ADVANCED_FACE('',(#1092),#447,.F.);
#10714=ADVANCED_FACE('',(#1093),#448,.T.);
#10715=ADVANCED_FACE('',(#1094),#449,.F.);
#10716=ADVANCED_FACE('',(#1095),#450,.T.);
#10717=ADVANCED_FACE('',(#1096),#451,.F.);
#10718=ADVANCED_FACE('',(#1097),#452,.T.);
#10719=ADVANCED_FACE('',(#1098),#453,.T.);
#10720=ADVANCED_FACE('',(#1099),#454,.T.);
#10721=ADVANCED_FACE('',(#1100),#455,.T.);
#10722=ADVANCED_FACE('',(#1101),#456,.T.);
#10723=ADVANCED_FACE('',(#1102),#457,.T.);
#10724=ADVANCED_FACE('',(#1103),#458,.F.);
#10725=ADVANCED_FACE('',(#1104),#459,.F.);
#10726=ADVANCED_FACE('',(#1105),#460,.T.);
#10727=ADVANCED_FACE('',(#1106),#461,.T.);
#10728=ADVANCED_FACE('',(#1107),#10418,.F.);
#10729=ADVANCED_FACE('',(#1108),#10419,.F.);
#10730=ADVANCED_FACE('',(#1109),#10420,.F.);
#10731=ADVANCED_FACE('',(#1110),#10421,.F.);
#10732=ADVANCED_FACE('',(#1111),#10422,.F.);
#10733=ADVANCED_FACE('',(#1112),#10423,.F.);
#10734=ADVANCED_FACE('',(#1113),#10424,.F.);
#10735=ADVANCED_FACE('',(#1114),#10425,.F.);
#10736=ADVANCED_FACE('',(#1115),#10426,.F.);
#10737=ADVANCED_FACE('',(#1116),#10427,.F.);
#10738=ADVANCED_FACE('',(#1117),#10428,.F.);
#10739=ADVANCED_FACE('',(#1118),#10429,.F.);
#10740=ADVANCED_FACE('',(#1119),#10430,.F.);
#10741=ADVANCED_FACE('',(#1120),#10431,.F.);
#10742=ADVANCED_FACE('',(#1121),#10432,.F.);
#10743=ADVANCED_FACE('',(#1122),#10433,.F.);
#10744=ADVANCED_FACE('',(#1123),#10434,.F.);
#10745=ADVANCED_FACE('',(#1124),#10435,.F.);
#10746=ADVANCED_FACE('',(#1125),#10436,.F.);
#10747=ADVANCED_FACE('',(#1126),#10437,.F.);
#10748=ADVANCED_FACE('',(#1127),#10438,.F.);
#10749=ADVANCED_FACE('',(#1128),#10439,.F.);
#10750=ADVANCED_FACE('',(#1129),#10440,.F.);
#10751=ADVANCED_FACE('',(#1130),#10441,.F.);
#10752=ADVANCED_FACE('',(#1131),#10442,.F.);
#10753=ADVANCED_FACE('',(#1132),#10443,.F.);
#10754=ADVANCED_FACE('',(#1133),#10444,.F.);
#10755=ADVANCED_FACE('',(#1134),#10445,.F.);
#10756=ADVANCED_FACE('',(#1135),#10446,.F.);
#10757=ADVANCED_FACE('',(#1136),#10447,.F.);
#10758=ADVANCED_FACE('',(#1137),#10448,.F.);
#10759=ADVANCED_FACE('',(#1138),#10449,.F.);
#10760=ADVANCED_FACE('',(#1139),#10450,.F.);
#10761=ADVANCED_FACE('',(#1140),#10451,.F.);
#10762=ADVANCED_FACE('',(#1141),#10452,.F.);
#10763=ADVANCED_FACE('',(#1142),#10453,.F.);
#10764=ADVANCED_FACE('',(#1143),#10454,.F.);
#10765=ADVANCED_FACE('',(#1144),#10455,.F.);
#10766=ADVANCED_FACE('',(#1145),#10456,.F.);
#10767=ADVANCED_FACE('',(#1146),#10457,.F.);
#10768=ADVANCED_FACE('',(#1147),#10458,.F.);
#10769=ADVANCED_FACE('',(#1148),#10459,.F.);
#10770=ADVANCED_FACE('',(#1149),#10460,.F.);
#10771=ADVANCED_FACE('',(#1150),#10461,.F.);
#10772=ADVANCED_FACE('',(#1151),#10462,.F.);
#10773=ADVANCED_FACE('',(#1152),#10463,.F.);
#10774=ADVANCED_FACE('',(#1153),#10464,.F.);
#10775=ADVANCED_FACE('',(#1154),#10465,.F.);
#10776=ADVANCED_FACE('',(#1155),#10466,.F.);
#10777=ADVANCED_FACE('',(#1156),#10467,.F.);
#10778=ADVANCED_FACE('',(#1157),#10468,.F.);
#10779=ADVANCED_FACE('',(#1158),#10469,.F.);
#10780=ADVANCED_FACE('',(#1159),#10470,.F.);
#10781=ADVANCED_FACE('',(#1160),#10471,.F.);
#10782=ADVANCED_FACE('',(#1161),#10472,.F.);
#10783=ADVANCED_FACE('',(#1162),#10473,.F.);
#10784=ADVANCED_FACE('',(#1163),#10474,.F.);
#10785=ADVANCED_FACE('',(#1164),#10475,.F.);
#10786=ADVANCED_FACE('',(#1165),#10476,.F.);
#10787=ADVANCED_FACE('',(#1166),#10477,.F.);
#10788=ADVANCED_FACE('',(#1167),#10478,.F.);
#10789=ADVANCED_FACE('',(#1168),#10479,.F.);
#10790=ADVANCED_FACE('',(#1169),#10480,.F.);
#10791=ADVANCED_FACE('',(#1170),#10481,.F.);
#10792=ADVANCED_FACE('',(#1171),#10482,.F.);
#10793=ADVANCED_FACE('',(#1172),#10483,.F.);
#10794=ADVANCED_FACE('',(#1173),#10484,.F.);
#10795=ADVANCED_FACE('',(#1174),#10485,.F.);
#10796=ADVANCED_FACE('',(#1175),#10486,.F.);
#10797=ADVANCED_FACE('',(#1176),#10487,.F.);
#10798=ADVANCED_FACE('',(#1177),#10488,.F.);
#10799=ADVANCED_FACE('',(#1178),#10489,.F.);
#10800=ADVANCED_FACE('',(#1179),#10490,.F.);
#10801=ADVANCED_FACE('',(#1180),#10491,.F.);
#10802=ADVANCED_FACE('',(#1181),#10492,.F.);
#10803=ADVANCED_FACE('',(#1182),#10493,.T.);
#10804=ADVANCED_FACE('',(#1183),#10494,.T.);
#10805=ADVANCED_FACE('',(#1184),#10495,.T.);
#10806=ADVANCED_FACE('',(#1185),#10496,.T.);
#10807=ADVANCED_FACE('',(#1186),#10497,.T.);
#10808=ADVANCED_FACE('',(#1187),#10498,.T.);
#10809=ADVANCED_FACE('',(#1188),#10499,.T.);
#10810=ADVANCED_FACE('',(#1189),#10500,.T.);
#10811=ADVANCED_FACE('',(#1190),#10501,.T.);
#10812=ADVANCED_FACE('',(#1191),#10502,.T.);
#10813=ADVANCED_FACE('',(#1192),#10503,.T.);
#10814=ADVANCED_FACE('',(#1193),#10504,.T.);
#10815=ADVANCED_FACE('',(#1194),#10505,.T.);
#10816=ADVANCED_FACE('',(#1195),#10506,.T.);
#10817=ADVANCED_FACE('',(#1196),#10507,.T.);
#10818=ADVANCED_FACE('',(#1197),#10508,.T.);
#10819=ADVANCED_FACE('',(#1198),#10509,.T.);
#10820=ADVANCED_FACE('',(#1199),#10510,.T.);
#10821=ADVANCED_FACE('',(#1200),#10511,.T.);
#10822=ADVANCED_FACE('',(#1201),#10512,.T.);
#10823=ADVANCED_FACE('',(#1202),#10513,.T.);
#10824=ADVANCED_FACE('',(#1203),#10514,.T.);
#10825=ADVANCED_FACE('',(#1204),#10515,.T.);
#10826=ADVANCED_FACE('',(#1205),#10516,.T.);
#10827=ADVANCED_FACE('',(#1206),#10517,.T.);
#10828=ADVANCED_FACE('',(#1207),#10518,.T.);
#10829=ADVANCED_FACE('',(#1208),#10519,.T.);
#10830=ADVANCED_FACE('',(#1209),#10520,.T.);
#10831=ADVANCED_FACE('',(#1210),#10521,.T.);
#10832=ADVANCED_FACE('',(#1211),#10522,.T.);
#10833=ADVANCED_FACE('',(#1212),#10523,.T.);
#10834=ADVANCED_FACE('',(#1213),#10524,.T.);
#10835=ADVANCED_FACE('',(#1214),#10525,.F.);
#10836=ADVANCED_FACE('',(#1215),#10526,.F.);
#10837=ADVANCED_FACE('',(#1216),#10527,.F.);
#10838=ADVANCED_FACE('',(#1217),#10528,.F.);
#10839=ADVANCED_FACE('',(#1218),#10529,.F.);
#10840=ADVANCED_FACE('',(#1219),#10530,.F.);
#10841=ADVANCED_FACE('',(#1220),#301,.T.);
#10842=ADVANCED_FACE('',(#1221),#10531,.T.);
#10843=ADVANCED_FACE('',(#1222),#302,.F.);
#10844=ADVANCED_FACE('',(#1223),#303,.F.);
#10845=ADVANCED_FACE('',(#1224),#304,.F.);
#10846=ADVANCED_FACE('',(#1225),#305,.F.);
#10847=ADVANCED_FACE('',(#1226),#289,.F.);
#10848=ADVANCED_FACE('',(#1227),#290,.F.);
#10849=ADVANCED_FACE('',(#1228),#462,.F.);
#10850=ADVANCED_FACE('',(#1229),#291,.F.);
#10851=ADVANCED_FACE('',(#1230,#132,#133,#134,#135,#136),#463,.F.);
#10852=ADVANCED_FACE('',(#1231),#292,.F.);
#10853=ADVANCED_FACE('',(#1232),#293,.F.);
#10854=ADVANCED_FACE('',(#1233),#464,.F.);
#10855=ADVANCED_FACE('',(#1234),#294,.F.);
#10856=ADVANCED_FACE('',(#1235),#295,.F.);
#10857=ADVANCED_FACE('',(#1236),#296,.F.);
#10858=ADVANCED_FACE('',(#1237),#465,.F.);
#10859=ADVANCED_FACE('',(#1238),#297,.F.);
#10860=ADVANCED_FACE('',(#1239),#298,.F.);
#10861=ADVANCED_FACE('',(#1240),#299,.F.);
#10862=ADVANCED_FACE('',(#1241),#466,.F.);
#10863=ADVANCED_FACE('',(#1242),#300,.F.);
#10864=ADVANCED_FACE('',(#1243,#137),#467,.T.);
#10865=ADVANCED_FACE('',(#1244,#138),#468,.T.);
#10866=ADVANCED_FACE('',(#1245),#469,.F.);
#10867=ADVANCED_FACE('',(#1246),#470,.F.);
#10868=ADVANCED_FACE('',(#1247),#10532,.T.);
#10869=ADVANCED_FACE('',(#1248),#471,.F.);
#10870=ADVANCED_FACE('',(#1249),#472,.F.);
#10871=ADVANCED_FACE('',(#1250),#10533,.T.);
#10872=ADVANCED_FACE('',(#1251),#473,.F.);
#10873=ADVANCED_FACE('',(#1252),#10534,.T.);
#10874=ADVANCED_FACE('',(#1253),#474,.F.);
#10875=ADVANCED_FACE('',(#1254),#10535,.T.);
#10876=ADVANCED_FACE('',(#1255),#475,.F.);
#10877=ADVANCED_FACE('',(#1256),#10536,.T.);
#10878=ADVANCED_FACE('',(#1257),#476,.F.);
#10879=ADVANCED_FACE('',(#1258),#10537,.T.);
#10880=ADVANCED_FACE('',(#1259),#10538,.T.);
#10881=ADVANCED_FACE('',(#1260),#10539,.T.);
#10882=ADVANCED_FACE('',(#1261,#139,#140,#141,#142,#143),#477,.F.);
#10883=ADVANCED_FACE('',(#1262),#306,.T.);
#10884=ADVANCED_FACE('',(#1263),#307,.T.);
#10885=ADVANCED_FACE('',(#1264),#308,.F.);
#10886=ADVANCED_FACE('',(#1265),#10540,.T.);
#10887=ADVANCED_FACE('',(#1266,#144),#478,.T.);
#10888=ADVANCED_FACE('',(#1267),#479,.T.);
#10889=ADVANCED_FACE('',(#1268),#480,.F.);
#10890=ADVANCED_FACE('',(#1269),#481,.F.);
#10891=ADVANCED_FACE('',(#1270),#10541,.F.);
#10892=ADVANCED_FACE('',(#1271),#309,.F.);
#10893=ADVANCED_FACE('',(#1272),#310,.F.);
#10894=ADVANCED_FACE('',(#1273),#311,.F.);
#10895=ADVANCED_FACE('',(#1274),#312,.F.);
#10896=ADVANCED_FACE('',(#1275),#10542,.F.);
#10897=ADVANCED_FACE('',(#1276),#10543,.F.);
#10898=ADVANCED_FACE('',(#1277),#10544,.F.);
#10899=ADVANCED_FACE('',(#1278),#10545,.F.);
#10900=ADVANCED_FACE('',(#1279),#10546,.F.);
#10901=ADVANCED_FACE('',(#1280),#482,.T.);
#10902=ADVANCED_FACE('',(#1281),#483,.T.);
#10903=ADVANCED_FACE('',(#1282),#484,.T.);
#10904=ADVANCED_FACE('',(#1283),#485,.T.);
#10905=ADVANCED_FACE('',(#1284),#486,.T.);
#10906=ADVANCED_FACE('',(#1285),#487,.F.);
#10907=ADVANCED_FACE('',(#1286),#488,.F.);
#10908=ADVANCED_FACE('',(#1287),#489,.F.);
#10909=ADVANCED_FACE('',(#1288),#490,.F.);
#10910=ADVANCED_FACE('',(#1289,#145),#491,.F.);
#10911=ADVANCED_FACE('',(#1290),#492,.F.);
#10912=ADVANCED_FACE('',(#1291,#146,#147,#148,#149,#150),#493,.T.);
#10913=ADVANCED_FACE('',(#1292),#10547,.T.);
#10914=ADVANCED_FACE('',(#1293),#10548,.T.);
#10915=ADVANCED_FACE('',(#1294),#10549,.T.);
#10916=ADVANCED_FACE('',(#1295),#494,.F.);
#10917=ADVANCED_FACE('',(#1296),#10550,.T.);
#10918=ADVANCED_FACE('',(#1297),#495,.F.);
#10919=ADVANCED_FACE('',(#1298),#10551,.T.);
#10920=ADVANCED_FACE('',(#1299),#496,.F.);
#10921=ADVANCED_FACE('',(#1300),#10552,.T.);
#10922=ADVANCED_FACE('',(#1301),#497,.F.);
#10923=ADVANCED_FACE('',(#1302),#10553,.T.);
#10924=ADVANCED_FACE('',(#1303),#498,.F.);
#10925=ADVANCED_FACE('',(#1304),#499,.F.);
#10926=ADVANCED_FACE('',(#1305),#500,.F.);
#10927=ADVANCED_FACE('',(#1306),#501,.F.);
#10928=ADVANCED_FACE('',(#1307),#502,.F.);
#10929=ADVANCED_FACE('',(#1308),#10554,.T.);
#10930=ADVANCED_FACE('',(#1309),#503,.F.);
#10931=ADVANCED_FACE('',(#1310),#504,.F.);
#10932=ADVANCED_FACE('',(#1311,#151),#505,.T.);
#10933=ADVANCED_FACE('',(#1312,#152),#506,.T.);
#10934=ADVANCED_FACE('',(#1313),#10555,.F.);
#10935=ADVANCED_FACE('',(#1314),#10556,.F.);
#10936=ADVANCED_FACE('',(#1315),#10557,.F.);
#10937=ADVANCED_FACE('',(#1316),#10558,.F.);
#10938=ADVANCED_FACE('',(#1317),#10559,.F.);
#10939=ADVANCED_FACE('',(#1318,#153),#507,.F.);
#10940=ADVANCED_FACE('',(#1319,#154,#155,#156,#157,#158),#508,.F.);
#10941=ADVANCED_FACE('',(#1320),#509,.F.);
#10942=ADVANCED_FACE('',(#1321),#510,.F.);
#10943=ADVANCED_FACE('',(#1322),#511,.F.);
#10944=ADVANCED_FACE('',(#1323),#512,.T.);
#10945=ADVANCED_FACE('',(#1324),#513,.T.);
#10946=ADVANCED_FACE('',(#1325),#514,.F.);
#10947=ADVANCED_FACE('',(#1326),#515,.T.);
#10948=ADVANCED_FACE('',(#1327),#516,.F.);
#10949=ADVANCED_FACE('',(#1328),#517,.T.);
#10950=ADVANCED_FACE('',(#1329),#518,.T.);
#10951=ADVANCED_FACE('',(#1330),#519,.T.);
#10952=ADVANCED_FACE('',(#1331),#520,.T.);
#10953=ADVANCED_FACE('',(#1332),#313,.T.);
#10954=ADVANCED_FACE('',(#1333),#10560,.T.);
#10955=ADVANCED_FACE('',(#1334,#159),#521,.F.);
#10956=ADVANCED_FACE('',(#1335),#314,.T.);
#10957=ADVANCED_FACE('',(#1336,#160),#522,.T.);
#10958=ADVANCED_FACE('',(#1337),#10561,.F.);
#10959=ADVANCED_FACE('',(#1338),#10562,.F.);
#10960=ADVANCED_FACE('',(#1339),#10563,.T.);
#10961=ADVANCED_FACE('',(#1340,#161),#523,.T.);
#10962=ADVANCED_FACE('',(#1341,#162),#524,.F.);
#10963=ADVANCED_FACE('',(#1342),#315,.F.);
#10964=ADVANCED_FACE('',(#1343),#316,.F.);
#10965=ADVANCED_FACE('',(#1344),#525,.F.);
#10966=ADVANCED_FACE('',(#1345),#526,.F.);
#10967=ADVANCED_FACE('',(#1346),#317,.T.);
#10968=ADVANCED_FACE('',(#1347),#527,.F.);
#10969=ADVANCED_FACE('',(#1348),#528,.F.);
#10970=ADVANCED_FACE('',(#1349),#529,.F.);
#10971=ADVANCED_FACE('',(#1350),#530,.F.);
#10972=ADVANCED_FACE('',(#1351,#163),#531,.T.);
#10973=ADVANCED_FACE('',(#1352),#318,.T.);
#10974=ADVANCED_FACE('',(#1353,#164),#532,.T.);
#10975=ADVANCED_FACE('',(#1354),#10564,.F.);
#10976=ADVANCED_FACE('',(#1355),#10565,.F.);
#10977=ADVANCED_FACE('',(#1356),#1023,.F.);
#10978=ADVANCED_FACE('',(#1357),#10566,.F.);
#10979=ADVANCED_FACE('',(#1358),#319,.T.);
#10980=ADVANCED_FACE('',(#1359),#10567,.T.);
#10981=ADVANCED_FACE('',(#1360),#320,.T.);
#10982=ADVANCED_FACE('',(#1361,#165),#533,.F.);
#10983=ADVANCED_FACE('',(#1362,#166),#534,.F.);
#10984=ADVANCED_FACE('',(#1363),#10568,.T.);
#10985=ADVANCED_FACE('',(#1364),#1024,.F.);
#10986=ADVANCED_FACE('',(#1365),#10569,.F.);
#10987=ADVANCED_FACE('',(#1366),#321,.F.);
#10988=ADVANCED_FACE('',(#1367,#167),#535,.F.);
#10989=ADVANCED_FACE('',(#1368,#168),#536,.F.);
#10990=ADVANCED_FACE('',(#1369),#322,.F.);
#10991=ADVANCED_FACE('',(#1370),#10570,.F.);
#10992=ADVANCED_FACE('',(#1371),#323,.F.);
#10993=ADVANCED_FACE('',(#1372),#10571,.T.);
#10994=ADVANCED_FACE('',(#1373),#1025,.F.);
#10995=ADVANCED_FACE('',(#1374),#10572,.T.);
#10996=ADVANCED_FACE('',(#1375),#324,.T.);
#10997=ADVANCED_FACE('',(#1376,#169),#537,.F.);
#10998=ADVANCED_FACE('',(#1377,#170),#538,.F.);
#10999=ADVANCED_FACE('',(#1378,#171),#539,.F.);
#11000=ADVANCED_FACE('',(#1379),#95,.T.);
#11001=ADVANCED_FACE('',(#1380),#96,.T.);
#11002=ADVANCED_FACE('',(#1381),#97,.T.);
#11003=ADVANCED_FACE('',(#1382),#98,.T.);
#11004=ADVANCED_FACE('',(#1383),#99,.T.);
#11005=ADVANCED_FACE('',(#1384),#100,.T.);
#11006=ADVANCED_FACE('',(#1385),#101,.T.);
#11007=ADVANCED_FACE('',(#1386),#102,.T.);
#11008=ADVANCED_FACE('',(#1387),#103,.T.);
#11009=ADVANCED_FACE('',(#1388),#104,.T.);
#11010=ADVANCED_FACE('',(#1389),#540,.F.);
#11011=ADVANCED_FACE('',(#1390),#541,.T.);
#11012=ADVANCED_FACE('',(#1391),#542,.F.);
#11013=ADVANCED_FACE('',(#1392),#543,.F.);
#11014=ADVANCED_FACE('',(#1393),#544,.F.);
#11015=ADVANCED_FACE('',(#1394),#10573,.F.);
#11016=ADVANCED_FACE('',(#1395),#545,.F.);
#11017=ADVANCED_FACE('',(#1396),#546,.F.);
#11018=ADVANCED_FACE('',(#1397),#547,.F.);
#11019=ADVANCED_FACE('',(#1398),#548,.F.);
#11020=ADVANCED_FACE('',(#1399),#549,.F.);
#11021=ADVANCED_FACE('',(#1400),#550,.F.);
#11022=ADVANCED_FACE('',(#1401),#551,.F.);
#11023=ADVANCED_FACE('',(#1402),#552,.F.);
#11024=ADVANCED_FACE('',(#1403),#553,.F.);
#11025=ADVANCED_FACE('',(#1404),#10574,.T.);
#11026=ADVANCED_FACE('',(#1405),#554,.F.);
#11027=ADVANCED_FACE('',(#1406),#555,.F.);
#11028=ADVANCED_FACE('',(#1407),#556,.F.);
#11029=ADVANCED_FACE('',(#1408),#557,.F.);
#11030=ADVANCED_FACE('',(#1409),#558,.F.);
#11031=ADVANCED_FACE('',(#1410),#559,.F.);
#11032=ADVANCED_FACE('',(#1411),#560,.F.);
#11033=ADVANCED_FACE('',(#1412),#561,.F.);
#11034=ADVANCED_FACE('',(#1413),#562,.F.);
#11035=ADVANCED_FACE('',(#1414),#563,.F.);
#11036=ADVANCED_FACE('',(#1415),#564,.F.);
#11037=ADVANCED_FACE('',(#1416),#565,.F.);
#11038=ADVANCED_FACE('',(#1417),#566,.F.);
#11039=ADVANCED_FACE('',(#1418),#567,.F.);
#11040=ADVANCED_FACE('',(#1419),#568,.F.);
#11041=ADVANCED_FACE('',(#1420),#569,.F.);
#11042=ADVANCED_FACE('',(#1421),#570,.F.);
#11043=ADVANCED_FACE('',(#1422),#571,.F.);
#11044=ADVANCED_FACE('',(#1423),#10575,.T.);
#11045=ADVANCED_FACE('',(#1424),#572,.F.);
#11046=ADVANCED_FACE('',(#1425),#573,.F.);
#11047=ADVANCED_FACE('',(#1426),#574,.F.);
#11048=ADVANCED_FACE('',(#1427),#575,.F.);
#11049=ADVANCED_FACE('',(#1428),#576,.F.);
#11050=ADVANCED_FACE('',(#1429),#577,.F.);
#11051=ADVANCED_FACE('',(#1430),#578,.F.);
#11052=ADVANCED_FACE('',(#1431),#579,.F.);
#11053=ADVANCED_FACE('',(#1432),#580,.F.);
#11054=ADVANCED_FACE('',(#1433),#581,.F.);
#11055=ADVANCED_FACE('',(#1434),#582,.T.);
#11056=ADVANCED_FACE('',(#1435),#583,.T.);
#11057=ADVANCED_FACE('',(#1436,#172,#173,#174),#584,.F.);
#11058=ADVANCED_FACE('',(#1437),#585,.F.);
#11059=ADVANCED_FACE('',(#1438),#586,.F.);
#11060=ADVANCED_FACE('',(#1439),#587,.T.);
#11061=ADVANCED_FACE('',(#1440),#588,.T.);
#11062=ADVANCED_FACE('',(#1441),#589,.T.);
#11063=ADVANCED_FACE('',(#1442),#10576,.F.);
#11064=ADVANCED_FACE('',(#1443),#590,.T.);
#11065=ADVANCED_FACE('',(#1444),#591,.T.);
#11066=ADVANCED_FACE('',(#1445),#592,.T.);
#11067=ADVANCED_FACE('',(#1446),#593,.T.);
#11068=ADVANCED_FACE('',(#1447),#594,.T.);
#11069=ADVANCED_FACE('',(#1448),#595,.T.);
#11070=ADVANCED_FACE('',(#1449),#596,.T.);
#11071=ADVANCED_FACE('',(#1450),#597,.T.);
#11072=ADVANCED_FACE('',(#1451),#598,.T.);
#11073=ADVANCED_FACE('',(#1452),#10577,.T.);
#11074=ADVANCED_FACE('',(#1453),#599,.T.);
#11075=ADVANCED_FACE('',(#1454),#600,.T.);
#11076=ADVANCED_FACE('',(#1455),#601,.T.);
#11077=ADVANCED_FACE('',(#1456),#602,.T.);
#11078=ADVANCED_FACE('',(#1457),#603,.T.);
#11079=ADVANCED_FACE('',(#1458),#604,.T.);
#11080=ADVANCED_FACE('',(#1459),#605,.T.);
#11081=ADVANCED_FACE('',(#1460),#606,.T.);
#11082=ADVANCED_FACE('',(#1461),#607,.T.);
#11083=ADVANCED_FACE('',(#1462),#608,.T.);
#11084=ADVANCED_FACE('',(#1463),#609,.T.);
#11085=ADVANCED_FACE('',(#1464),#610,.T.);
#11086=ADVANCED_FACE('',(#1465),#611,.T.);
#11087=ADVANCED_FACE('',(#1466),#612,.T.);
#11088=ADVANCED_FACE('',(#1467),#613,.T.);
#11089=ADVANCED_FACE('',(#1468),#614,.T.);
#11090=ADVANCED_FACE('',(#1469),#615,.T.);
#11091=ADVANCED_FACE('',(#1470),#616,.T.);
#11092=ADVANCED_FACE('',(#1471),#617,.T.);
#11093=ADVANCED_FACE('',(#1472),#10578,.T.);
#11094=ADVANCED_FACE('',(#1473),#618,.T.);
#11095=ADVANCED_FACE('',(#1474),#619,.T.);
#11096=ADVANCED_FACE('',(#1475),#620,.T.);
#11097=ADVANCED_FACE('',(#1476),#621,.T.);
#11098=ADVANCED_FACE('',(#1477),#622,.T.);
#11099=ADVANCED_FACE('',(#1478),#623,.T.);
#11100=ADVANCED_FACE('',(#1479),#624,.T.);
#11101=ADVANCED_FACE('',(#1480),#625,.T.);
#11102=ADVANCED_FACE('',(#1481),#626,.T.);
#11103=ADVANCED_FACE('',(#1482),#627,.T.);
#11104=ADVANCED_FACE('',(#1483),#628,.T.);
#11105=ADVANCED_FACE('',(#1484,#175,#176,#177),#629,.T.);
#11106=ADVANCED_FACE('',(#1485,#178),#630,.T.);
#11107=ADVANCED_FACE('',(#1486),#10579,.T.);
#11108=ADVANCED_FACE('',(#1487,#179),#631,.T.);
#11109=ADVANCED_FACE('',(#1488,#180),#632,.F.);
#11110=ADVANCED_FACE('',(#1489),#10580,.T.);
#11111=ADVANCED_FACE('',(#1490),#10581,.T.);
#11112=ADVANCED_FACE('',(#1491,#181),#633,.F.);
#11113=ADVANCED_FACE('',(#1492),#10582,.F.);
#11114=ADVANCED_FACE('',(#1493),#10583,.F.);
#11115=ADVANCED_FACE('',(#1494),#634,.T.);
#11116=ADVANCED_FACE('',(#1495),#635,.T.);
#11117=ADVANCED_FACE('',(#1496),#636,.T.);
#11118=ADVANCED_FACE('',(#1497),#637,.T.);
#11119=ADVANCED_FACE('',(#1498),#638,.T.);
#11120=ADVANCED_FACE('',(#1499),#639,.T.);
#11121=ADVANCED_FACE('',(#1500),#640,.T.);
#11122=ADVANCED_FACE('',(#1501),#641,.T.);
#11123=ADVANCED_FACE('',(#1502),#10584,.F.);
#11124=ADVANCED_FACE('',(#1503),#10585,.F.);
#11125=ADVANCED_FACE('',(#1504),#642,.T.);
#11126=ADVANCED_FACE('',(#1505),#643,.T.);
#11127=ADVANCED_FACE('',(#1506),#644,.T.);
#11128=ADVANCED_FACE('',(#1507),#645,.T.);
#11129=ADVANCED_FACE('',(#1508),#10586,.F.);
#11130=ADVANCED_FACE('',(#1509),#10587,.F.);
#11131=ADVANCED_FACE('',(#1510),#646,.T.);
#11132=ADVANCED_FACE('',(#1511),#647,.T.);
#11133=ADVANCED_FACE('',(#1512),#648,.T.);
#11134=ADVANCED_FACE('',(#1513),#649,.T.);
#11135=ADVANCED_FACE('',(#1514),#650,.T.);
#11136=ADVANCED_FACE('',(#1515),#651,.T.);
#11137=ADVANCED_FACE('',(#1516),#652,.T.);
#11138=ADVANCED_FACE('',(#1517),#653,.T.);
#11139=ADVANCED_FACE('',(#1518),#654,.T.);
#11140=ADVANCED_FACE('',(#1519),#10588,.T.);
#11141=ADVANCED_FACE('',(#1520),#655,.T.);
#11142=ADVANCED_FACE('',(#1521),#10589,.T.);
#11143=ADVANCED_FACE('',(#1522),#656,.T.);
#11144=ADVANCED_FACE('',(#1523),#10590,.T.);
#11145=ADVANCED_FACE('',(#1524),#657,.T.);
#11146=ADVANCED_FACE('',(#1525),#10591,.T.);
#11147=ADVANCED_FACE('',(#1526,#182,#183,#184,#185,#186,#187,#188,#189),
#658,.T.);
#11148=ADVANCED_FACE('',(#1527,#190,#191,#192,#193,#194,#195,#196,#197),
#659,.F.);
#11149=ADVANCED_FACE('',(#1528),#10592,.F.);
#11150=ADVANCED_FACE('',(#1529),#10593,.F.);
#11151=ADVANCED_FACE('',(#1530,#198),#10594,.T.);
#11152=ADVANCED_FACE('',(#1531,#199),#660,.T.);
#11153=ADVANCED_FACE('',(#1532,#200),#661,.F.);
#11154=ADVANCED_FACE('',(#1533),#10595,.T.);
#11155=ADVANCED_FACE('',(#1534,#201),#662,.T.);
#11156=ADVANCED_FACE('',(#1535),#10596,.T.);
#11157=ADVANCED_FACE('',(#1536,#202),#10597,.F.);
#11158=ADVANCED_FACE('',(#1537),#10598,.T.);
#11159=ADVANCED_FACE('',(#1538,#203),#663,.T.);
#11160=ADVANCED_FACE('',(#1539,#204),#664,.F.);
#11161=ADVANCED_FACE('',(#1540,#205),#665,.F.);
#11162=ADVANCED_FACE('',(#1541),#666,.T.);
#11163=ADVANCED_FACE('',(#1542),#10599,.F.);
#11164=ADVANCED_FACE('',(#1543),#667,.T.);
#11165=ADVANCED_FACE('',(#1544),#10600,.F.);
#11166=ADVANCED_FACE('',(#1545),#668,.T.);
#11167=ADVANCED_FACE('',(#1546),#10601,.T.);
#11168=ADVANCED_FACE('',(#1547),#669,.T.);
#11169=ADVANCED_FACE('',(#1548),#10602,.T.);
#11170=ADVANCED_FACE('',(#1549,#206),#670,.T.);
#11171=ADVANCED_FACE('',(#1550),#10603,.F.);
#11172=ADVANCED_FACE('',(#1551),#671,.T.);
#11173=ADVANCED_FACE('',(#1552),#10604,.F.);
#11174=ADVANCED_FACE('',(#1553),#672,.T.);
#11175=ADVANCED_FACE('',(#1554),#10605,.F.);
#11176=ADVANCED_FACE('',(#1555),#10606,.F.);
#11177=ADVANCED_FACE('',(#1556),#10607,.F.);
#11178=ADVANCED_FACE('',(#1557),#10608,.F.);
#11179=ADVANCED_FACE('',(#1558),#10609,.F.);
#11180=ADVANCED_FACE('',(#1559),#10610,.F.);
#11181=ADVANCED_FACE('',(#1560),#673,.T.);
#11182=ADVANCED_FACE('',(#1561),#10611,.F.);
#11183=ADVANCED_FACE('',(#1562),#674,.T.);
#11184=ADVANCED_FACE('',(#1563),#10612,.F.);
#11185=ADVANCED_FACE('',(#1564),#675,.T.);
#11186=ADVANCED_FACE('',(#1565),#10613,.F.);
#11187=ADVANCED_FACE('',(#1566),#676,.T.);
#11188=ADVANCED_FACE('',(#1567),#10614,.F.);
#11189=ADVANCED_FACE('',(#1568),#10615,.F.);
#11190=ADVANCED_FACE('',(#1569),#10616,.F.);
#11191=ADVANCED_FACE('',(#1570),#10617,.F.);
#11192=ADVANCED_FACE('',(#1571),#10618,.F.);
#11193=ADVANCED_FACE('',(#1572),#10619,.F.);
#11194=ADVANCED_FACE('',(#1573),#677,.T.);
#11195=ADVANCED_FACE('',(#1574),#10620,.F.);
#11196=ADVANCED_FACE('',(#1575),#678,.T.);
#11197=ADVANCED_FACE('',(#1576),#10621,.F.);
#11198=ADVANCED_FACE('',(#1577),#10622,.F.);
#11199=ADVANCED_FACE('',(#1578),#10623,.F.);
#11200=ADVANCED_FACE('',(#1579),#679,.T.);
#11201=ADVANCED_FACE('',(#1580),#10624,.F.);
#11202=ADVANCED_FACE('',(#1581),#680,.T.);
#11203=ADVANCED_FACE('',(#1582),#10625,.F.);
#11204=ADVANCED_FACE('',(#1583),#681,.T.);
#11205=ADVANCED_FACE('',(#1584),#10626,.F.);
#11206=ADVANCED_FACE('',(#1585),#682,.T.);
#11207=ADVANCED_FACE('',(#1586),#10627,.F.);
#11208=ADVANCED_FACE('',(#1587),#683,.T.);
#11209=ADVANCED_FACE('',(#1588),#10628,.F.);
#11210=ADVANCED_FACE('',(#1589),#684,.T.);
#11211=ADVANCED_FACE('',(#1590),#10629,.F.);
#11212=ADVANCED_FACE('',(#1591),#685,.T.);
#11213=ADVANCED_FACE('',(#1592),#10630,.F.);
#11214=ADVANCED_FACE('',(#1593),#686,.T.);
#11215=ADVANCED_FACE('',(#1594),#10631,.F.);
#11216=ADVANCED_FACE('',(#1595),#10632,.F.);
#11217=ADVANCED_FACE('',(#1596),#10633,.F.);
#11218=ADVANCED_FACE('',(#1597),#687,.T.);
#11219=ADVANCED_FACE('',(#1598),#10634,.T.);
#11220=ADVANCED_FACE('',(#1599),#688,.T.);
#11221=ADVANCED_FACE('',(#1600),#10635,.T.);
#11222=ADVANCED_FACE('',(#1601),#689,.T.);
#11223=ADVANCED_FACE('',(#1602),#10636,.T.);
#11224=ADVANCED_FACE('',(#1603),#690,.T.);
#11225=ADVANCED_FACE('',(#1604),#10637,.T.);
#11226=ADVANCED_FACE('',(#1605,#207,#208,#209,#210,#211,#212,#213,#214,
#215,#216,#217,#218,#219,#220,#221,#222,#223,#224,#225,#226,#227,#228,#229),
#691,.T.);
#11227=ADVANCED_FACE('',(#1606,#230,#231,#232,#233,#234,#235,#236,#237,
#238,#239,#240,#241,#242,#243,#244,#245,#246,#247,#248,#249,#250,#251,#252),
#692,.F.);
#11228=ADVANCED_FACE('',(#1607),#10638,.F.);
#11229=ADVANCED_FACE('',(#1608),#10639,.F.);
#11230=ADVANCED_FACE('',(#1609),#10640,.F.);
#11231=ADVANCED_FACE('',(#1610),#10641,.F.);
#11232=ADVANCED_FACE('',(#1611),#10642,.F.);
#11233=ADVANCED_FACE('',(#1612),#10643,.T.);
#11234=ADVANCED_FACE('',(#1613),#693,.T.);
#11235=ADVANCED_FACE('',(#1614),#10644,.T.);
#11236=ADVANCED_FACE('',(#1615),#694,.T.);
#11237=ADVANCED_FACE('',(#1616),#10645,.T.);
#11238=ADVANCED_FACE('',(#1617),#695,.T.);
#11239=ADVANCED_FACE('',(#1618),#10646,.T.);
#11240=ADVANCED_FACE('',(#1619),#696,.T.);
#11241=ADVANCED_FACE('',(#1620,#253,#254,#255,#256,#257),#697,.T.);
#11242=ADVANCED_FACE('',(#1621,#258,#259,#260,#261,#262),#698,.F.);
#11243=ADVANCED_FACE('',(#1622),#325,.T.);
#11244=ADVANCED_FACE('',(#1623),#1026,.F.);
#11245=ADVANCED_FACE('',(#1624,#263),#699,.T.);
#11246=ADVANCED_FACE('',(#1625),#10647,.T.);
#11247=ADVANCED_FACE('',(#1626),#700,.F.);
#11248=ADVANCED_FACE('',(#1627),#701,.F.);
#11249=ADVANCED_FACE('',(#1628),#702,.F.);
#11250=ADVANCED_FACE('',(#1629),#703,.F.);
#11251=ADVANCED_FACE('',(#1630),#704,.F.);
#11252=ADVANCED_FACE('',(#1631),#705,.F.);
#11253=ADVANCED_FACE('',(#1632),#706,.F.);
#11254=ADVANCED_FACE('',(#1633),#707,.F.);
#11255=ADVANCED_FACE('',(#1634),#708,.F.);
#11256=ADVANCED_FACE('',(#1635),#709,.F.);
#11257=ADVANCED_FACE('',(#1636),#710,.F.);
#11258=ADVANCED_FACE('',(#1637),#711,.F.);
#11259=ADVANCED_FACE('',(#1638),#712,.T.);
#11260=ADVANCED_FACE('',(#1639,#264),#713,.T.);
#11261=ADVANCED_FACE('',(#1640),#105,.T.);
#11262=CLOSED_SHELL('',(#10648,#10649,#10650,#10651,#10652,#10653,#10654,
#10655,#10656,#10657,#10658,#10659,#10660,#10661,#10662,#10663,#10664,#10665,
#10666,#10667));
#11263=CLOSED_SHELL('',(#10668,#10669,#10670,#10671,#10672,#10673,#10674,
#10675,#10676,#10677,#10678,#10679,#10680,#10681,#10682,#10683,#10684,#10685,
#10686,#10687));
#11264=CLOSED_SHELL('',(#10688,#10689,#10690,#10691,#10692,#10693,#10694,
#10695,#10696,#10697,#10698,#10699,#10700,#10701,#10702,#10703,#10704,#10705,
#10706,#10707));
#11265=CLOSED_SHELL('',(#10708,#10709,#10710,#10711,#10712,#10713,#10714,
#10715,#10716,#10717,#10718,#10719,#10720,#10721,#10722,#10723,#10724,#10725,
#10726,#10727));
#11266=CLOSED_SHELL('',(#10728,#10729,#10730,#10731,#10732,#10733,#10734,
#10735,#10736,#10737,#10738,#10739,#10740,#10741,#10742,#10743,#10744,#10745,
#10746,#10747,#10748,#10749,#10750,#10751,#10752,#10753,#10754,#10755,#10756,
#10757,#10758,#10759,#10760,#10761,#10762,#10763,#10764,#10765,#10766,#10767,
#10768,#10769,#10770,#10771,#10772,#10773,#10774,#10775,#10776,#10777,#10778,
#10779,#10780,#10781,#10782,#10783,#10784,#10785,#10786,#10787,#10788,#10789,
#10790,#10791,#10792,#10793,#10794,#10795,#10796,#10797,#10798,#10799,#10800,
#10801,#10802,#10803,#10804,#10805,#10806,#10807,#10808,#10809,#10810,#10811,
#10812,#10813,#10814,#10815,#10816,#10817,#10818,#10819,#10820,#10821,#10822,
#10823,#10824,#10825,#10826,#10827,#10828,#10829,#10830,#10831,#10832,#10833,
#10834,#10835,#10836,#10837,#10838,#10839,#10840,#10841,#10842,#10843,#10844,
#10845,#10846,#10847,#10848,#10849,#10850,#10851,#10852,#10853,#10854,#10855,
#10856,#10857,#10858,#10859,#10860,#10861,#10862,#10863,#10864,#10865,#10866,
#10867,#10868,#10869,#10870,#10871,#10872,#10873,#10874,#10875,#10876,#10877,
#10878,#10879,#10880,#10881,#10882));
#11267=CLOSED_SHELL('',(#10883,#10884,#10885,#10886,#10887,#10888,#10889,
#10890));
#11268=CLOSED_SHELL('',(#10891,#10892,#10893,#10894,#10895,#10896,#10897,
#10898,#10899,#10900,#10901,#10902,#10903,#10904,#10905,#10906,#10907,#10908,
#10909,#10910,#10911,#10912,#10913,#10914,#10915,#10916,#10917,#10918,#10919,
#10920,#10921,#10922,#10923,#10924,#10925,#10926,#10927,#10928,#10929,#10930,
#10931,#10932,#10933));
#11269=CLOSED_SHELL('',(#10934,#10935,#10936,#10937,#10938,#10939,#10940,
#10941,#10942,#10943,#10944,#10945,#10946,#10947,#10948,#10949,#10950,#10951,
#10952));
#11270=CLOSED_SHELL('',(#10953,#10954,#10955,#10956,#10957,#10958));
#11271=CLOSED_SHELL('',(#10959,#10960,#10961,#10962));
#11272=CLOSED_SHELL('',(#10963,#10964,#10965,#10966,#10967,#10968,#10969,
#10970,#10971,#10972,#10973,#10974,#10975));
#11273=CLOSED_SHELL('',(#10976,#10977,#10978,#10979,#10980,#10981,#10982,
#10983));
#11274=CLOSED_SHELL('',(#10984,#10985,#10986,#10987,#10988,#10989));
#11275=CLOSED_SHELL('',(#10990,#10991,#10992,#10993,#10994,#10995,#10996,
#10997,#10998,#10999));
#11276=CLOSED_SHELL('',(#11000));
#11277=CLOSED_SHELL('',(#11001));
#11278=CLOSED_SHELL('',(#11002));
#11279=CLOSED_SHELL('',(#11003));
#11280=CLOSED_SHELL('',(#11004));
#11281=CLOSED_SHELL('',(#11005));
#11282=CLOSED_SHELL('',(#11006));
#11283=CLOSED_SHELL('',(#11007));
#11284=CLOSED_SHELL('',(#11008));
#11285=CLOSED_SHELL('',(#11009));
#11286=CLOSED_SHELL('',(#11010,#11011,#11012,#11013,#11014,#11015,#11016,
#11017,#11018,#11019,#11020,#11021,#11022,#11023,#11024,#11025,#11026,#11027,
#11028,#11029,#11030,#11031,#11032,#11033,#11034,#11035,#11036,#11037,#11038,
#11039,#11040,#11041,#11042,#11043,#11044,#11045,#11046,#11047,#11048,#11049,
#11050,#11051,#11052,#11053,#11054,#11055,#11056,#11057,#11058,#11059,#11060,
#11061,#11062,#11063,#11064,#11065,#11066,#11067,#11068,#11069,#11070,#11071,
#11072,#11073,#11074,#11075,#11076,#11077,#11078,#11079,#11080,#11081,#11082,
#11083,#11084,#11085,#11086,#11087,#11088,#11089,#11090,#11091,#11092,#11093,
#11094,#11095,#11096,#11097,#11098,#11099,#11100,#11101,#11102,#11103,#11104,
#11105));
#11287=CLOSED_SHELL('',(#11106,#11107,#11108,#11109,#11110,#11111,#11112,
#11113));
#11288=CLOSED_SHELL('',(#11114,#11115,#11116,#11117,#11118,#11119,#11120,
#11121,#11122,#11123,#11124,#11125,#11126,#11127,#11128,#11129,#11130,#11131,
#11132,#11133,#11134,#11135,#11136,#11137,#11138,#11139,#11140,#11141,#11142,
#11143,#11144,#11145,#11146,#11147,#11148));
#11289=CLOSED_SHELL('',(#11149,#11150,#11151,#11152,#11153,#11154,#11155,
#11156,#11157,#11158,#11159,#11160));
#11290=CLOSED_SHELL('',(#11161,#11162,#11163,#11164,#11165,#11166,#11167,
#11168,#11169,#11170));
#11291=CLOSED_SHELL('',(#11171,#11172,#11173,#11174,#11175,#11176,#11177,
#11178,#11179,#11180,#11181,#11182,#11183,#11184,#11185,#11186,#11187,#11188,
#11189,#11190,#11191,#11192,#11193,#11194,#11195,#11196,#11197,#11198,#11199,
#11200,#11201,#11202,#11203,#11204,#11205,#11206,#11207,#11208,#11209,#11210,
#11211,#11212,#11213,#11214,#11215,#11216,#11217,#11218,#11219,#11220,#11221,
#11222,#11223,#11224,#11225,#11226,#11227));
#11292=CLOSED_SHELL('',(#11228,#11229,#11230,#11231,#11232,#11233,#11234,
#11235,#11236,#11237,#11238,#11239,#11240,#11241,#11242));
#11293=CLOSED_SHELL('',(#11243,#11244,#11245,#11246,#11247,#11248,#11249,
#11250,#11251,#11252,#11253,#11254,#11255,#11256,#11257,#11258,#11259,#11260,
#11261));
#11294=DERIVED_UNIT_ELEMENT(#11320,1.);
#11295=DERIVED_UNIT_ELEMENT(#36462,-3.);
#11296=DERIVED_UNIT_ELEMENT(#11320,1.);
#11297=DERIVED_UNIT_ELEMENT(#36462,-3.);
#11298=DERIVED_UNIT_ELEMENT(#11320,1.);
#11299=DERIVED_UNIT_ELEMENT(#36462,-3.);
#11300=DERIVED_UNIT_ELEMENT(#11320,1.);
#11301=DERIVED_UNIT_ELEMENT(#36462,-3.);
#11302=DERIVED_UNIT_ELEMENT(#11320,1.);
#11303=DERIVED_UNIT_ELEMENT(#36462,-3.);
#11304=DERIVED_UNIT_ELEMENT(#11320,1.);
#11305=DERIVED_UNIT_ELEMENT(#36462,-3.);
#11306=DERIVED_UNIT_ELEMENT(#11320,1.);
#11307=DERIVED_UNIT_ELEMENT(#36462,-3.);
#11308=DERIVED_UNIT_ELEMENT(#11320,1.);
#11309=DERIVED_UNIT_ELEMENT(#36462,-3.);
#11310=DERIVED_UNIT_ELEMENT(#11320,1.);
#11311=DERIVED_UNIT_ELEMENT(#36462,-3.);
#11312=DERIVED_UNIT_ELEMENT(#11320,1.);
#11313=DERIVED_UNIT_ELEMENT(#36462,-3.);
#11314=DERIVED_UNIT_ELEMENT(#11320,1.);
#11315=DERIVED_UNIT_ELEMENT(#36462,-3.);
#11316=DERIVED_UNIT_ELEMENT(#11320,1.);
#11317=DERIVED_UNIT_ELEMENT(#36462,-3.);
#11318=DERIVED_UNIT_ELEMENT(#11320,1.);
#11319=DERIVED_UNIT_ELEMENT(#36462,-3.);
#11320=(
MASS_UNIT()
NAMED_UNIT(*)
SI_UNIT(.KILO.,.GRAM.)
);
#11321=DERIVED_UNIT((#11294,#11295));
#11322=DERIVED_UNIT((#11296,#11297));
#11323=DERIVED_UNIT((#11298,#11299));
#11324=DERIVED_UNIT((#11300,#11301));
#11325=DERIVED_UNIT((#11302,#11303));
#11326=DERIVED_UNIT((#11304,#11305));
#11327=DERIVED_UNIT((#11306,#11307));
#11328=DERIVED_UNIT((#11308,#11309));
#11329=DERIVED_UNIT((#11310,#11311));
#11330=DERIVED_UNIT((#11312,#11313));
#11331=DERIVED_UNIT((#11314,#11315));
#11332=DERIVED_UNIT((#11316,#11317));
#11333=DERIVED_UNIT((#11318,#11319));
#11334=MEASURE_REPRESENTATION_ITEM('density measure',
POSITIVE_RATIO_MEASURE(7850.),#11321);
#11335=MEASURE_REPRESENTATION_ITEM('density measure',
POSITIVE_RATIO_MEASURE(7850.),#11322);
#11336=MEASURE_REPRESENTATION_ITEM('density measure',
POSITIVE_RATIO_MEASURE(7850.),#11323);
#11337=MEASURE_REPRESENTATION_ITEM('density measure',
POSITIVE_RATIO_MEASURE(8030.),#11324);
#11338=MEASURE_REPRESENTATION_ITEM('density measure',
POSITIVE_RATIO_MEASURE(7850.),#11325);
#11339=MEASURE_REPRESENTATION_ITEM('density measure',
POSITIVE_RATIO_MEASURE(7850.),#11326);
#11340=MEASURE_REPRESENTATION_ITEM('density measure',
POSITIVE_RATIO_MEASURE(7850.),#11327);
#11341=MEASURE_REPRESENTATION_ITEM('density measure',
POSITIVE_RATIO_MEASURE(7850.),#11328);
#11342=MEASURE_REPRESENTATION_ITEM('density measure',
POSITIVE_RATIO_MEASURE(7850.),#11329);
#11343=MEASURE_REPRESENTATION_ITEM('density measure',
POSITIVE_RATIO_MEASURE(7850.),#11330);
#11344=MEASURE_REPRESENTATION_ITEM('density measure',
POSITIVE_RATIO_MEASURE(7850.),#11331);
#11345=MEASURE_REPRESENTATION_ITEM('density measure',
POSITIVE_RATIO_MEASURE(7850.),#11332);
#11346=MEASURE_REPRESENTATION_ITEM('density measure',
POSITIVE_RATIO_MEASURE(7750.),#11333);
#11347=PROPERTY_DEFINITION_REPRESENTATION(#11412,#11373);
#11348=PROPERTY_DEFINITION_REPRESENTATION(#11413,#11374);
#11349=PROPERTY_DEFINITION_REPRESENTATION(#11414,#11375);
#11350=PROPERTY_DEFINITION_REPRESENTATION(#11415,#11376);
#11351=PROPERTY_DEFINITION_REPRESENTATION(#11416,#11377);
#11352=PROPERTY_DEFINITION_REPRESENTATION(#11417,#11378);
#11353=PROPERTY_DEFINITION_REPRESENTATION(#11418,#11379);
#11354=PROPERTY_DEFINITION_REPRESENTATION(#11419,#11380);
#11355=PROPERTY_DEFINITION_REPRESENTATION(#11420,#11381);
#11356=PROPERTY_DEFINITION_REPRESENTATION(#11421,#11382);
#11357=PROPERTY_DEFINITION_REPRESENTATION(#11422,#11383);
#11358=PROPERTY_DEFINITION_REPRESENTATION(#11423,#11384);
#11359=PROPERTY_DEFINITION_REPRESENTATION(#11424,#11385);
#11360=PROPERTY_DEFINITION_REPRESENTATION(#11425,#11386);
#11361=PROPERTY_DEFINITION_REPRESENTATION(#11426,#11387);
#11362=PROPERTY_DEFINITION_REPRESENTATION(#11427,#11388);
#11363=PROPERTY_DEFINITION_REPRESENTATION(#11428,#11389);
#11364=PROPERTY_DEFINITION_REPRESENTATION(#11429,#11390);
#11365=PROPERTY_DEFINITION_REPRESENTATION(#11430,#11391);
#11366=PROPERTY_DEFINITION_REPRESENTATION(#11431,#11392);
#11367=PROPERTY_DEFINITION_REPRESENTATION(#11432,#11393);
#11368=PROPERTY_DEFINITION_REPRESENTATION(#11433,#11394);
#11369=PROPERTY_DEFINITION_REPRESENTATION(#11434,#11395);
#11370=PROPERTY_DEFINITION_REPRESENTATION(#11435,#11396);
#11371=PROPERTY_DEFINITION_REPRESENTATION(#11436,#11397);
#11372=PROPERTY_DEFINITION_REPRESENTATION(#11437,#11398);
#11373=REPRESENTATION('material name',(#11399),#36446);
#11374=REPRESENTATION('density',(#11334),#36446);
#11375=REPRESENTATION('material name',(#11400),#36448);
#11376=REPRESENTATION('density',(#11335),#36448);
#11377=REPRESENTATION('material name',(#11401),#36449);
#11378=REPRESENTATION('density',(#11336),#36449);
#11379=REPRESENTATION('material name',(#11402),#36450);
#11380=REPRESENTATION('density',(#11337),#36450);
#11381=REPRESENTATION('material name',(#11403),#36451);
#11382=REPRESENTATION('density',(#11338),#36451);
#11383=REPRESENTATION('material name',(#11404),#36452);
#11384=REPRESENTATION('density',(#11339),#36452);
#11385=REPRESENTATION('material name',(#11405),#36453);
#11386=REPRESENTATION('density',(#11340),#36453);
#11387=REPRESENTATION('material name',(#11406),#36454);
#11388=REPRESENTATION('density',(#11341),#36454);
#11389=REPRESENTATION('material name',(#11407),#36455);
#11390=REPRESENTATION('density',(#11342),#36455);
#11391=REPRESENTATION('material name',(#11408),#36456);
#11392=REPRESENTATION('density',(#11343),#36456);
#11393=REPRESENTATION('material name',(#11409),#36457);
#11394=REPRESENTATION('density',(#11344),#36457);
#11395=REPRESENTATION('material name',(#11410),#36458);
#11396=REPRESENTATION('density',(#11345),#36458);
#11397=REPRESENTATION('material name',(#11411),#36459);
#11398=REPRESENTATION('density',(#11346),#36459);
#11399=DESCRIPTIVE_REPRESENTATION_ITEM('Steel','Steel');
#11400=DESCRIPTIVE_REPRESENTATION_ITEM('Steel','Steel');
#11401=DESCRIPTIVE_REPRESENTATION_ITEM('Steel','Steel');
#11402=DESCRIPTIVE_REPRESENTATION_ITEM('Steel 6, Plain',
'Steel 6, Plain');
#11403=DESCRIPTIVE_REPRESENTATION_ITEM('Steel','Steel');
#11404=DESCRIPTIVE_REPRESENTATION_ITEM('Steel','Steel');
#11405=DESCRIPTIVE_REPRESENTATION_ITEM('Steel','Steel');
#11406=DESCRIPTIVE_REPRESENTATION_ITEM('Steel','Steel');
#11407=DESCRIPTIVE_REPRESENTATION_ITEM('Steel','Steel');
#11408=DESCRIPTIVE_REPRESENTATION_ITEM('Steel','Steel');
#11409=DESCRIPTIVE_REPRESENTATION_ITEM('Steel','Steel');
#11410=DESCRIPTIVE_REPRESENTATION_ITEM('Steel','Steel');
#11411=DESCRIPTIVE_REPRESENTATION_ITEM('Steel Grade 2, Plain',
'Steel Grade 2, Plain');
#11412=PROPERTY_DEFINITION('material property','material name',#36533);
#11413=PROPERTY_DEFINITION('material property','density of part',#36533);
#11414=PROPERTY_DEFINITION('material property','material name',#36535);
#11415=PROPERTY_DEFINITION('material property','density of part',#36535);
#11416=PROPERTY_DEFINITION('material property','material name',#36536);
#11417=PROPERTY_DEFINITION('material property','density of part',#36536);
#11418=PROPERTY_DEFINITION('material property','material name',#36537);
#11419=PROPERTY_DEFINITION('material property','density of part',#36537);
#11420=PROPERTY_DEFINITION('material property','material name',#36538);
#11421=PROPERTY_DEFINITION('material property','density of part',#36538);
#11422=PROPERTY_DEFINITION('material property','material name',#36539);
#11423=PROPERTY_DEFINITION('material property','density of part',#36539);
#11424=PROPERTY_DEFINITION('material property','material name',#36540);
#11425=PROPERTY_DEFINITION('material property','density of part',#36540);
#11426=PROPERTY_DEFINITION('material property','material name',#36541);
#11427=PROPERTY_DEFINITION('material property','density of part',#36541);
#11428=PROPERTY_DEFINITION('material property','material name',#36542);
#11429=PROPERTY_DEFINITION('material property','density of part',#36542);
#11430=PROPERTY_DEFINITION('material property','material name',#36543);
#11431=PROPERTY_DEFINITION('material property','density of part',#36543);
#11432=PROPERTY_DEFINITION('material property','material name',#36544);
#11433=PROPERTY_DEFINITION('material property','density of part',#36544);
#11434=PROPERTY_DEFINITION('material property','material name',#36545);
#11435=PROPERTY_DEFINITION('material property','density of part',#36545);
#11436=PROPERTY_DEFINITION('material property','material name',#36546);
#11437=PROPERTY_DEFINITION('material property','density of part',#36546);
#11438=AXIS2_PLACEMENT_3D('',#15381,#12437,#12438);
#11439=AXIS2_PLACEMENT_3D('',#15382,#12439,#12440);
#11440=AXIS2_PLACEMENT_3D('',#15383,#12441,#12442);
#11441=AXIS2_PLACEMENT_3D('',#15385,#12443,#12444);
#11442=AXIS2_PLACEMENT_3D('',#15389,#12446,#12447);
#11443=AXIS2_PLACEMENT_3D('',#15390,#12448,#12449);
#11444=AXIS2_PLACEMENT_3D('',#15391,#12450,#12451);
#11445=AXIS2_PLACEMENT_3D('',#15398,#12452,#12453);
#11446=AXIS2_PLACEMENT_3D('',#15405,#12454,#12455);
#11447=AXIS2_PLACEMENT_3D('',#15407,#12456,#12457);
#11448=AXIS2_PLACEMENT_3D('',#15409,#12458,#12459);
#11449=AXIS2_PLACEMENT_3D('',#15418,#12460,#12461);
#11450=AXIS2_PLACEMENT_3D('',#15420,#12462,#12463);
#11451=AXIS2_PLACEMENT_3D('',#15422,#12464,#12465);
#11452=AXIS2_PLACEMENT_3D('',#15431,#12466,#12467);
#11453=AXIS2_PLACEMENT_3D('',#15433,#12468,#12469);
#11454=AXIS2_PLACEMENT_3D('',#15435,#12470,#12471);
#11455=AXIS2_PLACEMENT_3D('',#15444,#12472,#12473);
#11456=AXIS2_PLACEMENT_3D('',#15446,#12474,#12475);
#11457=AXIS2_PLACEMENT_3D('',#15447,#12476,#12477);
#11458=AXIS2_PLACEMENT_3D('',#15448,#12478,#12479);
#11459=AXIS2_PLACEMENT_3D('',#15452,#12482,#12483);
#11460=AXIS2_PLACEMENT_3D('',#15456,#12486,#12487);
#11461=AXIS2_PLACEMENT_3D('',#15460,#12490,#12491);
#11462=AXIS2_PLACEMENT_3D('',#15461,#12492,#12493);
#11463=AXIS2_PLACEMENT_3D('',#15465,#12496,#12497);
#11464=AXIS2_PLACEMENT_3D('',#15471,#12501,#12502);
#11465=AXIS2_PLACEMENT_3D('',#15477,#12506,#12507);
#11466=AXIS2_PLACEMENT_3D('',#15483,#12511,#12512);
#11467=AXIS2_PLACEMENT_3D('',#15485,#12514,#12515);
#11468=AXIS2_PLACEMENT_3D('',#15491,#12519,#12520);
#11469=AXIS2_PLACEMENT_3D('',#15493,#12522,#12523);
#11470=AXIS2_PLACEMENT_3D('',#15504,#12530,#12531);
#11471=AXIS2_PLACEMENT_3D('',#15507,#12534,#12535);
#11472=AXIS2_PLACEMENT_3D('',#15508,#12536,#12537);
#11473=AXIS2_PLACEMENT_3D('',#15509,#12538,#12539);
#11474=AXIS2_PLACEMENT_3D('',#15511,#12541,#12542);
#11475=AXIS2_PLACEMENT_3D('',#15513,#12544,#12545);
#11476=AXIS2_PLACEMENT_3D('',#15514,#12546,#12547);
#11477=AXIS2_PLACEMENT_3D('',#15516,#12548,#12549);
#11478=AXIS2_PLACEMENT_3D('',#15520,#12551,#12552);
#11479=AXIS2_PLACEMENT_3D('',#15521,#12553,#12554);
#11480=AXIS2_PLACEMENT_3D('',#15522,#12555,#12556);
#11481=AXIS2_PLACEMENT_3D('',#15529,#12557,#12558);
#11482=AXIS2_PLACEMENT_3D('',#15536,#12559,#12560);
#11483=AXIS2_PLACEMENT_3D('',#15538,#12561,#12562);
#11484=AXIS2_PLACEMENT_3D('',#15540,#12563,#12564);
#11485=AXIS2_PLACEMENT_3D('',#15549,#12565,#12566);
#11486=AXIS2_PLACEMENT_3D('',#15551,#12567,#12568);
#11487=AXIS2_PLACEMENT_3D('',#15553,#12569,#12570);
#11488=AXIS2_PLACEMENT_3D('',#15562,#12571,#12572);
#11489=AXIS2_PLACEMENT_3D('',#15564,#12573,#12574);
#11490=AXIS2_PLACEMENT_3D('',#15566,#12575,#12576);
#11491=AXIS2_PLACEMENT_3D('',#15575,#12577,#12578);
#11492=AXIS2_PLACEMENT_3D('',#15577,#12579,#12580);
#11493=AXIS2_PLACEMENT_3D('',#15578,#12581,#12582);
#11494=AXIS2_PLACEMENT_3D('',#15579,#12583,#12584);
#11495=AXIS2_PLACEMENT_3D('',#15583,#12587,#12588);
#11496=AXIS2_PLACEMENT_3D('',#15587,#12591,#12592);
#11497=AXIS2_PLACEMENT_3D('',#15591,#12595,#12596);
#11498=AXIS2_PLACEMENT_3D('',#15592,#12597,#12598);
#11499=AXIS2_PLACEMENT_3D('',#15596,#12601,#12602);
#11500=AXIS2_PLACEMENT_3D('',#15602,#12606,#12607);
#11501=AXIS2_PLACEMENT_3D('',#15608,#12611,#12612);
#11502=AXIS2_PLACEMENT_3D('',#15614,#12616,#12617);
#11503=AXIS2_PLACEMENT_3D('',#15616,#12619,#12620);
#11504=AXIS2_PLACEMENT_3D('',#15622,#12624,#12625);
#11505=AXIS2_PLACEMENT_3D('',#15624,#12627,#12628);
#11506=AXIS2_PLACEMENT_3D('',#15635,#12635,#12636);
#11507=AXIS2_PLACEMENT_3D('',#15638,#12639,#12640);
#11508=AXIS2_PLACEMENT_3D('',#15639,#12641,#12642);
#11509=AXIS2_PLACEMENT_3D('',#15640,#12643,#12644);
#11510=AXIS2_PLACEMENT_3D('',#15642,#12646,#12647);
#11511=AXIS2_PLACEMENT_3D('',#15644,#12649,#12650);
#11512=AXIS2_PLACEMENT_3D('',#15645,#12651,#12652);
#11513=AXIS2_PLACEMENT_3D('',#15647,#12653,#12654);
#11514=AXIS2_PLACEMENT_3D('',#15651,#12656,#12657);
#11515=AXIS2_PLACEMENT_3D('',#15652,#12658,#12659);
#11516=AXIS2_PLACEMENT_3D('',#15653,#12660,#12661);
#11517=AXIS2_PLACEMENT_3D('',#15660,#12662,#12663);
#11518=AXIS2_PLACEMENT_3D('',#15667,#12664,#12665);
#11519=AXIS2_PLACEMENT_3D('',#15669,#12666,#12667);
#11520=AXIS2_PLACEMENT_3D('',#15671,#12668,#12669);
#11521=AXIS2_PLACEMENT_3D('',#15680,#12670,#12671);
#11522=AXIS2_PLACEMENT_3D('',#15682,#12672,#12673);
#11523=AXIS2_PLACEMENT_3D('',#15684,#12674,#12675);
#11524=AXIS2_PLACEMENT_3D('',#15693,#12676,#12677);
#11525=AXIS2_PLACEMENT_3D('',#15695,#12678,#12679);
#11526=AXIS2_PLACEMENT_3D('',#15697,#12680,#12681);
#11527=AXIS2_PLACEMENT_3D('',#15706,#12682,#12683);
#11528=AXIS2_PLACEMENT_3D('',#15708,#12684,#12685);
#11529=AXIS2_PLACEMENT_3D('',#15709,#12686,#12687);
#11530=AXIS2_PLACEMENT_3D('',#15710,#12688,#12689);
#11531=AXIS2_PLACEMENT_3D('',#15714,#12692,#12693);
#11532=AXIS2_PLACEMENT_3D('',#15718,#12696,#12697);
#11533=AXIS2_PLACEMENT_3D('',#15722,#12700,#12701);
#11534=AXIS2_PLACEMENT_3D('',#15723,#12702,#12703);
#11535=AXIS2_PLACEMENT_3D('',#15727,#12706,#12707);
#11536=AXIS2_PLACEMENT_3D('',#15733,#12711,#12712);
#11537=AXIS2_PLACEMENT_3D('',#15739,#12716,#12717);
#11538=AXIS2_PLACEMENT_3D('',#15745,#12721,#12722);
#11539=AXIS2_PLACEMENT_3D('',#15747,#12724,#12725);
#11540=AXIS2_PLACEMENT_3D('',#15753,#12729,#12730);
#11541=AXIS2_PLACEMENT_3D('',#15755,#12732,#12733);
#11542=AXIS2_PLACEMENT_3D('',#15766,#12740,#12741);
#11543=AXIS2_PLACEMENT_3D('',#15769,#12744,#12745);
#11544=AXIS2_PLACEMENT_3D('',#15770,#12746,#12747);
#11545=AXIS2_PLACEMENT_3D('',#15771,#12748,#12749);
#11546=AXIS2_PLACEMENT_3D('',#15773,#12751,#12752);
#11547=AXIS2_PLACEMENT_3D('',#15775,#12754,#12755);
#11548=AXIS2_PLACEMENT_3D('',#15776,#12756,#12757);
#11549=AXIS2_PLACEMENT_3D('',#15778,#12758,#12759);
#11550=AXIS2_PLACEMENT_3D('',#15782,#12761,#12762);
#11551=AXIS2_PLACEMENT_3D('',#15783,#12763,#12764);
#11552=AXIS2_PLACEMENT_3D('',#15784,#12765,#12766);
#11553=AXIS2_PLACEMENT_3D('',#15791,#12767,#12768);
#11554=AXIS2_PLACEMENT_3D('',#15798,#12769,#12770);
#11555=AXIS2_PLACEMENT_3D('',#15800,#12771,#12772);
#11556=AXIS2_PLACEMENT_3D('',#15802,#12773,#12774);
#11557=AXIS2_PLACEMENT_3D('',#15811,#12775,#12776);
#11558=AXIS2_PLACEMENT_3D('',#15813,#12777,#12778);
#11559=AXIS2_PLACEMENT_3D('',#15815,#12779,#12780);
#11560=AXIS2_PLACEMENT_3D('',#15824,#12781,#12782);
#11561=AXIS2_PLACEMENT_3D('',#15826,#12783,#12784);
#11562=AXIS2_PLACEMENT_3D('',#15828,#12785,#12786);
#11563=AXIS2_PLACEMENT_3D('',#15837,#12787,#12788);
#11564=AXIS2_PLACEMENT_3D('',#15839,#12789,#12790);
#11565=AXIS2_PLACEMENT_3D('',#15840,#12791,#12792);
#11566=AXIS2_PLACEMENT_3D('',#15841,#12793,#12794);
#11567=AXIS2_PLACEMENT_3D('',#15845,#12797,#12798);
#11568=AXIS2_PLACEMENT_3D('',#15849,#12801,#12802);
#11569=AXIS2_PLACEMENT_3D('',#15853,#12805,#12806);
#11570=AXIS2_PLACEMENT_3D('',#15854,#12807,#12808);
#11571=AXIS2_PLACEMENT_3D('',#15858,#12811,#12812);
#11572=AXIS2_PLACEMENT_3D('',#15864,#12816,#12817);
#11573=AXIS2_PLACEMENT_3D('',#15870,#12821,#12822);
#11574=AXIS2_PLACEMENT_3D('',#15876,#12826,#12827);
#11575=AXIS2_PLACEMENT_3D('',#15878,#12829,#12830);
#11576=AXIS2_PLACEMENT_3D('',#15884,#12834,#12835);
#11577=AXIS2_PLACEMENT_3D('',#15886,#12837,#12838);
#11578=AXIS2_PLACEMENT_3D('',#15897,#12845,#12846);
#11579=AXIS2_PLACEMENT_3D('',#15900,#12849,#12850);
#11580=AXIS2_PLACEMENT_3D('',#15901,#12851,#12852);
#11581=AXIS2_PLACEMENT_3D('',#15902,#12853,#12854);
#11582=AXIS2_PLACEMENT_3D('',#15904,#12856,#12857);
#11583=AXIS2_PLACEMENT_3D('',#15906,#12859,#12860);
#11584=AXIS2_PLACEMENT_3D('',#15907,#12861,#12862);
#11585=AXIS2_PLACEMENT_3D('',#15937,#12864,#12865);
#11586=AXIS2_PLACEMENT_3D('',#15958,#12866,#12867);
#11587=AXIS2_PLACEMENT_3D('',#16036,#12869,#12870);
#11588=AXIS2_PLACEMENT_3D('',#16112,#12872,#12873);
#11589=AXIS2_PLACEMENT_3D('',#16188,#12875,#12876);
#11590=AXIS2_PLACEMENT_3D('',#16264,#12878,#12879);
#11591=AXIS2_PLACEMENT_3D('',#16340,#12881,#12882);
#11592=AXIS2_PLACEMENT_3D('',#16418,#12884,#12885);
#11593=AXIS2_PLACEMENT_3D('',#16496,#12887,#12888);
#11594=AXIS2_PLACEMENT_3D('',#16572,#12890,#12891);
#11595=AXIS2_PLACEMENT_3D('',#16648,#12893,#12894);
#11596=AXIS2_PLACEMENT_3D('',#16724,#12896,#12897);
#11597=AXIS2_PLACEMENT_3D('',#16800,#12899,#12900);
#11598=AXIS2_PLACEMENT_3D('',#16876,#12902,#12903);
#11599=AXIS2_PLACEMENT_3D('',#16954,#12905,#12906);
#11600=AXIS2_PLACEMENT_3D('',#17032,#12908,#12909);
#11601=AXIS2_PLACEMENT_3D('',#17108,#12911,#12912);
#11602=AXIS2_PLACEMENT_3D('',#17184,#12914,#12915);
#11603=AXIS2_PLACEMENT_3D('',#17260,#12917,#12918);
#11604=AXIS2_PLACEMENT_3D('',#17336,#12920,#12921);
#11605=AXIS2_PLACEMENT_3D('',#17358,#12923,#12924);
#11606=AXIS2_PLACEMENT_3D('',#17371,#12925,#12926);
#11607=AXIS2_PLACEMENT_3D('',#17449,#12928,#12929);
#11608=AXIS2_PLACEMENT_3D('',#17525,#12931,#12932);
#11609=AXIS2_PLACEMENT_3D('',#17601,#12934,#12935);
#11610=AXIS2_PLACEMENT_3D('',#17677,#12937,#12938);
#11611=AXIS2_PLACEMENT_3D('',#17753,#12940,#12941);
#11612=AXIS2_PLACEMENT_3D('',#17829,#12943,#12944);
#11613=AXIS2_PLACEMENT_3D('',#17909,#12946,#12947);
#11614=AXIS2_PLACEMENT_3D('',#17985,#12949,#12950);
#11615=AXIS2_PLACEMENT_3D('',#18061,#12952,#12953);
#11616=AXIS2_PLACEMENT_3D('',#18137,#12955,#12956);
#11617=AXIS2_PLACEMENT_3D('',#18213,#12958,#12959);
#11618=AXIS2_PLACEMENT_3D('',#18289,#12961,#12962);
#11619=AXIS2_PLACEMENT_3D('',#18367,#12964,#12965);
#11620=AXIS2_PLACEMENT_3D('',#18445,#12967,#12968);
#11621=AXIS2_PLACEMENT_3D('',#18521,#12970,#12971);
#11622=AXIS2_PLACEMENT_3D('',#18597,#12973,#12974);
#11623=AXIS2_PLACEMENT_3D('',#18673,#12976,#12977);
#11624=AXIS2_PLACEMENT_3D('',#18749,#12979,#12980);
#11625=AXIS2_PLACEMENT_3D('',#18762,#12982,#12983);
#11626=AXIS2_PLACEMENT_3D('',#18763,#12984,#12985);
#11627=AXIS2_PLACEMENT_3D('',#18841,#12987,#12988);
#11628=AXIS2_PLACEMENT_3D('',#18917,#12990,#12991);
#11629=AXIS2_PLACEMENT_3D('',#18993,#12993,#12994);
#11630=AXIS2_PLACEMENT_3D('',#19069,#12996,#12997);
#11631=AXIS2_PLACEMENT_3D('',#19145,#12999,#13000);
#11632=AXIS2_PLACEMENT_3D('',#19221,#13002,#13003);
#11633=AXIS2_PLACEMENT_3D('',#19299,#13005,#13006);
#11634=AXIS2_PLACEMENT_3D('',#19377,#13008,#13009);
#11635=AXIS2_PLACEMENT_3D('',#19453,#13011,#13012);
#11636=AXIS2_PLACEMENT_3D('',#19529,#13014,#13015);
#11637=AXIS2_PLACEMENT_3D('',#19605,#13017,#13018);
#11638=AXIS2_PLACEMENT_3D('',#19681,#13020,#13021);
#11639=AXIS2_PLACEMENT_3D('',#19759,#13023,#13024);
#11640=AXIS2_PLACEMENT_3D('',#19837,#13026,#13027);
#11641=AXIS2_PLACEMENT_3D('',#19913,#13029,#13030);
#11642=AXIS2_PLACEMENT_3D('',#19989,#13032,#13033);
#11643=AXIS2_PLACEMENT_3D('',#20065,#13035,#13036);
#11644=AXIS2_PLACEMENT_3D('',#20141,#13038,#13039);
#11645=AXIS2_PLACEMENT_3D('',#20181,#13041,#13042);
#11646=AXIS2_PLACEMENT_3D('',#20212,#13043,#13044);
#11647=AXIS2_PLACEMENT_3D('',#20288,#13046,#13047);
#11648=AXIS2_PLACEMENT_3D('',#20364,#13049,#13050);
#11649=AXIS2_PLACEMENT_3D('',#20440,#13052,#13053);
#11650=AXIS2_PLACEMENT_3D('',#20516,#13055,#13056);
#11651=AXIS2_PLACEMENT_3D('',#20592,#13058,#13059);
#11652=AXIS2_PLACEMENT_3D('',#20670,#13061,#13062);
#11653=AXIS2_PLACEMENT_3D('',#20748,#13064,#13065);
#11654=AXIS2_PLACEMENT_3D('',#20824,#13067,#13068);
#11655=AXIS2_PLACEMENT_3D('',#20900,#13070,#13071);
#11656=AXIS2_PLACEMENT_3D('',#20976,#13073,#13074);
#11657=AXIS2_PLACEMENT_3D('',#21052,#13076,#13077);
#11658=AXIS2_PLACEMENT_3D('',#21128,#13079,#13080);
#11659=AXIS2_PLACEMENT_3D('',#21208,#13082,#13083);
#11660=AXIS2_PLACEMENT_3D('',#21284,#13085,#13086);
#11661=AXIS2_PLACEMENT_3D('',#21360,#13088,#13089);
#11662=AXIS2_PLACEMENT_3D('',#21436,#13091,#13092);
#11663=AXIS2_PLACEMENT_3D('',#21512,#13094,#13095);
#11664=AXIS2_PLACEMENT_3D('',#21517,#13097,#13098);
#11665=AXIS2_PLACEMENT_3D('',#21532,#13099,#13100);
#11666=AXIS2_PLACEMENT_3D('',#21553,#13102,#13103);
#11667=AXIS2_PLACEMENT_3D('',#21592,#13104,#13105);
#11668=AXIS2_PLACEMENT_3D('',#21668,#13107,#13108);
#11669=AXIS2_PLACEMENT_3D('',#21744,#13110,#13111);
#11670=AXIS2_PLACEMENT_3D('',#21820,#13113,#13114);
#11671=AXIS2_PLACEMENT_3D('',#21898,#13116,#13117);
#11672=AXIS2_PLACEMENT_3D('',#21971,#13120,#13121);
#11673=AXIS2_PLACEMENT_3D('',#21976,#13123,#13124);
#11674=AXIS2_PLACEMENT_3D('',#21991,#13125,#13126);
#11675=AXIS2_PLACEMENT_3D('',#22012,#13128,#13129);
#11676=AXIS2_PLACEMENT_3D('',#22051,#13130,#13131);
#11677=AXIS2_PLACEMENT_3D('',#22127,#13133,#13134);
#11678=AXIS2_PLACEMENT_3D('',#22203,#13136,#13137);
#11679=AXIS2_PLACEMENT_3D('',#22279,#13139,#13140);
#11680=AXIS2_PLACEMENT_3D('',#22357,#13142,#13143);
#11681=AXIS2_PLACEMENT_3D('',#22430,#13146,#13147);
#11682=AXIS2_PLACEMENT_3D('',#22435,#13149,#13150);
#11683=AXIS2_PLACEMENT_3D('',#22450,#13151,#13152);
#11684=AXIS2_PLACEMENT_3D('',#22471,#13154,#13155);
#11685=AXIS2_PLACEMENT_3D('',#22510,#13156,#13157);
#11686=AXIS2_PLACEMENT_3D('',#22586,#13159,#13160);
#11687=AXIS2_PLACEMENT_3D('',#22662,#13162,#13163);
#11688=AXIS2_PLACEMENT_3D('',#22738,#13165,#13166);
#11689=AXIS2_PLACEMENT_3D('',#22816,#13168,#13169);
#11690=AXIS2_PLACEMENT_3D('',#22889,#13172,#13173);
#11691=AXIS2_PLACEMENT_3D('',#22894,#13175,#13176);
#11692=AXIS2_PLACEMENT_3D('',#22909,#13177,#13178);
#11693=AXIS2_PLACEMENT_3D('',#22930,#13180,#13181);
#11694=AXIS2_PLACEMENT_3D('',#22969,#13182,#13183);
#11695=AXIS2_PLACEMENT_3D('',#23045,#13185,#13186);
#11696=AXIS2_PLACEMENT_3D('',#23121,#13188,#13189);
#11697=AXIS2_PLACEMENT_3D('',#23197,#13191,#13192);
#11698=AXIS2_PLACEMENT_3D('',#23275,#13194,#13195);
#11699=AXIS2_PLACEMENT_3D('',#23348,#13198,#13199);
#11700=AXIS2_PLACEMENT_3D('',#23421,#13200,#13201);
#11701=AXIS2_PLACEMENT_3D('',#23494,#13202,#13203);
#11702=AXIS2_PLACEMENT_3D('',#23567,#13204,#13205);
#11703=AXIS2_PLACEMENT_3D('',#23640,#13206,#13207);
#11704=AXIS2_PLACEMENT_3D('',#23679,#13208,#13209);
#11705=AXIS2_PLACEMENT_3D('',#23712,#13210,#13211);
#11706=AXIS2_PLACEMENT_3D('',#23743,#13212,#13213);
#11707=AXIS2_PLACEMENT_3D('',#23768,#13214,#13215);
#11708=AXIS2_PLACEMENT_3D('',#23791,#13216,#13217);
#11709=AXIS2_PLACEMENT_3D('',#23808,#13218,#13219);
#11710=AXIS2_PLACEMENT_3D('',#23823,#13220,#13221);
#11711=AXIS2_PLACEMENT_3D('',#23832,#13222,#13223);
#11712=AXIS2_PLACEMENT_3D('',#23834,#13224,#13225);
#11713=AXIS2_PLACEMENT_3D('',#23837,#13227,#13228);
#11714=AXIS2_PLACEMENT_3D('',#23838,#13229,#13230);
#11715=AXIS2_PLACEMENT_3D('',#23840,#13231,#13232);
#11716=AXIS2_PLACEMENT_3D('',#23843,#13234,#13235);
#11717=AXIS2_PLACEMENT_3D('',#23844,#13236,#13237);
#11718=AXIS2_PLACEMENT_3D('',#23846,#13238,#13239);
#11719=AXIS2_PLACEMENT_3D('',#23849,#13241,#13242);
#11720=AXIS2_PLACEMENT_3D('',#23850,#13243,#13244);
#11721=AXIS2_PLACEMENT_3D('',#23853,#13246,#13247);
#11722=AXIS2_PLACEMENT_3D('',#23854,#13248,#13249);
#11723=AXIS2_PLACEMENT_3D('',#23898,#13250,#13251);
#11724=AXIS2_PLACEMENT_3D('',#23915,#13253,#13254);
#11725=AXIS2_PLACEMENT_3D('',#23916,#13255,#13256);
#11726=AXIS2_PLACEMENT_3D('',#23960,#13257,#13258);
#11727=AXIS2_PLACEMENT_3D('',#23977,#13260,#13261);
#11728=AXIS2_PLACEMENT_3D('',#23978,#13262,#13263);
#11729=AXIS2_PLACEMENT_3D('',#24022,#13264,#13265);
#11730=AXIS2_PLACEMENT_3D('',#24039,#13267,#13268);
#11731=AXIS2_PLACEMENT_3D('',#24040,#13269,#13270);
#11732=AXIS2_PLACEMENT_3D('',#24084,#13271,#13272);
#11733=AXIS2_PLACEMENT_3D('',#24101,#13274,#13275);
#11734=AXIS2_PLACEMENT_3D('',#24740,#13276,#13277);
#11735=AXIS2_PLACEMENT_3D('',#25682,#13279,#13280);
#11736=AXIS2_PLACEMENT_3D('',#25986,#13282,#13283);
#11737=AXIS2_PLACEMENT_3D('',#26630,#13285,#13286);
#11738=AXIS2_PLACEMENT_3D('',#26647,#13295,#13296);
#11739=AXIS2_PLACEMENT_3D('',#26648,#13297,#13298);
#11740=AXIS2_PLACEMENT_3D('',#26649,#13299,#13300);
#11741=AXIS2_PLACEMENT_3D('',#26650,#13301,#13302);
#11742=AXIS2_PLACEMENT_3D('',#26651,#13303,#13304);
#11743=AXIS2_PLACEMENT_3D('',#26652,#13305,#13306);
#11744=AXIS2_PLACEMENT_3D('',#28535,#13309,#13310);
#11745=AXIS2_PLACEMENT_3D('',#31061,#13314,#13315);
#11746=AXIS2_PLACEMENT_3D('',#33587,#13319,#13320);
#11747=AXIS2_PLACEMENT_3D('',#34231,#13322,#13323);
#11748=AXIS2_PLACEMENT_3D('',#34232,#13324,#13325);
#11749=AXIS2_PLACEMENT_3D('',#34233,#13326,#13327);
#11750=AXIS2_PLACEMENT_3D('',#34239,#13331,#13332);
#11751=AXIS2_PLACEMENT_3D('',#34243,#13335,#13336);
#11752=AXIS2_PLACEMENT_3D('',#34245,#13337,#13338);
#11753=AXIS2_PLACEMENT_3D('',#34248,#13340,#13341);
#11754=AXIS2_PLACEMENT_3D('',#34249,#13342,#13343);
#11755=AXIS2_PLACEMENT_3D('',#34253,#13346,#13347);
#11756=AXIS2_PLACEMENT_3D('',#34257,#13350,#13351);
#11757=AXIS2_PLACEMENT_3D('',#34259,#13352,#13353);
#11758=AXIS2_PLACEMENT_3D('',#34261,#13355,#13356);
#11759=AXIS2_PLACEMENT_3D('',#34265,#13359,#13360);
#11760=AXIS2_PLACEMENT_3D('',#34267,#13361,#13362);
#11761=AXIS2_PLACEMENT_3D('',#34269,#13364,#13365);
#11762=AXIS2_PLACEMENT_3D('',#34273,#13368,#13369);
#11763=AXIS2_PLACEMENT_3D('',#34275,#13370,#13371);
#11764=AXIS2_PLACEMENT_3D('',#34277,#13373,#13374);
#11765=AXIS2_PLACEMENT_3D('',#34281,#13377,#13378);
#11766=AXIS2_PLACEMENT_3D('',#34283,#13379,#13380);
#11767=AXIS2_PLACEMENT_3D('',#34285,#13382,#13383);
#11768=AXIS2_PLACEMENT_3D('',#34287,#13385,#13386);
#11769=AXIS2_PLACEMENT_3D('',#34289,#13387,#13388);
#11770=AXIS2_PLACEMENT_3D('',#34291,#13390,#13391);
#11771=AXIS2_PLACEMENT_3D('',#34293,#13392,#13393);
#11772=AXIS2_PLACEMENT_3D('',#34295,#13395,#13396);
#11773=AXIS2_PLACEMENT_3D('',#34297,#13398,#13399);
#11774=AXIS2_PLACEMENT_3D('',#34298,#13400,#13401);
#11775=AXIS2_PLACEMENT_3D('',#34303,#13403,#13404);
#11776=AXIS2_PLACEMENT_3D('',#34308,#13405,#13406);
#11777=AXIS2_PLACEMENT_3D('',#34309,#13407,#13408);
#11778=AXIS2_PLACEMENT_3D('',#34310,#13409,#13410);
#11779=AXIS2_PLACEMENT_3D('',#34315,#13411,#13412);
#11780=AXIS2_PLACEMENT_3D('',#34316,#13413,#13414);
#11781=AXIS2_PLACEMENT_3D('',#34320,#13416,#13417);
#11782=AXIS2_PLACEMENT_3D('',#34321,#13418,#13419);
#11783=AXIS2_PLACEMENT_3D('',#34323,#13420,#13421);
#11784=AXIS2_PLACEMENT_3D('',#34328,#13424,#13425);
#11785=AXIS2_PLACEMENT_3D('',#34330,#13427,#13428);
#11786=AXIS2_PLACEMENT_3D('',#34331,#13429,#13430);
#11787=AXIS2_PLACEMENT_3D('',#34332,#13431,#13432);
#11788=AXIS2_PLACEMENT_3D('',#34334,#13434,#13435);
#11789=AXIS2_PLACEMENT_3D('',#34335,#13436,#13437);
#11790=AXIS2_PLACEMENT_3D('',#34337,#13438,#13439);
#11791=AXIS2_PLACEMENT_3D('',#34340,#13441,#13442);
#11792=AXIS2_PLACEMENT_3D('',#34341,#13443,#13444);
#11793=AXIS2_PLACEMENT_3D('',#34343,#13445,#13446);
#11794=AXIS2_PLACEMENT_3D('',#34346,#13448,#13449);
#11795=AXIS2_PLACEMENT_3D('',#34347,#13450,#13451);
#11796=AXIS2_PLACEMENT_3D('',#34349,#13452,#13453);
#11797=AXIS2_PLACEMENT_3D('',#34352,#13455,#13456);
#11798=AXIS2_PLACEMENT_3D('',#34353,#13457,#13458);
#11799=AXIS2_PLACEMENT_3D('',#34355,#13459,#13460);
#11800=AXIS2_PLACEMENT_3D('',#34358,#13462,#13463);
#11801=AXIS2_PLACEMENT_3D('',#34359,#13464,#13465);
#11802=AXIS2_PLACEMENT_3D('',#34361,#13466,#13467);
#11803=AXIS2_PLACEMENT_3D('',#34364,#13469,#13470);
#11804=AXIS2_PLACEMENT_3D('',#34365,#13471,#13472);
#11805=AXIS2_PLACEMENT_3D('',#34367,#13473,#13474);
#11806=AXIS2_PLACEMENT_3D('',#34369,#13476,#13477);
#11807=AXIS2_PLACEMENT_3D('',#34371,#13478,#13479);
#11808=AXIS2_PLACEMENT_3D('',#34373,#13481,#13482);
#11809=AXIS2_PLACEMENT_3D('',#34375,#13483,#13484);
#11810=AXIS2_PLACEMENT_3D('',#34377,#13486,#13487);
#11811=AXIS2_PLACEMENT_3D('',#34379,#13488,#13489);
#11812=AXIS2_PLACEMENT_3D('',#34381,#13491,#13492);
#11813=AXIS2_PLACEMENT_3D('',#34383,#13493,#13494);
#11814=AXIS2_PLACEMENT_3D('',#34386,#13496,#13497);
#11815=AXIS2_PLACEMENT_3D('',#34387,#13498,#13499);
#11816=AXIS2_PLACEMENT_3D('',#34388,#13500,#13501);
#11817=AXIS2_PLACEMENT_3D('',#34389,#13502,#13503);
#11818=AXIS2_PLACEMENT_3D('',#34390,#13504,#13505);
#11819=AXIS2_PLACEMENT_3D('',#34391,#13506,#13507);
#11820=AXIS2_PLACEMENT_3D('',#34400,#13512,#13513);
#11821=AXIS2_PLACEMENT_3D('',#34406,#13517,#13518);
#11822=AXIS2_PLACEMENT_3D('',#34410,#13521,#13522);
#11823=AXIS2_PLACEMENT_3D('',#34414,#13525,#13526);
#11824=AXIS2_PLACEMENT_3D('',#34416,#13528,#13529);
#11825=AXIS2_PLACEMENT_3D('',#34425,#13534,#13535);
#11826=AXIS2_PLACEMENT_3D('',#34431,#13539,#13540);
#11827=AXIS2_PLACEMENT_3D('',#34448,#13549,#13550);
#11828=AXIS2_PLACEMENT_3D('',#34450,#13551,#13552);
#11829=AXIS2_PLACEMENT_3D('',#34452,#13553,#13554);
#11830=AXIS2_PLACEMENT_3D('',#34454,#13556,#13557);
#11831=AXIS2_PLACEMENT_3D('',#34456,#13558,#13559);
#11832=AXIS2_PLACEMENT_3D('',#34458,#13561,#13562);
#11833=AXIS2_PLACEMENT_3D('',#34460,#13563,#13564);
#11834=AXIS2_PLACEMENT_3D('',#34462,#13566,#13567);
#11835=AXIS2_PLACEMENT_3D('',#34468,#13571,#13572);
#11836=AXIS2_PLACEMENT_3D('',#34470,#13573,#13574);
#11837=AXIS2_PLACEMENT_3D('',#34472,#13576,#13577);
#11838=AXIS2_PLACEMENT_3D('',#34476,#13580,#13581);
#11839=AXIS2_PLACEMENT_3D('',#34478,#13582,#13583);
#11840=AXIS2_PLACEMENT_3D('',#34480,#13585,#13586);
#11841=AXIS2_PLACEMENT_3D('',#34484,#13589,#13590);
#11842=AXIS2_PLACEMENT_3D('',#34486,#13591,#13592);
#11843=AXIS2_PLACEMENT_3D('',#34488,#13594,#13595);
#11844=AXIS2_PLACEMENT_3D('',#34492,#13598,#13599);
#11845=AXIS2_PLACEMENT_3D('',#34494,#13600,#13601);
#11846=AXIS2_PLACEMENT_3D('',#34496,#13603,#13604);
#11847=AXIS2_PLACEMENT_3D('',#34500,#13607,#13608);
#11848=AXIS2_PLACEMENT_3D('',#34504,#13611,#13612);
#11849=AXIS2_PLACEMENT_3D('',#34506,#13613,#13614);
#11850=AXIS2_PLACEMENT_3D('',#34510,#13617,#13618);
#11851=AXIS2_PLACEMENT_3D('',#34514,#13621,#13622);
#11852=AXIS2_PLACEMENT_3D('',#34517,#13624,#13625);
#11853=AXIS2_PLACEMENT_3D('',#34518,#13626,#13627);
#11854=AXIS2_PLACEMENT_3D('',#34521,#13630,#13631);
#11855=AXIS2_PLACEMENT_3D('',#34525,#13634,#13635);
#11856=AXIS2_PLACEMENT_3D('',#34527,#13637,#13638);
#11857=AXIS2_PLACEMENT_3D('',#34528,#13639,#13640);
#11858=AXIS2_PLACEMENT_3D('',#34529,#13641,#13642);
#11859=AXIS2_PLACEMENT_3D('',#34531,#13643,#13644);
#11860=AXIS2_PLACEMENT_3D('',#34534,#13646,#13647);
#11861=AXIS2_PLACEMENT_3D('',#34535,#13648,#13649);
#11862=AXIS2_PLACEMENT_3D('',#34537,#13650,#13651);
#11863=AXIS2_PLACEMENT_3D('',#34540,#13653,#13654);
#11864=AXIS2_PLACEMENT_3D('',#34541,#13655,#13656);
#11865=AXIS2_PLACEMENT_3D('',#34543,#13657,#13658);
#11866=AXIS2_PLACEMENT_3D('',#34546,#13660,#13661);
#11867=AXIS2_PLACEMENT_3D('',#34547,#13662,#13663);
#11868=AXIS2_PLACEMENT_3D('',#34549,#13664,#13665);
#11869=AXIS2_PLACEMENT_3D('',#34552,#13667,#13668);
#11870=AXIS2_PLACEMENT_3D('',#34553,#13669,#13670);
#11871=AXIS2_PLACEMENT_3D('',#34555,#13671,#13672);
#11872=AXIS2_PLACEMENT_3D('',#34558,#13674,#13675);
#11873=AXIS2_PLACEMENT_3D('',#34559,#13676,#13677);
#11874=AXIS2_PLACEMENT_3D('',#34576,#13686,#13687);
#11875=AXIS2_PLACEMENT_3D('',#34593,#13696,#13697);
#11876=AXIS2_PLACEMENT_3D('',#34596,#13700,#13701);
#11877=AXIS2_PLACEMENT_3D('',#34598,#13703,#13704);
#11878=AXIS2_PLACEMENT_3D('',#34600,#13706,#13707);
#11879=AXIS2_PLACEMENT_3D('',#34603,#13710,#13711);
#11880=AXIS2_PLACEMENT_3D('',#34606,#13714,#13715);
#11881=AXIS2_PLACEMENT_3D('',#34607,#13716,#13717);
#11882=AXIS2_PLACEMENT_3D('',#34608,#13718,#13719);
#11883=AXIS2_PLACEMENT_3D('',#34609,#13720,#13721);
#11884=AXIS2_PLACEMENT_3D('',#34610,#13722,#13723);
#11885=AXIS2_PLACEMENT_3D('',#34611,#13724,#13725);
#11886=AXIS2_PLACEMENT_3D('',#34612,#13726,#13727);
#11887=AXIS2_PLACEMENT_3D('',#34613,#13728,#13729);
#11888=AXIS2_PLACEMENT_3D('',#34614,#13730,#13731);
#11889=AXIS2_PLACEMENT_3D('',#34615,#13732,#13733);
#11890=AXIS2_PLACEMENT_3D('',#34617,#13734,#13735);
#11891=AXIS2_PLACEMENT_3D('',#34620,#13737,#13738);
#11892=AXIS2_PLACEMENT_3D('',#34621,#13739,#13740);
#11893=AXIS2_PLACEMENT_3D('',#34623,#13741,#13742);
#11894=AXIS2_PLACEMENT_3D('',#34625,#13744,#13745);
#11895=AXIS2_PLACEMENT_3D('',#34627,#13746,#13747);
#11896=AXIS2_PLACEMENT_3D('',#34628,#13748,#13749);
#11897=AXIS2_PLACEMENT_3D('',#34631,#13751,#13752);
#11898=AXIS2_PLACEMENT_3D('',#34632,#13753,#13754);
#11899=AXIS2_PLACEMENT_3D('',#34634,#13755,#13756);
#11900=AXIS2_PLACEMENT_3D('',#34635,#13757,#13758);
#11901=AXIS2_PLACEMENT_3D('',#34637,#13760,#13761);
#11902=AXIS2_PLACEMENT_3D('',#34638,#13762,#13763);
#11903=AXIS2_PLACEMENT_3D('',#34640,#13764,#13765);
#11904=AXIS2_PLACEMENT_3D('',#34643,#13767,#13768);
#11905=AXIS2_PLACEMENT_3D('',#34644,#13769,#13770);
#11906=AXIS2_PLACEMENT_3D('',#34646,#13771,#13772);
#11907=AXIS2_PLACEMENT_3D('',#34649,#13774,#13775);
#11908=AXIS2_PLACEMENT_3D('',#34650,#13776,#13777);
#11909=AXIS2_PLACEMENT_3D('',#34651,#13778,#13779);
#11910=AXIS2_PLACEMENT_3D('',#34652,#13780,#13781);
#11911=AXIS2_PLACEMENT_3D('',#34653,#13782,#13783);
#11912=AXIS2_PLACEMENT_3D('',#34655,#13784,#13785);
#11913=AXIS2_PLACEMENT_3D('',#34658,#13787,#13788);
#11914=AXIS2_PLACEMENT_3D('',#34659,#13789,#13790);
#11915=AXIS2_PLACEMENT_3D('',#34661,#13791,#13792);
#11916=AXIS2_PLACEMENT_3D('',#34664,#13794,#13795);
#11917=AXIS2_PLACEMENT_3D('',#34665,#13796,#13797);
#11918=AXIS2_PLACEMENT_3D('',#34678,#13800,#13801);
#11919=AXIS2_PLACEMENT_3D('',#34688,#13803,#13804);
#11920=AXIS2_PLACEMENT_3D('',#34696,#13806,#13807);
#11921=AXIS2_PLACEMENT_3D('',#34711,#13808,#13809);
#11922=AXIS2_PLACEMENT_3D('',#34717,#13811,#13812);
#11923=AXIS2_PLACEMENT_3D('',#34727,#13814,#13815);
#11924=AXIS2_PLACEMENT_3D('',#34733,#13817,#13818);
#11925=AXIS2_PLACEMENT_3D('',#34737,#13819,#13820);
#11926=AXIS2_PLACEMENT_3D('',#34739,#13821,#13822);
#11927=AXIS2_PLACEMENT_3D('',#34740,#13823,#13824);
#11928=AXIS2_PLACEMENT_3D('',#34742,#13826,#13827);
#11929=AXIS2_PLACEMENT_3D('',#34743,#13828,#13829);
#11930=AXIS2_PLACEMENT_3D('',#34745,#13831,#13832);
#11931=AXIS2_PLACEMENT_3D('',#34746,#13833,#13834);
#11932=AXIS2_PLACEMENT_3D('',#34748,#13835,#13836);
#11933=AXIS2_PLACEMENT_3D('',#34751,#13838,#13839);
#11934=AXIS2_PLACEMENT_3D('',#34752,#13840,#13841);
#11935=AXIS2_PLACEMENT_3D('',#34754,#13842,#13843);
#11936=AXIS2_PLACEMENT_3D('',#34755,#13844,#13845);
#11937=AXIS2_PLACEMENT_3D('',#34756,#13846,#13847);
#11938=AXIS2_PLACEMENT_3D('',#34758,#13848,#13849);
#11939=AXIS2_PLACEMENT_3D('',#34760,#13851,#13852);
#11940=AXIS2_PLACEMENT_3D('',#34762,#13853,#13854);
#11941=AXIS2_PLACEMENT_3D('',#34765,#13856,#13857);
#11942=AXIS2_PLACEMENT_3D('',#34766,#13858,#13859);
#11943=AXIS2_PLACEMENT_3D('',#34769,#13860,#13861);
#11944=AXIS2_PLACEMENT_3D('',#34770,#13862,#13863);
#11945=AXIS2_PLACEMENT_3D('',#34772,#13865,#13866);
#11946=AXIS2_PLACEMENT_3D('',#34775,#13868,#13869);
#11947=AXIS2_PLACEMENT_3D('',#34776,#13870,#13871);
#11948=AXIS2_PLACEMENT_3D('',#34777,#13872,#13873);
#11949=AXIS2_PLACEMENT_3D('',#34778,#13874,#13875);
#11950=AXIS2_PLACEMENT_3D('',#34780,#13876,#13877);
#11951=AXIS2_PLACEMENT_3D('',#34783,#13879,#13880);
#11952=AXIS2_PLACEMENT_3D('',#34784,#13881,#13882);
#11953=AXIS2_PLACEMENT_3D('',#34786,#13883,#13884);
#11954=AXIS2_PLACEMENT_3D('',#34787,#13885,#13886);
#11955=AXIS2_PLACEMENT_3D('',#34788,#13887,#13888);
#11956=AXIS2_PLACEMENT_3D('',#34790,#13889,#13890);
#11957=AXIS2_PLACEMENT_3D('',#34793,#13892,#13893);
#11958=AXIS2_PLACEMENT_3D('',#34794,#13894,#13895);
#11959=AXIS2_PLACEMENT_3D('',#34797,#13897,#13898);
#11960=AXIS2_PLACEMENT_3D('',#34798,#13899,#13900);
#11961=AXIS2_PLACEMENT_3D('',#34799,#13901,#13902);
#11962=AXIS2_PLACEMENT_3D('',#34800,#13903,#13904);
#11963=AXIS2_PLACEMENT_3D('',#34802,#13905,#13906);
#11964=AXIS2_PLACEMENT_3D('',#34805,#13908,#13909);
#11965=AXIS2_PLACEMENT_3D('',#34806,#13910,#13911);
#11966=AXIS2_PLACEMENT_3D('',#34809,#13912,#13913);
#11967=AXIS2_PLACEMENT_3D('',#34810,#13914,#13915);
#11968=AXIS2_PLACEMENT_3D('',#34812,#13917,#13918);
#11969=AXIS2_PLACEMENT_3D('',#34815,#13920,#13921);
#11970=AXIS2_PLACEMENT_3D('',#34816,#13922,#13923);
#11971=AXIS2_PLACEMENT_3D('',#34818,#13924,#13925);
#11972=AXIS2_PLACEMENT_3D('',#34821,#13927,#13928);
#11973=AXIS2_PLACEMENT_3D('',#34822,#13929,#13930);
#11974=AXIS2_PLACEMENT_3D('',#34824,#13931,#13932);
#11975=AXIS2_PLACEMENT_3D('',#34825,#13933,#13934);
#11976=AXIS2_PLACEMENT_3D('',#34826,#13935,#13936);
#11977=AXIS2_PLACEMENT_3D('',#34828,#13937,#13938);
#11978=AXIS2_PLACEMENT_3D('',#34831,#13940,#13941);
#11979=AXIS2_PLACEMENT_3D('',#34832,#13942,#13943);
#11980=AXIS2_PLACEMENT_3D('',#34834,#13944,#13945);
#11981=AXIS2_PLACEMENT_3D('',#34836,#13947,#13948);
#11982=AXIS2_PLACEMENT_3D('',#34837,#13949,#13950);
#11983=AXIS2_PLACEMENT_3D('',#34838,#13951,#13952);
#11984=AXIS2_PLACEMENT_3D('',#34839,#13953,#13954);
#11985=AXIS2_PLACEMENT_3D('',#34842,#13955,#13956);
#11986=AXIS2_PLACEMENT_3D('',#34843,#13957,#13958);
#11987=AXIS2_PLACEMENT_3D('',#34846,#13959,#13960);
#11988=AXIS2_PLACEMENT_3D('',#34847,#13961,#13962);
#11989=AXIS2_PLACEMENT_3D('',#34850,#13963,#13964);
#11990=AXIS2_PLACEMENT_3D('',#34851,#13965,#13966);
#11991=AXIS2_PLACEMENT_3D('',#34854,#13967,#13968);
#11992=AXIS2_PLACEMENT_3D('',#34855,#13969,#13970);
#11993=AXIS2_PLACEMENT_3D('',#34858,#13971,#13972);
#11994=AXIS2_PLACEMENT_3D('',#34859,#13973,#13974);
#11995=AXIS2_PLACEMENT_3D('',#34862,#13975,#13976);
#11996=AXIS2_PLACEMENT_3D('',#34863,#13977,#13978);
#11997=AXIS2_PLACEMENT_3D('',#34866,#13979,#13980);
#11998=AXIS2_PLACEMENT_3D('',#34867,#13981,#13982);
#11999=AXIS2_PLACEMENT_3D('',#34870,#13983,#13984);
#12000=AXIS2_PLACEMENT_3D('',#34871,#13985,#13986);
#12001=AXIS2_PLACEMENT_3D('',#34874,#13987,#13988);
#12002=AXIS2_PLACEMENT_3D('',#34875,#13989,#13990);
#12003=AXIS2_PLACEMENT_3D('',#34878,#13991,#13992);
#12004=AXIS2_PLACEMENT_3D('',#34879,#13993,#13994);
#12005=AXIS2_PLACEMENT_3D('',#34880,#13995,#13996);
#12006=AXIS2_PLACEMENT_3D('',#34881,#13997,#13998);
#12007=AXIS2_PLACEMENT_3D('',#34882,#13999,#14000);
#12008=AXIS2_PLACEMENT_3D('',#34883,#14001,#14002);
#12009=AXIS2_PLACEMENT_3D('',#34884,#14003,#14004);
#12010=AXIS2_PLACEMENT_3D('',#34885,#14005,#14006);
#12011=AXIS2_PLACEMENT_3D('',#34894,#14011,#14012);
#12012=AXIS2_PLACEMENT_3D('',#34903,#14017,#14018);
#12013=AXIS2_PLACEMENT_3D('',#34912,#14023,#14024);
#12014=AXIS2_PLACEMENT_3D('',#34921,#14029,#14030);
#12015=AXIS2_PLACEMENT_3D('',#34930,#14035,#14036);
#12016=AXIS2_PLACEMENT_3D('',#34932,#14037,#14038);
#12017=AXIS2_PLACEMENT_3D('',#34935,#14040,#14041);
#12018=AXIS2_PLACEMENT_3D('',#34936,#14042,#14043);
#12019=AXIS2_PLACEMENT_3D('',#34945,#14048,#14049);
#12020=AXIS2_PLACEMENT_3D('',#34954,#14054,#14055);
#12021=AXIS2_PLACEMENT_3D('',#34957,#14058,#14059);
#12022=AXIS2_PLACEMENT_3D('',#34963,#14063,#14064);
#12023=AXIS2_PLACEMENT_3D('',#34969,#14068,#14069);
#12024=AXIS2_PLACEMENT_3D('',#34975,#14073,#14074);
#12025=AXIS2_PLACEMENT_3D('',#34981,#14078,#14079);
#12026=AXIS2_PLACEMENT_3D('',#34987,#14083,#14084);
#12027=AXIS2_PLACEMENT_3D('',#34993,#14088,#14089);
#12028=AXIS2_PLACEMENT_3D('',#34995,#14090,#14091);
#12029=AXIS2_PLACEMENT_3D('',#34998,#14093,#14094);
#12030=AXIS2_PLACEMENT_3D('',#34999,#14095,#14096);
#12031=AXIS2_PLACEMENT_3D('',#35005,#14100,#14101);
#12032=AXIS2_PLACEMENT_3D('',#35011,#14105,#14106);
#12033=AXIS2_PLACEMENT_3D('',#35017,#14110,#14111);
#12034=AXIS2_PLACEMENT_3D('',#35020,#14114,#14115);
#12035=AXIS2_PLACEMENT_3D('',#35029,#14120,#14121);
#12036=AXIS2_PLACEMENT_3D('',#35032,#14124,#14125);
#12037=AXIS2_PLACEMENT_3D('',#35035,#14128,#14129);
#12038=AXIS2_PLACEMENT_3D('',#35044,#14134,#14135);
#12039=AXIS2_PLACEMENT_3D('',#35050,#14139,#14140);
#12040=AXIS2_PLACEMENT_3D('',#35053,#14143,#14144);
#12041=AXIS2_PLACEMENT_3D('',#35062,#14149,#14150);
#12042=AXIS2_PLACEMENT_3D('',#35065,#14153,#14154);
#12043=AXIS2_PLACEMENT_3D('',#35071,#14158,#14159);
#12044=AXIS2_PLACEMENT_3D('',#35077,#14163,#14164);
#12045=AXIS2_PLACEMENT_3D('',#35083,#14168,#14169);
#12046=AXIS2_PLACEMENT_3D('',#35089,#14173,#14174);
#12047=AXIS2_PLACEMENT_3D('',#35095,#14178,#14179);
#12048=AXIS2_PLACEMENT_3D('',#35101,#14183,#14184);
#12049=AXIS2_PLACEMENT_3D('',#35103,#14185,#14186);
#12050=AXIS2_PLACEMENT_3D('',#35106,#14188,#14189);
#12051=AXIS2_PLACEMENT_3D('',#35107,#14190,#14191);
#12052=AXIS2_PLACEMENT_3D('',#35113,#14195,#14196);
#12053=AXIS2_PLACEMENT_3D('',#35119,#14200,#14201);
#12054=AXIS2_PLACEMENT_3D('',#35125,#14205,#14206);
#12055=AXIS2_PLACEMENT_3D('',#35128,#14209,#14210);
#12056=AXIS2_PLACEMENT_3D('',#35131,#14213,#14214);
#12057=AXIS2_PLACEMENT_3D('',#35137,#14218,#14219);
#12058=AXIS2_PLACEMENT_3D('',#35143,#14223,#14224);
#12059=AXIS2_PLACEMENT_3D('',#35149,#14228,#14229);
#12060=AXIS2_PLACEMENT_3D('',#35155,#14233,#14234);
#12061=AXIS2_PLACEMENT_3D('',#35161,#14238,#14239);
#12062=AXIS2_PLACEMENT_3D('',#35167,#14243,#14244);
#12063=AXIS2_PLACEMENT_3D('',#35173,#14248,#14249);
#12064=AXIS2_PLACEMENT_3D('',#35203,#14264,#14265);
#12065=AXIS2_PLACEMENT_3D('',#35231,#14279,#14280);
#12066=AXIS2_PLACEMENT_3D('',#35265,#14298,#14299);
#12067=AXIS2_PLACEMENT_3D('',#35266,#14300,#14301);
#12068=AXIS2_PLACEMENT_3D('',#35270,#14304,#14305);
#12069=AXIS2_PLACEMENT_3D('',#35274,#14308,#14309);
#12070=AXIS2_PLACEMENT_3D('',#35280,#14313,#14314);
#12071=AXIS2_PLACEMENT_3D('',#35286,#14318,#14319);
#12072=AXIS2_PLACEMENT_3D('',#35292,#14323,#14324);
#12073=AXIS2_PLACEMENT_3D('',#35295,#14326,#14327);
#12074=AXIS2_PLACEMENT_3D('',#35296,#14328,#14329);
#12075=AXIS2_PLACEMENT_3D('',#35302,#14333,#14334);
#12076=AXIS2_PLACEMENT_3D('',#35308,#14338,#14339);
#12077=AXIS2_PLACEMENT_3D('',#35310,#14341,#14342);
#12078=AXIS2_PLACEMENT_3D('',#35314,#14345,#14346);
#12079=AXIS2_PLACEMENT_3D('',#35318,#14349,#14350);
#12080=AXIS2_PLACEMENT_3D('',#35322,#14353,#14354);
#12081=AXIS2_PLACEMENT_3D('',#35326,#14357,#14358);
#12082=AXIS2_PLACEMENT_3D('',#35330,#14361,#14362);
#12083=AXIS2_PLACEMENT_3D('',#35334,#14365,#14366);
#12084=AXIS2_PLACEMENT_3D('',#35336,#14367,#14368);
#12085=AXIS2_PLACEMENT_3D('',#35338,#14370,#14371);
#12086=AXIS2_PLACEMENT_3D('',#35342,#14374,#14375);
#12087=AXIS2_PLACEMENT_3D('',#35346,#14378,#14379);
#12088=AXIS2_PLACEMENT_3D('',#35350,#14382,#14383);
#12089=AXIS2_PLACEMENT_3D('',#35352,#14385,#14386);
#12090=AXIS2_PLACEMENT_3D('',#35358,#14390,#14391);
#12091=AXIS2_PLACEMENT_3D('',#35360,#14393,#14394);
#12092=AXIS2_PLACEMENT_3D('',#35362,#14396,#14397);
#12093=AXIS2_PLACEMENT_3D('',#35366,#14400,#14401);
#12094=AXIS2_PLACEMENT_3D('',#35370,#14404,#14405);
#12095=AXIS2_PLACEMENT_3D('',#35374,#14408,#14409);
#12096=AXIS2_PLACEMENT_3D('',#35376,#14411,#14412);
#12097=AXIS2_PLACEMENT_3D('',#35382,#14416,#14417);
#12098=AXIS2_PLACEMENT_3D('',#35384,#14419,#14420);
#12099=AXIS2_PLACEMENT_3D('',#35388,#14423,#14424);
#12100=AXIS2_PLACEMENT_3D('',#35392,#14427,#14428);
#12101=AXIS2_PLACEMENT_3D('',#35396,#14431,#14432);
#12102=AXIS2_PLACEMENT_3D('',#35400,#14435,#14436);
#12103=AXIS2_PLACEMENT_3D('',#35404,#14439,#14440);
#12104=AXIS2_PLACEMENT_3D('',#35408,#14443,#14444);
#12105=AXIS2_PLACEMENT_3D('',#35410,#14445,#14446);
#12106=AXIS2_PLACEMENT_3D('',#35412,#14448,#14449);
#12107=AXIS2_PLACEMENT_3D('',#35416,#14452,#14453);
#12108=AXIS2_PLACEMENT_3D('',#35420,#14456,#14457);
#12109=AXIS2_PLACEMENT_3D('',#35424,#14460,#14461);
#12110=AXIS2_PLACEMENT_3D('',#35426,#14463,#14464);
#12111=AXIS2_PLACEMENT_3D('',#35428,#14466,#14467);
#12112=AXIS2_PLACEMENT_3D('',#35432,#14470,#14471);
#12113=AXIS2_PLACEMENT_3D('',#35436,#14474,#14475);
#12114=AXIS2_PLACEMENT_3D('',#35440,#14478,#14479);
#12115=AXIS2_PLACEMENT_3D('',#35444,#14482,#14483);
#12116=AXIS2_PLACEMENT_3D('',#35448,#14486,#14487);
#12117=AXIS2_PLACEMENT_3D('',#35450,#14489,#14490);
#12118=AXIS2_PLACEMENT_3D('',#35451,#14491,#14492);
#12119=AXIS2_PLACEMENT_3D('',#35452,#14493,#14494);
#12120=AXIS2_PLACEMENT_3D('',#35454,#14495,#14496);
#12121=AXIS2_PLACEMENT_3D('',#35456,#14497,#14498);
#12122=AXIS2_PLACEMENT_3D('',#35457,#14499,#14500);
#12123=AXIS2_PLACEMENT_3D('',#35459,#14501,#14502);
#12124=AXIS2_PLACEMENT_3D('',#35462,#14504,#14505);
#12125=AXIS2_PLACEMENT_3D('',#35463,#14506,#14507);
#12126=AXIS2_PLACEMENT_3D('',#35465,#14508,#14509);
#12127=AXIS2_PLACEMENT_3D('',#35466,#14510,#14511);
#12128=AXIS2_PLACEMENT_3D('',#35468,#14512,#14513);
#12129=AXIS2_PLACEMENT_3D('',#35469,#14514,#14515);
#12130=AXIS2_PLACEMENT_3D('',#35472,#14517,#14518);
#12131=AXIS2_PLACEMENT_3D('',#35473,#14519,#14520);
#12132=AXIS2_PLACEMENT_3D('',#35475,#14522,#14523);
#12133=AXIS2_PLACEMENT_3D('',#35477,#14524,#14525);
#12134=AXIS2_PLACEMENT_3D('',#35478,#14526,#14527);
#12135=AXIS2_PLACEMENT_3D('',#35480,#14529,#14530);
#12136=AXIS2_PLACEMENT_3D('',#35481,#14531,#14532);
#12137=AXIS2_PLACEMENT_3D('',#35483,#14533,#14534);
#12138=AXIS2_PLACEMENT_3D('',#35486,#14536,#14537);
#12139=AXIS2_PLACEMENT_3D('',#35487,#14538,#14539);
#12140=AXIS2_PLACEMENT_3D('',#35496,#14544,#14545);
#12141=AXIS2_PLACEMENT_3D('',#35502,#14549,#14550);
#12142=AXIS2_PLACEMENT_3D('',#35508,#14554,#14555);
#12143=AXIS2_PLACEMENT_3D('',#35511,#14558,#14559);
#12144=AXIS2_PLACEMENT_3D('',#35520,#14564,#14565);
#12145=AXIS2_PLACEMENT_3D('',#35526,#14569,#14570);
#12146=AXIS2_PLACEMENT_3D('',#35532,#14574,#14575);
#12147=AXIS2_PLACEMENT_3D('',#35535,#14578,#14579);
#12148=AXIS2_PLACEMENT_3D('',#35537,#14580,#14581);
#12149=AXIS2_PLACEMENT_3D('',#35540,#14583,#14584);
#12150=AXIS2_PLACEMENT_3D('',#35541,#14585,#14586);
#12151=AXIS2_PLACEMENT_3D('',#35543,#14587,#14588);
#12152=AXIS2_PLACEMENT_3D('',#35546,#14590,#14591);
#12153=AXIS2_PLACEMENT_3D('',#35547,#14592,#14593);
#12154=AXIS2_PLACEMENT_3D('',#35556,#14598,#14599);
#12155=AXIS2_PLACEMENT_3D('',#35562,#14603,#14604);
#12156=AXIS2_PLACEMENT_3D('',#35568,#14608,#14609);
#12157=AXIS2_PLACEMENT_3D('',#35571,#14612,#14613);
#12158=AXIS2_PLACEMENT_3D('',#35573,#14614,#14615);
#12159=AXIS2_PLACEMENT_3D('',#35576,#14617,#14618);
#12160=AXIS2_PLACEMENT_3D('',#35577,#14619,#14620);
#12161=AXIS2_PLACEMENT_3D('',#35579,#14621,#14622);
#12162=AXIS2_PLACEMENT_3D('',#35582,#14624,#14625);
#12163=AXIS2_PLACEMENT_3D('',#35583,#14626,#14627);
#12164=AXIS2_PLACEMENT_3D('',#35592,#14632,#14633);
#12165=AXIS2_PLACEMENT_3D('',#35598,#14637,#14638);
#12166=AXIS2_PLACEMENT_3D('',#35604,#14642,#14643);
#12167=AXIS2_PLACEMENT_3D('',#35610,#14647,#14648);
#12168=AXIS2_PLACEMENT_3D('',#35616,#14652,#14653);
#12169=AXIS2_PLACEMENT_3D('',#35622,#14657,#14658);
#12170=AXIS2_PLACEMENT_3D('',#35628,#14662,#14663);
#12171=AXIS2_PLACEMENT_3D('',#35634,#14667,#14668);
#12172=AXIS2_PLACEMENT_3D('',#35640,#14672,#14673);
#12173=AXIS2_PLACEMENT_3D('',#35642,#14674,#14675);
#12174=AXIS2_PLACEMENT_3D('',#35644,#14676,#14677);
#12175=AXIS2_PLACEMENT_3D('',#35646,#14679,#14680);
#12176=AXIS2_PLACEMENT_3D('',#35652,#14684,#14685);
#12177=AXIS2_PLACEMENT_3D('',#35654,#14686,#14687);
#12178=AXIS2_PLACEMENT_3D('',#35656,#14688,#14689);
#12179=AXIS2_PLACEMENT_3D('',#35658,#14691,#14692);
#12180=AXIS2_PLACEMENT_3D('',#35664,#14696,#14697);
#12181=AXIS2_PLACEMENT_3D('',#35666,#14698,#14699);
#12182=AXIS2_PLACEMENT_3D('',#35668,#14700,#14701);
#12183=AXIS2_PLACEMENT_3D('',#35670,#14703,#14704);
#12184=AXIS2_PLACEMENT_3D('',#35676,#14708,#14709);
#12185=AXIS2_PLACEMENT_3D('',#35677,#14710,#14711);
#12186=AXIS2_PLACEMENT_3D('',#35678,#14712,#14713);
#12187=AXIS2_PLACEMENT_3D('',#35679,#14714,#14715);
#12188=AXIS2_PLACEMENT_3D('',#35680,#14716,#14717);
#12189=AXIS2_PLACEMENT_3D('',#35681,#14718,#14719);
#12190=AXIS2_PLACEMENT_3D('',#35682,#14720,#14721);
#12191=AXIS2_PLACEMENT_3D('',#35754,#14723,#14724);
#12192=AXIS2_PLACEMENT_3D('',#35838,#14726,#14727);
#12193=AXIS2_PLACEMENT_3D('',#35840,#14728,#14729);
#12194=AXIS2_PLACEMENT_3D('',#35844,#14732,#14733);
#12195=AXIS2_PLACEMENT_3D('',#35845,#14734,#14735);
#12196=AXIS2_PLACEMENT_3D('',#35847,#14736,#14737);
#12197=AXIS2_PLACEMENT_3D('',#35848,#14738,#14739);
#12198=AXIS2_PLACEMENT_3D('',#35850,#14740,#14741);
#12199=AXIS2_PLACEMENT_3D('',#35852,#14742,#14743);
#12200=AXIS2_PLACEMENT_3D('',#35853,#14744,#14745);
#12201=AXIS2_PLACEMENT_3D('',#35855,#14746,#14747);
#12202=AXIS2_PLACEMENT_3D('',#35857,#14749,#14750);
#12203=AXIS2_PLACEMENT_3D('',#35858,#14751,#14752);
#12204=AXIS2_PLACEMENT_3D('',#35861,#14754,#14755);
#12205=AXIS2_PLACEMENT_3D('',#35862,#14756,#14757);
#12206=AXIS2_PLACEMENT_3D('',#35864,#14758,#14759);
#12207=AXIS2_PLACEMENT_3D('',#35867,#14762,#14763);
#12208=AXIS2_PLACEMENT_3D('',#35869,#14764,#14765);
#12209=AXIS2_PLACEMENT_3D('',#35872,#14767,#14768);
#12210=AXIS2_PLACEMENT_3D('',#35873,#14769,#14770);
#12211=AXIS2_PLACEMENT_3D('',#35874,#14771,#14772);
#12212=AXIS2_PLACEMENT_3D('',#35875,#14773,#14774);
#12213=AXIS2_PLACEMENT_3D('',#35876,#14775,#14776);
#12214=AXIS2_PLACEMENT_3D('',#35879,#14777,#14778);
#12215=AXIS2_PLACEMENT_3D('',#35883,#14780,#14781);
#12216=AXIS2_PLACEMENT_3D('',#35887,#14783,#14784);
#12217=AXIS2_PLACEMENT_3D('',#35891,#14786,#14787);
#12218=AXIS2_PLACEMENT_3D('',#35893,#14789,#14790);
#12219=AXIS2_PLACEMENT_3D('',#35899,#14794,#14795);
#12220=AXIS2_PLACEMENT_3D('',#35901,#14796,#14797);
#12221=AXIS2_PLACEMENT_3D('',#35903,#14799,#14800);
#12222=AXIS2_PLACEMENT_3D('',#35907,#14803,#14804);
#12223=AXIS2_PLACEMENT_3D('',#35908,#14805,#14806);
#12224=AXIS2_PLACEMENT_3D('',#35909,#14807,#14808);
#12225=AXIS2_PLACEMENT_3D('',#35915,#14812,#14813);
#12226=AXIS2_PLACEMENT_3D('',#35917,#14814,#14815);
#12227=AXIS2_PLACEMENT_3D('',#35919,#14817,#14818);
#12228=AXIS2_PLACEMENT_3D('',#35923,#14821,#14822);
#12229=AXIS2_PLACEMENT_3D('',#35924,#14823,#14824);
#12230=AXIS2_PLACEMENT_3D('',#35925,#14825,#14826);
#12231=AXIS2_PLACEMENT_3D('',#35926,#14827,#14828);
#12232=AXIS2_PLACEMENT_3D('',#35927,#14829,#14830);
#12233=AXIS2_PLACEMENT_3D('',#35929,#14831,#14832);
#12234=AXIS2_PLACEMENT_3D('',#35932,#14834,#14835);
#12235=AXIS2_PLACEMENT_3D('',#35933,#14836,#14837);
#12236=AXIS2_PLACEMENT_3D('',#35942,#14842,#14843);
#12237=AXIS2_PLACEMENT_3D('',#35944,#14844,#14845);
#12238=AXIS2_PLACEMENT_3D('',#35946,#14846,#14847);
#12239=AXIS2_PLACEMENT_3D('',#35948,#14849,#14850);
#12240=AXIS2_PLACEMENT_3D('',#35954,#14854,#14855);
#12241=AXIS2_PLACEMENT_3D('',#35955,#14856,#14857);
#12242=AXIS2_PLACEMENT_3D('',#35956,#14858,#14859);
#12243=AXIS2_PLACEMENT_3D('',#35957,#14860,#14861);
#12244=AXIS2_PLACEMENT_3D('',#35959,#14862,#14863);
#12245=AXIS2_PLACEMENT_3D('',#35962,#14865,#14866);
#12246=AXIS2_PLACEMENT_3D('',#35963,#14867,#14868);
#12247=AXIS2_PLACEMENT_3D('',#35965,#14869,#14870);
#12248=AXIS2_PLACEMENT_3D('',#35968,#14872,#14873);
#12249=AXIS2_PLACEMENT_3D('',#35969,#14874,#14875);
#12250=AXIS2_PLACEMENT_3D('',#35971,#14876,#14877);
#12251=AXIS2_PLACEMENT_3D('',#35974,#14879,#14880);
#12252=AXIS2_PLACEMENT_3D('',#35975,#14881,#14882);
#12253=AXIS2_PLACEMENT_3D('',#35977,#14883,#14884);
#12254=AXIS2_PLACEMENT_3D('',#35980,#14886,#14887);
#12255=AXIS2_PLACEMENT_3D('',#35981,#14888,#14889);
#12256=AXIS2_PLACEMENT_3D('',#35983,#14890,#14891);
#12257=AXIS2_PLACEMENT_3D('',#35986,#14893,#14894);
#12258=AXIS2_PLACEMENT_3D('',#35987,#14895,#14896);
#12259=AXIS2_PLACEMENT_3D('',#35996,#14901,#14902);
#12260=AXIS2_PLACEMENT_3D('',#35998,#14903,#14904);
#12261=AXIS2_PLACEMENT_3D('',#36000,#14905,#14906);
#12262=AXIS2_PLACEMENT_3D('',#36002,#14908,#14909);
#12263=AXIS2_PLACEMENT_3D('',#36008,#14913,#14914);
#12264=AXIS2_PLACEMENT_3D('',#36009,#14915,#14916);
#12265=AXIS2_PLACEMENT_3D('',#36010,#14917,#14918);
#12266=AXIS2_PLACEMENT_3D('',#36011,#14919,#14920);
#12267=AXIS2_PLACEMENT_3D('',#36020,#14925,#14926);
#12268=AXIS2_PLACEMENT_3D('',#36022,#14927,#14928);
#12269=AXIS2_PLACEMENT_3D('',#36024,#14929,#14930);
#12270=AXIS2_PLACEMENT_3D('',#36026,#14932,#14933);
#12271=AXIS2_PLACEMENT_3D('',#36032,#14937,#14938);
#12272=AXIS2_PLACEMENT_3D('',#36033,#14939,#14940);
#12273=AXIS2_PLACEMENT_3D('',#36034,#14941,#14942);
#12274=AXIS2_PLACEMENT_3D('',#36035,#14943,#14944);
#12275=AXIS2_PLACEMENT_3D('',#36037,#14945,#14946);
#12276=AXIS2_PLACEMENT_3D('',#36040,#14948,#14949);
#12277=AXIS2_PLACEMENT_3D('',#36041,#14950,#14951);
#12278=AXIS2_PLACEMENT_3D('',#36043,#14952,#14953);
#12279=AXIS2_PLACEMENT_3D('',#36046,#14955,#14956);
#12280=AXIS2_PLACEMENT_3D('',#36047,#14957,#14958);
#12281=AXIS2_PLACEMENT_3D('',#36049,#14959,#14960);
#12282=AXIS2_PLACEMENT_3D('',#36052,#14962,#14963);
#12283=AXIS2_PLACEMENT_3D('',#36053,#14964,#14965);
#12284=AXIS2_PLACEMENT_3D('',#36055,#14966,#14967);
#12285=AXIS2_PLACEMENT_3D('',#36058,#14969,#14970);
#12286=AXIS2_PLACEMENT_3D('',#36059,#14971,#14972);
#12287=AXIS2_PLACEMENT_3D('',#36061,#14973,#14974);
#12288=AXIS2_PLACEMENT_3D('',#36064,#14976,#14977);
#12289=AXIS2_PLACEMENT_3D('',#36065,#14978,#14979);
#12290=AXIS2_PLACEMENT_3D('',#36074,#14984,#14985);
#12291=AXIS2_PLACEMENT_3D('',#36076,#14986,#14987);
#12292=AXIS2_PLACEMENT_3D('',#36078,#14988,#14989);
#12293=AXIS2_PLACEMENT_3D('',#36080,#14991,#14992);
#12294=AXIS2_PLACEMENT_3D('',#36086,#14996,#14997);
#12295=AXIS2_PLACEMENT_3D('',#36087,#14998,#14999);
#12296=AXIS2_PLACEMENT_3D('',#36088,#15000,#15001);
#12297=AXIS2_PLACEMENT_3D('',#36089,#15002,#15003);
#12298=AXIS2_PLACEMENT_3D('',#36091,#15004,#15005);
#12299=AXIS2_PLACEMENT_3D('',#36094,#15007,#15008);
#12300=AXIS2_PLACEMENT_3D('',#36095,#15009,#15010);
#12301=AXIS2_PLACEMENT_3D('',#36097,#15011,#15012);
#12302=AXIS2_PLACEMENT_3D('',#36100,#15014,#15015);
#12303=AXIS2_PLACEMENT_3D('',#36101,#15016,#15017);
#12304=AXIS2_PLACEMENT_3D('',#36110,#15022,#15023);
#12305=AXIS2_PLACEMENT_3D('',#36112,#15024,#15025);
#12306=AXIS2_PLACEMENT_3D('',#36114,#15026,#15027);
#12307=AXIS2_PLACEMENT_3D('',#36116,#15029,#15030);
#12308=AXIS2_PLACEMENT_3D('',#36122,#15034,#15035);
#12309=AXIS2_PLACEMENT_3D('',#36123,#15036,#15037);
#12310=AXIS2_PLACEMENT_3D('',#36124,#15038,#15039);
#12311=AXIS2_PLACEMENT_3D('',#36125,#15040,#15041);
#12312=AXIS2_PLACEMENT_3D('',#36134,#15046,#15047);
#12313=AXIS2_PLACEMENT_3D('',#36136,#15048,#15049);
#12314=AXIS2_PLACEMENT_3D('',#36138,#15050,#15051);
#12315=AXIS2_PLACEMENT_3D('',#36140,#15053,#15054);
#12316=AXIS2_PLACEMENT_3D('',#36146,#15058,#15059);
#12317=AXIS2_PLACEMENT_3D('',#36147,#15060,#15061);
#12318=AXIS2_PLACEMENT_3D('',#36148,#15062,#15063);
#12319=AXIS2_PLACEMENT_3D('',#36149,#15064,#15065);
#12320=AXIS2_PLACEMENT_3D('',#36158,#15070,#15071);
#12321=AXIS2_PLACEMENT_3D('',#36160,#15072,#15073);
#12322=AXIS2_PLACEMENT_3D('',#36162,#15074,#15075);
#12323=AXIS2_PLACEMENT_3D('',#36164,#15077,#15078);
#12324=AXIS2_PLACEMENT_3D('',#36170,#15082,#15083);
#12325=AXIS2_PLACEMENT_3D('',#36171,#15084,#15085);
#12326=AXIS2_PLACEMENT_3D('',#36172,#15086,#15087);
#12327=AXIS2_PLACEMENT_3D('',#36173,#15088,#15089);
#12328=AXIS2_PLACEMENT_3D('',#36182,#15094,#15095);
#12329=AXIS2_PLACEMENT_3D('',#36184,#15096,#15097);
#12330=AXIS2_PLACEMENT_3D('',#36186,#15098,#15099);
#12331=AXIS2_PLACEMENT_3D('',#36188,#15101,#15102);
#12332=AXIS2_PLACEMENT_3D('',#36194,#15106,#15107);
#12333=AXIS2_PLACEMENT_3D('',#36195,#15108,#15109);
#12334=AXIS2_PLACEMENT_3D('',#36196,#15110,#15111);
#12335=AXIS2_PLACEMENT_3D('',#36197,#15112,#15113);
#12336=AXIS2_PLACEMENT_3D('',#36199,#15114,#15115);
#12337=AXIS2_PLACEMENT_3D('',#36202,#15117,#15118);
#12338=AXIS2_PLACEMENT_3D('',#36203,#15119,#15120);
#12339=AXIS2_PLACEMENT_3D('',#36205,#15121,#15122);
#12340=AXIS2_PLACEMENT_3D('',#36208,#15124,#15125);
#12341=AXIS2_PLACEMENT_3D('',#36209,#15126,#15127);
#12342=AXIS2_PLACEMENT_3D('',#36218,#15132,#15133);
#12343=AXIS2_PLACEMENT_3D('',#36220,#15134,#15135);
#12344=AXIS2_PLACEMENT_3D('',#36222,#15136,#15137);
#12345=AXIS2_PLACEMENT_3D('',#36224,#15139,#15140);
#12346=AXIS2_PLACEMENT_3D('',#36230,#15144,#15145);
#12347=AXIS2_PLACEMENT_3D('',#36232,#15146,#15147);
#12348=AXIS2_PLACEMENT_3D('',#36234,#15148,#15149);
#12349=AXIS2_PLACEMENT_3D('',#36236,#15151,#15152);
#12350=AXIS2_PLACEMENT_3D('',#36242,#15156,#15157);
#12351=AXIS2_PLACEMENT_3D('',#36244,#15158,#15159);
#12352=AXIS2_PLACEMENT_3D('',#36246,#15160,#15161);
#12353=AXIS2_PLACEMENT_3D('',#36248,#15163,#15164);
#12354=AXIS2_PLACEMENT_3D('',#36254,#15168,#15169);
#12355=AXIS2_PLACEMENT_3D('',#36255,#15170,#15171);
#12356=AXIS2_PLACEMENT_3D('',#36256,#15172,#15173);
#12357=AXIS2_PLACEMENT_3D('',#36257,#15174,#15175);
#12358=AXIS2_PLACEMENT_3D('',#36258,#15176,#15177);
#12359=AXIS2_PLACEMENT_3D('',#36259,#15178,#15179);
#12360=AXIS2_PLACEMENT_3D('',#36260,#15180,#15181);
#12361=AXIS2_PLACEMENT_3D('',#36262,#15182,#15183);
#12362=AXIS2_PLACEMENT_3D('',#36265,#15185,#15186);
#12363=AXIS2_PLACEMENT_3D('',#36266,#15187,#15188);
#12364=AXIS2_PLACEMENT_3D('',#36268,#15189,#15190);
#12365=AXIS2_PLACEMENT_3D('',#36271,#15192,#15193);
#12366=AXIS2_PLACEMENT_3D('',#36272,#15194,#15195);
#12367=AXIS2_PLACEMENT_3D('',#36274,#15196,#15197);
#12368=AXIS2_PLACEMENT_3D('',#36277,#15199,#15200);
#12369=AXIS2_PLACEMENT_3D('',#36278,#15201,#15202);
#12370=AXIS2_PLACEMENT_3D('',#36280,#15203,#15204);
#12371=AXIS2_PLACEMENT_3D('',#36283,#15206,#15207);
#12372=AXIS2_PLACEMENT_3D('',#36284,#15208,#15209);
#12373=AXIS2_PLACEMENT_3D('',#36286,#15210,#15211);
#12374=AXIS2_PLACEMENT_3D('',#36289,#15213,#15214);
#12375=AXIS2_PLACEMENT_3D('',#36290,#15215,#15216);
#12376=AXIS2_PLACEMENT_3D('',#36293,#15217,#15218);
#12377=AXIS2_PLACEMENT_3D('',#36297,#15220,#15221);
#12378=AXIS2_PLACEMENT_3D('',#36299,#15223,#15224);
#12379=AXIS2_PLACEMENT_3D('',#36305,#15228,#15229);
#12380=AXIS2_PLACEMENT_3D('',#36307,#15230,#15231);
#12381=AXIS2_PLACEMENT_3D('',#36309,#15232,#15233);
#12382=AXIS2_PLACEMENT_3D('',#36311,#15235,#15236);
#12383=AXIS2_PLACEMENT_3D('',#36317,#15240,#15241);
#12384=AXIS2_PLACEMENT_3D('',#36319,#15242,#15243);
#12385=AXIS2_PLACEMENT_3D('',#36321,#15244,#15245);
#12386=AXIS2_PLACEMENT_3D('',#36323,#15247,#15248);
#12387=AXIS2_PLACEMENT_3D('',#36329,#15252,#15253);
#12388=AXIS2_PLACEMENT_3D('',#36331,#15254,#15255);
#12389=AXIS2_PLACEMENT_3D('',#36333,#15256,#15257);
#12390=AXIS2_PLACEMENT_3D('',#36335,#15259,#15260);
#12391=AXIS2_PLACEMENT_3D('',#36338,#15263,#15264);
#12392=AXIS2_PLACEMENT_3D('',#36339,#15265,#15266);
#12393=AXIS2_PLACEMENT_3D('',#36340,#15267,#15268);
#12394=AXIS2_PLACEMENT_3D('',#36341,#15269,#15270);
#12395=AXIS2_PLACEMENT_3D('',#36343,#15271,#15272);
#12396=AXIS2_PLACEMENT_3D('',#36346,#15274,#15275);
#12397=AXIS2_PLACEMENT_3D('',#36347,#15276,#15277);
#12398=AXIS2_PLACEMENT_3D('',#36349,#15278,#15279);
#12399=AXIS2_PLACEMENT_3D('',#36351,#15280,#15281);
#12400=AXIS2_PLACEMENT_3D('',#36352,#15282,#15283);
#12401=AXIS2_PLACEMENT_3D('',#36353,#15284,#15285);
#12402=AXIS2_PLACEMENT_3D('',#36355,#15286,#15287);
#12403=AXIS2_PLACEMENT_3D('',#36356,#15288,#15289);
#12404=AXIS2_PLACEMENT_3D('',#36358,#15291,#15292);
#12405=AXIS2_PLACEMENT_3D('',#36365,#15296,#15297);
#12406=AXIS2_PLACEMENT_3D('',#36369,#15300,#15301);
#12407=AXIS2_PLACEMENT_3D('',#36373,#15304,#15305);
#12408=AXIS2_PLACEMENT_3D('',#36377,#15308,#15309);
#12409=AXIS2_PLACEMENT_3D('',#36381,#15312,#15313);
#12410=AXIS2_PLACEMENT_3D('',#36383,#15315,#15316);
#12411=AXIS2_PLACEMENT_3D('',#36389,#15320,#15321);
#12412=AXIS2_PLACEMENT_3D('',#36393,#15324,#15325);
#12413=AXIS2_PLACEMENT_3D('',#36397,#15328,#15329);
#12414=AXIS2_PLACEMENT_3D('',#36401,#15332,#15333);
#12415=AXIS2_PLACEMENT_3D('',#36405,#15336,#15337);
#12416=AXIS2_PLACEMENT_3D('',#36407,#15339,#15340);
#12417=AXIS2_PLACEMENT_3D('',#36408,#15341,#15342);
#12418=AXIS2_PLACEMENT_3D('',#36410,#15343,#15344);
#12419=AXIS2_PLACEMENT_3D('',#36411,#15345,#15346);
#12420=AXIS2_PLACEMENT_3D('',#36412,#15347,#15348);
#12421=AXIS2_PLACEMENT_3D('',#36413,#15349,#15350);
#12422=AXIS2_PLACEMENT_3D('',#36414,#15351,#15352);
#12423=AXIS2_PLACEMENT_3D('',#36415,#15353,#15354);
#12424=AXIS2_PLACEMENT_3D('',#36416,#15355,#15356);
#12425=AXIS2_PLACEMENT_3D('',#36417,#15357,#15358);
#12426=AXIS2_PLACEMENT_3D('',#36418,#15359,#15360);
#12427=AXIS2_PLACEMENT_3D('',#36419,#15361,#15362);
#12428=AXIS2_PLACEMENT_3D('',#36420,#15363,#15364);
#12429=AXIS2_PLACEMENT_3D('',#36421,#15365,#15366);
#12430=AXIS2_PLACEMENT_3D('',#36422,#15367,#15368);
#12431=AXIS2_PLACEMENT_3D('',#36423,#15369,#15370);
#12432=AXIS2_PLACEMENT_3D('',#36424,#15371,#15372);
#12433=AXIS2_PLACEMENT_3D('',#36425,#15373,#15374);
#12434=AXIS2_PLACEMENT_3D('',#36426,#15375,#15376);
#12435=AXIS2_PLACEMENT_3D('',#36427,#15377,#15378);
#12436=AXIS2_PLACEMENT_3D('',#36428,#15379,#15380);
#12437=DIRECTION('axis',(0.,0.,1.));
#12438=DIRECTION('refdir',(1.,0.,0.));
#12439=DIRECTION('axis',(0.,0.,1.));
#12440=DIRECTION('refdir',(1.,0.,0.));
#12441=DIRECTION('center_axis',(0.,0.,1.));
#12442=DIRECTION('ref_axis',(1.,0.,0.));
#12443=DIRECTION('center_axis',(0.,0.,-1.));
#12444=DIRECTION('ref_axis',(-1.,0.,0.));
#12445=DIRECTION('',(0.,0.,-1.));
#12446=DIRECTION('center_axis',(0.,0.,1.));
#12447=DIRECTION('ref_axis',(-1.,0.,0.));
#12448=DIRECTION('center_axis',(0.,0.,1.));
#12449=DIRECTION('ref_axis',(-1.,0.,0.));
#12450=DIRECTION('center_axis',(0.,0.,-1.));
#12451=DIRECTION('ref_axis',(-1.,0.,0.));
#12452=DIRECTION('center_axis',(0.,-1.,0.));
#12453=DIRECTION('ref_axis',(1.,0.,0.));
#12454=DIRECTION('center_axis',(0.,1.,0.));
#12455=DIRECTION('ref_axis',(-0.662700408463881,0.,0.748884616360762));
#12456=DIRECTION('center_axis',(0.,0.,-1.));
#12457=DIRECTION('ref_axis',(-1.,0.,0.));
#12458=DIRECTION('center_axis',(-1.,-1.23033231110227E-14,1.91813075638571E-13));
#12459=DIRECTION('ref_axis',(-1.51799278823133E-13,0.662700408404006,-0.748884616413746));
#12460=DIRECTION('center_axis',(-1.,-6.87436171423541E-14,6.46003611483159E-13));
#12461=DIRECTION('ref_axis',(-5.29338589993441E-13,0.662700408303445,-0.748884616502734));
#12462=DIRECTION('center_axis',(0.,0.,-1.));
#12463=DIRECTION('ref_axis',(-1.,0.,0.));
#12464=DIRECTION('center_axis',(-2.42515865283882E-14,1.,-2.2795089778668E-13));
#12465=DIRECTION('ref_axis',(0.628654464794611,1.92519804155958E-13,0.777684745828154));
#12466=DIRECTION('center_axis',(2.42515865283884E-14,1.,2.27950897786681E-13));
#12467=DIRECTION('ref_axis',(0.628654464776,-1.92519804158937E-13,0.777684745843199));
#12468=DIRECTION('center_axis',(0.,0.,-1.));
#12469=DIRECTION('ref_axis',(-1.,0.,0.));
#12470=DIRECTION('center_axis',(-1.,-4.42963920865616E-14,-3.40131136130303E-13));
#12471=DIRECTION('ref_axis',(2.92361920824713E-13,-0.628654464727554,-0.777684745882361));
#12472=DIRECTION('center_axis',(-1.,-8.06737718791901E-14,-6.82057482811295E-13));
#12473=DIRECTION('ref_axis',(5.81141627215589E-13,-0.628654464429985,-0.777684746122906));
#12474=DIRECTION('center_axis',(0.,0.,-1.));
#12475=DIRECTION('ref_axis',(-1.,0.,0.));
#12476=DIRECTION('center_axis',(-4.02653252918805E-14,1.,3.02189686082951E-13));
#12477=DIRECTION('ref_axis',(-0.662700408561431,-2.52989054626112E-13,0.748884616274438));
#12478=DIRECTION('center_axis',(0.,0.,-1.));
#12479=DIRECTION('ref_axis',(-1.,0.,0.));
#12480=DIRECTION('',(0.,-1.,0.));
#12481=DIRECTION('',(-1.,0.,0.));
#12482=DIRECTION('center_axis',(0.,0.,-1.));
#12483=DIRECTION('ref_axis',(-1.,0.,0.));
#12484=DIRECTION('',(-1.,0.,0.));
#12485=DIRECTION('',(0.,-1.,0.));
#12486=DIRECTION('center_axis',(0.,0.,-1.));
#12487=DIRECTION('ref_axis',(-1.,0.,0.));
#12488=DIRECTION('',(0.,-1.,0.));
#12489=DIRECTION('',(-1.,0.,0.));
#12490=DIRECTION('center_axis',(0.,0.,-1.));
#12491=DIRECTION('ref_axis',(-1.,0.,0.));
#12492=DIRECTION('center_axis',(0.,0.,-1.));
#12493=DIRECTION('ref_axis',(-1.,0.,0.));
#12494=DIRECTION('',(0.,-1.,0.));
#12495=DIRECTION('',(-1.,0.,0.));
#12496=DIRECTION('center_axis',(1.,0.,0.));
#12497=DIRECTION('ref_axis',(0.,0.,-1.));
#12498=DIRECTION('',(0.,0.,-1.));
#12499=DIRECTION('',(0.,-1.,0.));
#12500=DIRECTION('',(0.,0.,-1.));
#12501=DIRECTION('center_axis',(1.,0.,0.));
#12502=DIRECTION('ref_axis',(0.,0.,-1.));
#12503=DIRECTION('',(0.,0.,-1.));
#12504=DIRECTION('',(0.,-1.,0.));
#12505=DIRECTION('',(0.,0.,-1.));
#12506=DIRECTION('center_axis',(1.,0.,0.));
#12507=DIRECTION('ref_axis',(0.,0.,-1.));
#12508=DIRECTION('',(0.,0.,-1.));
#12509=DIRECTION('',(0.,-1.,0.));
#12510=DIRECTION('',(0.,0.,-1.));
#12511=DIRECTION('center_axis',(0.,-1.,0.));
#12512=DIRECTION('ref_axis',(0.,0.,-1.));
#12513=DIRECTION('',(-1.,0.,0.));
#12514=DIRECTION('center_axis',(1.,0.,0.));
#12515=DIRECTION('ref_axis',(0.,0.,-1.));
#12516=DIRECTION('',(0.,0.,-1.));
#12517=DIRECTION('',(0.,-1.,0.));
#12518=DIRECTION('',(0.,0.,-1.));
#12519=DIRECTION('center_axis',(0.,1.,0.));
#12520=DIRECTION('ref_axis',(0.,0.,1.));
#12521=DIRECTION('',(1.,0.,0.));
#12522=DIRECTION('center_axis',(0.,0.,-1.));
#12523=DIRECTION('ref_axis',(-1.,0.,0.));
#12524=DIRECTION('',(-1.,0.,0.));
#12525=DIRECTION('',(0.,-1.,0.));
#12526=DIRECTION('',(-1.,0.,0.));
#12527=DIRECTION('',(-1.,0.,0.));
#12528=DIRECTION('',(0.,1.,0.));
#12529=DIRECTION('',(-1.,0.,0.));
#12530=DIRECTION('center_axis',(1.,0.,0.));
#12531=DIRECTION('ref_axis',(0.,0.,-1.));
#12532=DIRECTION('',(0.,0.,-1.));
#12533=DIRECTION('',(0.,0.,-1.));
#12534=DIRECTION('center_axis',(0.,-1.,0.));
#12535=DIRECTION('ref_axis',(0.,0.,-1.));
#12536=DIRECTION('center_axis',(0.,-1.,0.));
#12537=DIRECTION('ref_axis',(0.,0.,-1.));
#12538=DIRECTION('center_axis',(0.,-1.,0.));
#12539=DIRECTION('ref_axis',(0.,0.,-1.));
#12540=DIRECTION('',(0.,0.,-1.));
#12541=DIRECTION('center_axis',(-1.,0.,0.));
#12542=DIRECTION('ref_axis',(0.,0.,1.));
#12543=DIRECTION('',(0.,0.,-1.));
#12544=DIRECTION('center_axis',(0.,-1.,0.));
#12545=DIRECTION('ref_axis',(0.,0.,-1.));
#12546=DIRECTION('center_axis',(4.16203559120935E-32,4.16203559120936E-32,
1.));
#12547=DIRECTION('ref_axis',(-3.27821759239711E-15,1.,-4.16203559120935E-32));
#12548=DIRECTION('center_axis',(-4.16203559120935E-32,-4.16203559120936E-32,
-1.));
#12549=DIRECTION('ref_axis',(3.27821759239712E-15,-1.,4.16203559120935E-32));
#12550=DIRECTION('',(-4.16203559120935E-32,-4.16203559120936E-32,-1.));
#12551=DIRECTION('center_axis',(4.16203559120935E-32,4.16203559120936E-32,
1.));
#12552=DIRECTION('ref_axis',(3.27821759239712E-15,-1.,4.16203559120935E-32));
#12553=DIRECTION('center_axis',(4.16203559120935E-32,4.16203559120936E-32,
1.));
#12554=DIRECTION('ref_axis',(3.27821759239712E-15,-1.,4.16203559120935E-32));
#12555=DIRECTION('center_axis',(-4.16203559120935E-32,-4.16203559120936E-32,
-1.));
#12556=DIRECTION('ref_axis',(3.35689481461465E-15,-1.,0.));
#12557=DIRECTION('center_axis',(1.,3.49676543189026E-15,-4.16203559120936E-32));
#12558=DIRECTION('ref_axis',(-3.49676543189026E-15,1.,0.));
#12559=DIRECTION('center_axis',(-1.,-2.79620021808786E-14,1.10376610444469E-13));
#12560=DIRECTION('ref_axis',(-1.01189775835862E-13,0.6627004084464,-0.748884616376231));
#12561=DIRECTION('center_axis',(-4.16203559120935E-32,-4.16203559120936E-32,
-1.));
#12562=DIRECTION('ref_axis',(3.64246399155235E-15,-1.,4.16203559120935E-32));
#12563=DIRECTION('center_axis',(5.22244552899185E-14,-1.,3.38377885085167E-13));
#12564=DIRECTION('ref_axis',(-0.662700408929437,-2.88015160394313E-13,-0.748884615948783));
#12565=DIRECTION('center_axis',(9.67056193232502E-14,-1.,7.56380221927762E-13));
#12566=DIRECTION('ref_axis',(-0.662700408393056,-6.30528365788067E-13,-0.748884616423436));
#12567=DIRECTION('center_axis',(-4.16203559120935E-32,-4.16203559120936E-32,
-1.));
#12568=DIRECTION('ref_axis',(3.64246399155235E-15,-1.,4.16203559120935E-32));
#12569=DIRECTION('center_axis',(-1.,-3.21705988223668E-14,-2.26155687236952E-13));
#12570=DIRECTION('ref_axis',(1.96102018725182E-13,-0.62865446483494,-0.777684745795554));
#12571=DIRECTION('center_axis',(-1.,1.63325742344061E-14,2.29746108336374E-13));
#12572=DIRECTION('ref_axis',(-1.88937589565396E-13,-0.628654464884546,-0.777684745755454));
#12573=DIRECTION('center_axis',(-4.16203559120935E-32,-4.16203559120936E-32,
-1.));
#12574=DIRECTION('ref_axis',(3.64246399155235E-15,-1.,4.16203559120935E-32));
#12575=DIRECTION('center_axis',(4.81734732924783E-14,-1.,-3.00344109282818E-13));
#12576=DIRECTION('ref_axis',(0.628654464809676,2.6385750135564E-13,-0.777684745815976));
#12577=DIRECTION('center_axis',(7.6631840791126E-14,-1.,-6.44065666513476E-13));
#12578=DIRECTION('ref_axis',(0.628654464493172,5.49054993151786E-13,-0.777684746071827));
#12579=DIRECTION('center_axis',(-4.16203559120935E-32,-4.16203559120936E-32,
-1.));
#12580=DIRECTION('ref_axis',(3.64246399155235E-15,-1.,4.16203559120935E-32));
#12581=DIRECTION('center_axis',(-1.,-5.22244552898928E-14,3.38377885085076E-13));
#12582=DIRECTION('ref_axis',(-2.88015160457499E-13,0.662700408673497,-0.748884616175269));
#12583=DIRECTION('center_axis',(-4.16203559120935E-32,-4.16203559120936E-32,
-1.));
#12584=DIRECTION('ref_axis',(3.49148133884313E-15,-1.,4.16203559120935E-32));
#12585=DIRECTION('',(1.,3.49148133884313E-15,-4.16203559120936E-32));
#12586=DIRECTION('',(3.49148133884313E-15,-1.,4.16203559120935E-32));
#12587=DIRECTION('center_axis',(-4.16203559120935E-32,-4.16203559120936E-32,
-1.));
#12588=DIRECTION('ref_axis',(3.49148133884313E-15,-1.,4.16203559120935E-32));
#12589=DIRECTION('',(3.49148133884313E-15,-1.,4.16203559120935E-32));
#12590=DIRECTION('',(1.,3.49148133884313E-15,-4.16203559120936E-32));
#12591=DIRECTION('center_axis',(-4.16203559120935E-32,-4.16203559120936E-32,
-1.));
#12592=DIRECTION('ref_axis',(3.49148133884313E-15,-1.,4.16203559120935E-32));
#12593=DIRECTION('',(1.,3.49148133884313E-15,-4.16203559120936E-32));
#12594=DIRECTION('',(3.49148133884313E-15,-1.,4.16203559120935E-32));
#12595=DIRECTION('center_axis',(-4.16203559120935E-32,-4.16203559120936E-32,
-1.));
#12596=DIRECTION('ref_axis',(3.49148133884313E-15,-1.,4.16203559120935E-32));
#12597=DIRECTION('center_axis',(-4.16203559120935E-32,-4.16203559120936E-32,
-1.));
#12598=DIRECTION('ref_axis',(3.49148133884313E-15,-1.,4.16203559120935E-32));
#12599=DIRECTION('',(1.,3.49148133884313E-15,-4.16203559120936E-32));
#12600=DIRECTION('',(3.49148133884313E-15,-1.,4.16203559120935E-32));
#12601=DIRECTION('center_axis',(-3.49148133884313E-15,1.,-4.16203559120935E-32));
#12602=DIRECTION('ref_axis',(-4.16203559120935E-32,-4.16203559120937E-32,
-1.));
#12603=DIRECTION('',(-4.16203559120935E-32,-4.16203559120936E-32,-1.));
#12604=DIRECTION('',(1.,3.49148133884313E-15,-4.16203559120936E-32));
#12605=DIRECTION('',(-4.16203559120935E-32,-4.16203559120936E-32,-1.));
#12606=DIRECTION('center_axis',(-3.49148133884313E-15,1.,-4.16203559120935E-32));
#12607=DIRECTION('ref_axis',(-4.16203559120935E-32,-4.16203559120937E-32,
-1.));
#12608=DIRECTION('',(-4.16203559120935E-32,-4.16203559120936E-32,-1.));
#12609=DIRECTION('',(1.,3.49148133884313E-15,-4.16203559120936E-32));
#12610=DIRECTION('',(-4.16203559120935E-32,-4.16203559120936E-32,-1.));
#12611=DIRECTION('center_axis',(-3.49148133884313E-15,1.,-4.16203559120935E-32));
#12612=DIRECTION('ref_axis',(-4.16203559120935E-32,-4.16203559120937E-32,
-1.));
#12613=DIRECTION('',(-4.16203559120935E-32,-4.16203559120936E-32,-1.));
#12614=DIRECTION('',(1.,3.49148133884313E-15,-4.16203559120936E-32));
#12615=DIRECTION('',(-4.16203559120935E-32,-4.16203559120936E-32,-1.));
#12616=DIRECTION('center_axis',(1.,3.49148133884313E-15,-4.16203559120936E-32));
#12617=DIRECTION('ref_axis',(-4.16203559120935E-32,-4.16203559120936E-32,
-1.));
#12618=DIRECTION('',(3.49148133884313E-15,-1.,4.16203559120935E-32));
#12619=DIRECTION('center_axis',(-3.49148133884313E-15,1.,-4.16203559120935E-32));
#12620=DIRECTION('ref_axis',(-4.16203559120935E-32,-4.16203559120937E-32,
-1.));
#12621=DIRECTION('',(-4.16203559120935E-32,-4.16203559120936E-32,-1.));
#12622=DIRECTION('',(1.,3.49148133884313E-15,-4.16203559120936E-32));
#12623=DIRECTION('',(-4.16203559120935E-32,-4.16203559120936E-32,-1.));
#12624=DIRECTION('center_axis',(-1.,-3.49148133884313E-15,4.16203559120936E-32));
#12625=DIRECTION('ref_axis',(4.16203559120935E-32,4.16203559120936E-32,
1.));
#12626=DIRECTION('',(-3.49148133884313E-15,1.,-4.16203559120935E-32));
#12627=DIRECTION('center_axis',(-4.16203559120935E-32,-4.16203559120936E-32,
-1.));
#12628=DIRECTION('ref_axis',(3.49148133884313E-15,-1.,4.16203559120935E-32));
#12629=DIRECTION('',(3.49148133884313E-15,-1.,4.16203559120935E-32));
#12630=DIRECTION('',(1.,3.49148133884313E-15,-4.16203559120936E-32));
#12631=DIRECTION('',(3.49148133884313E-15,-1.,4.16203559120935E-32));
#12632=DIRECTION('',(3.49148133884313E-15,-1.,4.16203559120935E-32));
#12633=DIRECTION('',(-1.,-3.49148133884313E-15,4.16203559120936E-32));
#12634=DIRECTION('',(3.49148133884313E-15,-1.,4.16203559120935E-32));
#12635=DIRECTION('center_axis',(-3.49148133884313E-15,1.,-4.16203559120935E-32));
#12636=DIRECTION('ref_axis',(-4.16203559120935E-32,-4.16203559120937E-32,
-1.));
#12637=DIRECTION('',(-4.16203559120935E-32,-4.16203559120936E-32,-1.));
#12638=DIRECTION('',(-4.16203559120935E-32,-4.16203559120936E-32,-1.));
#12639=DIRECTION('center_axis',(1.,3.49148133884313E-15,-4.16203559120936E-32));
#12640=DIRECTION('ref_axis',(-4.16203559120935E-32,-4.16203559120936E-32,
-1.));
#12641=DIRECTION('center_axis',(1.,3.49148133884313E-15,-4.16203559120936E-32));
#12642=DIRECTION('ref_axis',(-4.16203559120935E-32,-4.16203559120936E-32,
-1.));
#12643=DIRECTION('center_axis',(1.,3.49148133884313E-15,-4.16203559120936E-32));
#12644=DIRECTION('ref_axis',(-4.16203559120935E-32,-4.16203559120936E-32,
-1.));
#12645=DIRECTION('',(-4.16203559120935E-32,-4.16203559120936E-32,-1.));
#12646=DIRECTION('center_axis',(3.49148133884313E-15,-1.,4.16203559120935E-32));
#12647=DIRECTION('ref_axis',(4.16203559120935E-32,4.16203559120937E-32,
1.));
#12648=DIRECTION('',(-4.16203559120935E-32,-4.16203559120936E-32,-1.));
#12649=DIRECTION('center_axis',(1.,3.49148133884313E-15,-4.16203559120936E-32));
#12650=DIRECTION('ref_axis',(-4.16203559120935E-32,-4.16203559120936E-32,
-1.));
#12651=DIRECTION('center_axis',(0.,8.3240711824187E-32,1.));
#12652=DIRECTION('ref_axis',(-1.,0.,0.));
#12653=DIRECTION('center_axis',(0.,-8.3240711824187E-32,-1.));
#12654=DIRECTION('ref_axis',(1.,0.,0.));
#12655=DIRECTION('',(0.,-8.3240711824187E-32,-1.));
#12656=DIRECTION('center_axis',(0.,8.3240711824187E-32,1.));
#12657=DIRECTION('ref_axis',(1.,0.,0.));
#12658=DIRECTION('center_axis',(0.,8.3240711824187E-32,1.));
#12659=DIRECTION('ref_axis',(1.,0.,0.));
#12660=DIRECTION('center_axis',(0.,-8.3240711824187E-32,-1.));
#12661=DIRECTION('ref_axis',(1.,0.,0.));
#12662=DIRECTION('center_axis',(0.,1.,-8.3240711824187E-32));
#12663=DIRECTION('ref_axis',(-1.,0.,0.));
#12664=DIRECTION('center_axis',(0.,-1.,0.));
#12665=DIRECTION('ref_axis',(-0.662700408463881,0.,-0.748884616360762));
#12666=DIRECTION('center_axis',(0.,-8.3240711824187E-32,-1.));
#12667=DIRECTION('ref_axis',(1.,0.,0.));
#12668=DIRECTION('center_axis',(1.,1.23033231110227E-14,1.91813075638571E-13));
#12669=DIRECTION('ref_axis',(-1.51799278823133E-13,0.662700408404006,0.748884616413746));
#12670=DIRECTION('center_axis',(1.,6.87436171423541E-14,6.46003611483159E-13));
#12671=DIRECTION('ref_axis',(-5.29338589993441E-13,0.662700408303445,0.748884616502734));
#12672=DIRECTION('center_axis',(0.,-8.3240711824187E-32,-1.));
#12673=DIRECTION('ref_axis',(1.,0.,0.));
#12674=DIRECTION('center_axis',(2.42515865283882E-14,-1.,-2.2795089778668E-13));
#12675=DIRECTION('ref_axis',(0.628654464794611,1.92519804155958E-13,-0.777684745828154));
#12676=DIRECTION('center_axis',(-2.42515865283884E-14,-1.,2.27950897786681E-13));
#12677=DIRECTION('ref_axis',(0.628654464776,-1.92519804158937E-13,-0.777684745843199));
#12678=DIRECTION('center_axis',(0.,-8.3240711824187E-32,-1.));
#12679=DIRECTION('ref_axis',(1.,0.,0.));
#12680=DIRECTION('center_axis',(1.,4.42963920865616E-14,-3.40131136130303E-13));
#12681=DIRECTION('ref_axis',(2.92361920824713E-13,-0.628654464727554,0.777684745882361));
#12682=DIRECTION('center_axis',(1.,8.06737718791901E-14,-6.82057482811295E-13));
#12683=DIRECTION('ref_axis',(5.81141627215589E-13,-0.628654464429985,0.777684746122906));
#12684=DIRECTION('center_axis',(0.,-8.3240711824187E-32,-1.));
#12685=DIRECTION('ref_axis',(1.,0.,0.));
#12686=DIRECTION('center_axis',(4.02653252918805E-14,-1.,3.02189686082951E-13));
#12687=DIRECTION('ref_axis',(-0.662700408561431,-2.52989054626112E-13,-0.748884616274438));
#12688=DIRECTION('center_axis',(0.,-8.3240711824187E-32,-1.));
#12689=DIRECTION('ref_axis',(1.,0.,0.));
#12690=DIRECTION('',(0.,1.,-8.3240711824187E-32));
#12691=DIRECTION('',(1.,0.,0.));
#12692=DIRECTION('center_axis',(0.,-8.3240711824187E-32,-1.));
#12693=DIRECTION('ref_axis',(1.,0.,0.));
#12694=DIRECTION('',(1.,0.,0.));
#12695=DIRECTION('',(0.,1.,-8.3240711824187E-32));
#12696=DIRECTION('center_axis',(0.,-8.3240711824187E-32,-1.));
#12697=DIRECTION('ref_axis',(1.,0.,0.));
#12698=DIRECTION('',(0.,1.,-8.3240711824187E-32));
#12699=DIRECTION('',(1.,0.,0.));
#12700=DIRECTION('center_axis',(0.,-8.3240711824187E-32,-1.));
#12701=DIRECTION('ref_axis',(1.,0.,0.));
#12702=DIRECTION('center_axis',(0.,-8.3240711824187E-32,-1.));
#12703=DIRECTION('ref_axis',(1.,0.,0.));
#12704=DIRECTION('',(0.,1.,-8.3240711824187E-32));
#12705=DIRECTION('',(1.,0.,0.));
#12706=DIRECTION('center_axis',(-1.,0.,0.));
#12707=DIRECTION('ref_axis',(0.,-8.3240711824187E-32,-1.));
#12708=DIRECTION('',(0.,-8.3240711824187E-32,-1.));
#12709=DIRECTION('',(0.,1.,-8.3240711824187E-32));
#12710=DIRECTION('',(0.,-8.3240711824187E-32,-1.));
#12711=DIRECTION('center_axis',(-1.,0.,0.));
#12712=DIRECTION('ref_axis',(0.,-8.3240711824187E-32,-1.));
#12713=DIRECTION('',(0.,-8.3240711824187E-32,-1.));
#12714=DIRECTION('',(0.,1.,-8.3240711824187E-32));
#12715=DIRECTION('',(0.,-8.3240711824187E-32,-1.));
#12716=DIRECTION('center_axis',(-1.,0.,0.));
#12717=DIRECTION('ref_axis',(0.,-8.3240711824187E-32,-1.));
#12718=DIRECTION('',(0.,-8.3240711824187E-32,-1.));
#12719=DIRECTION('',(0.,1.,-8.3240711824187E-32));
#12720=DIRECTION('',(0.,-8.3240711824187E-32,-1.));
#12721=DIRECTION('center_axis',(0.,1.,-8.3240711824187E-32));
#12722=DIRECTION('ref_axis',(0.,-8.3240711824187E-32,-1.));
#12723=DIRECTION('',(1.,0.,0.));
#12724=DIRECTION('center_axis',(-1.,0.,0.));
#12725=DIRECTION('ref_axis',(0.,-8.3240711824187E-32,-1.));
#12726=DIRECTION('',(0.,-8.3240711824187E-32,-1.));
#12727=DIRECTION('',(0.,1.,-8.3240711824187E-32));
#12728=DIRECTION('',(0.,-8.3240711824187E-32,-1.));
#12729=DIRECTION('center_axis',(0.,-1.,8.3240711824187E-32));
#12730=DIRECTION('ref_axis',(0.,8.3240711824187E-32,1.));
#12731=DIRECTION('',(-1.,0.,0.));
#12732=DIRECTION('center_axis',(0.,-8.3240711824187E-32,-1.));
#12733=DIRECTION('ref_axis',(1.,0.,0.));
#12734=DIRECTION('',(1.,0.,0.));
#12735=DIRECTION('',(0.,1.,-8.3240711824187E-32));
#12736=DIRECTION('',(1.,0.,0.));
#12737=DIRECTION('',(1.,0.,0.));
#12738=DIRECTION('',(0.,-1.,8.3240711824187E-32));
#12739=DIRECTION('',(1.,0.,0.));
#12740=DIRECTION('center_axis',(-1.,0.,0.));
#12741=DIRECTION('ref_axis',(0.,-8.3240711824187E-32,-1.));
#12742=DIRECTION('',(0.,-8.3240711824187E-32,-1.));
#12743=DIRECTION('',(0.,-8.3240711824187E-32,-1.));
#12744=DIRECTION('center_axis',(0.,1.,-8.3240711824187E-32));
#12745=DIRECTION('ref_axis',(0.,-8.3240711824187E-32,-1.));
#12746=DIRECTION('center_axis',(0.,1.,-8.3240711824187E-32));
#12747=DIRECTION('ref_axis',(0.,-8.3240711824187E-32,-1.));
#12748=DIRECTION('center_axis',(0.,1.,-8.3240711824187E-32));
#12749=DIRECTION('ref_axis',(0.,-8.3240711824187E-32,-1.));
#12750=DIRECTION('',(0.,-8.3240711824187E-32,-1.));
#12751=DIRECTION('center_axis',(1.,0.,0.));
#12752=DIRECTION('ref_axis',(0.,8.3240711824187E-32,1.));
#12753=DIRECTION('',(0.,-8.3240711824187E-32,-1.));
#12754=DIRECTION('center_axis',(0.,1.,-8.3240711824187E-32));
#12755=DIRECTION('ref_axis',(0.,-8.3240711824187E-32,-1.));
#12756=DIRECTION('center_axis',(-4.16203559120935E-32,4.16203559120931E-32,
1.));
#12757=DIRECTION('ref_axis',(1.03810223759242E-14,-1.,4.16203559120935E-32));
#12758=DIRECTION('center_axis',(4.16203559120935E-32,-4.16203559120931E-32,
-1.));
#12759=DIRECTION('ref_axis',(-1.03810223759242E-14,1.,-4.16203559120935E-32));
#12760=DIRECTION('',(4.16203559120935E-32,-4.16203559120931E-32,-1.));
#12761=DIRECTION('center_axis',(-4.16203559120935E-32,4.16203559120931E-32,
1.));
#12762=DIRECTION('ref_axis',(-9.83465277719135E-15,1.,-4.16203559120935E-32));
#12763=DIRECTION('center_axis',(-4.16203559120935E-32,4.16203559120931E-32,
1.));
#12764=DIRECTION('ref_axis',(-9.83465277719135E-15,1.,-4.16203559120935E-32));
#12765=DIRECTION('center_axis',(4.16203559120935E-32,-4.16203559120931E-32,
-1.));
#12766=DIRECTION('ref_axis',(-1.00706844438439E-14,1.,0.));
#12767=DIRECTION('center_axis',(-1.,-9.79094320929272E-15,-4.16203559120931E-32));
#12768=DIRECTION('ref_axis',(9.79094320929272E-15,-1.,0.));
#12769=DIRECTION('center_axis',(1.,3.18336478092136E-14,7.05643845663474E-14));
#12770=DIRECTION('ref_axis',(-7.39407534612729E-14,0.66270040877393,0.748884616086394));
#12771=DIRECTION('center_axis',(4.16203559120935E-32,-4.16203559120931E-32,
-1.));
#12772=DIRECTION('ref_axis',(-1.0927391974657E-14,1.,-4.16203559120936E-32));
#12773=DIRECTION('center_axis',(-4.81807131050712E-14,1.,3.00377672645013E-13));
#12774=DIRECTION('ref_axis',(-0.662700408385393,-2.56877596413992E-13,0.748884616430217));
#12775=DIRECTION('center_axis',(-5.66123905878238E-14,1.,5.32002974162615E-13));
#12776=DIRECTION('ref_axis',(-0.662700408320119,-4.35925897634763E-13,0.748884616487979));
#12777=DIRECTION('center_axis',(4.16203559120935E-32,-4.16203559120931E-32,
-1.));
#12778=DIRECTION('ref_axis',(-1.0927391974657E-14,1.,-4.16203559120936E-32));
#12779=DIRECTION('center_axis',(1.,3.62125299104317E-14,-2.64147503534732E-13));
#12780=DIRECTION('ref_axis',(2.28188652755739E-13,-0.628654464803139,0.777684745821261));
#12781=DIRECTION('center_axis',(1.,-8.41356194042581E-15,2.31541318886086E-13));
#12782=DIRECTION('ref_axis',(-1.85355374991887E-13,-0.628654464869737,0.777684745767425));
#12783=DIRECTION('center_axis',(4.16203559120935E-32,-4.16203559120931E-32,
-1.));
#12784=DIRECTION('ref_axis',(-1.0927391974657E-14,1.,-4.16203559120936E-32));
#12785=DIRECTION('center_axis',(-5.60924855864494E-14,1.,-2.98548898733053E-13));
#12786=DIRECTION('ref_axis',(0.628654464448989,2.67439715997863E-13,0.777684746107544));
#12787=DIRECTION('center_axis',(-8.06737718791917E-14,1.,-6.82057482811304E-13));
#12788=DIRECTION('ref_axis',(0.628654464496999,5.81141627184055E-13,0.777684746068734));
#12789=DIRECTION('center_axis',(4.16203559120935E-32,-4.16203559120931E-32,
-1.));
#12790=DIRECTION('ref_axis',(-1.0927391974657E-14,1.,-4.16203559120936E-32));
#12791=DIRECTION('center_axis',(1.,2.42624531090294E-14,2.28001274640695E-13));
#12792=DIRECTION('ref_axis',(-1.86825384661082E-13,0.662700408540891,0.748884616292614));
#12793=DIRECTION('center_axis',(4.16203559120935E-32,-4.16203559120931E-32,
-1.));
#12794=DIRECTION('ref_axis',(-1.04744440165294E-14,1.,-4.16203559120935E-32));
#12795=DIRECTION('',(-1.,-1.04744440165294E-14,-4.16203559120931E-32));
#12796=DIRECTION('',(-1.04744440165294E-14,1.,-4.16203559120935E-32));
#12797=DIRECTION('center_axis',(4.16203559120935E-32,-4.16203559120931E-32,
-1.));
#12798=DIRECTION('ref_axis',(-1.04744440165294E-14,1.,-4.16203559120935E-32));
#12799=DIRECTION('',(-1.04744440165294E-14,1.,-4.16203559120935E-32));
#12800=DIRECTION('',(-1.,-1.04744440165294E-14,-4.16203559120931E-32));
#12801=DIRECTION('center_axis',(4.16203559120935E-32,-4.16203559120931E-32,
-1.));
#12802=DIRECTION('ref_axis',(-1.04744440165294E-14,1.,-4.16203559120935E-32));
#12803=DIRECTION('',(-1.,-1.04744440165294E-14,-4.16203559120931E-32));
#12804=DIRECTION('',(-1.04744440165294E-14,1.,-4.16203559120935E-32));
#12805=DIRECTION('center_axis',(4.16203559120935E-32,-4.16203559120931E-32,
-1.));
#12806=DIRECTION('ref_axis',(-1.04744440165294E-14,1.,-4.16203559120935E-32));
#12807=DIRECTION('center_axis',(4.16203559120935E-32,-4.16203559120931E-32,
-1.));
#12808=DIRECTION('ref_axis',(-1.04744440165294E-14,1.,-4.16203559120935E-32));
#12809=DIRECTION('',(-1.,-1.04744440165294E-14,-4.16203559120931E-32));
#12810=DIRECTION('',(-1.04744440165294E-14,1.,-4.16203559120935E-32));
#12811=DIRECTION('center_axis',(1.04744440165294E-14,-1.,4.16203559120935E-32));
#12812=DIRECTION('ref_axis',(4.16203559120935E-32,-4.16203559120931E-32,
-1.));
#12813=DIRECTION('',(4.16203559120935E-32,-4.16203559120931E-32,-1.));
#12814=DIRECTION('',(-1.,-1.04744440165294E-14,-4.16203559120931E-32));
#12815=DIRECTION('',(4.16203559120935E-32,-4.16203559120931E-32,-1.));
#12816=DIRECTION('center_axis',(1.04744440165294E-14,-1.,4.16203559120935E-32));
#12817=DIRECTION('ref_axis',(4.16203559120935E-32,-4.16203559120931E-32,
-1.));
#12818=DIRECTION('',(4.16203559120935E-32,-4.16203559120931E-32,-1.));
#12819=DIRECTION('',(-1.,-1.04744440165294E-14,-4.16203559120931E-32));
#12820=DIRECTION('',(4.16203559120935E-32,-4.16203559120931E-32,-1.));
#12821=DIRECTION('center_axis',(1.04744440165294E-14,-1.,4.16203559120935E-32));
#12822=DIRECTION('ref_axis',(4.16203559120935E-32,-4.16203559120931E-32,
-1.));
#12823=DIRECTION('',(4.16203559120935E-32,-4.16203559120931E-32,-1.));
#12824=DIRECTION('',(-1.,-1.04744440165294E-14,-4.16203559120931E-32));
#12825=DIRECTION('',(4.16203559120935E-32,-4.16203559120931E-32,-1.));
#12826=DIRECTION('center_axis',(-1.,-1.04744440165294E-14,-4.16203559120931E-32));
#12827=DIRECTION('ref_axis',(4.16203559120935E-32,-4.16203559120931E-32,
-1.));
#12828=DIRECTION('',(-1.04744440165294E-14,1.,-4.16203559120935E-32));
#12829=DIRECTION('center_axis',(1.04744440165294E-14,-1.,4.16203559120935E-32));
#12830=DIRECTION('ref_axis',(4.16203559120935E-32,-4.16203559120931E-32,
-1.));
#12831=DIRECTION('',(4.16203559120935E-32,-4.16203559120931E-32,-1.));
#12832=DIRECTION('',(-1.,-1.04744440165294E-14,-4.16203559120931E-32));
#12833=DIRECTION('',(4.16203559120935E-32,-4.16203559120931E-32,-1.));
#12834=DIRECTION('center_axis',(1.,1.04744440165294E-14,4.16203559120931E-32));
#12835=DIRECTION('ref_axis',(-4.16203559120935E-32,4.16203559120931E-32,
1.));
#12836=DIRECTION('',(1.04744440165294E-14,-1.,4.16203559120935E-32));
#12837=DIRECTION('center_axis',(4.16203559120935E-32,-4.16203559120931E-32,
-1.));
#12838=DIRECTION('ref_axis',(-1.04744440165294E-14,1.,-4.16203559120935E-32));
#12839=DIRECTION('',(-1.04744440165294E-14,1.,-4.16203559120935E-32));
#12840=DIRECTION('',(-1.,-1.04744440165294E-14,-4.16203559120931E-32));
#12841=DIRECTION('',(-1.04744440165294E-14,1.,-4.16203559120935E-32));
#12842=DIRECTION('',(-1.04744440165294E-14,1.,-4.16203559120935E-32));
#12843=DIRECTION('',(1.,1.04744440165294E-14,4.16203559120931E-32));
#12844=DIRECTION('',(-1.04744440165294E-14,1.,-4.16203559120935E-32));
#12845=DIRECTION('center_axis',(1.04744440165294E-14,-1.,4.16203559120935E-32));
#12846=DIRECTION('ref_axis',(4.16203559120935E-32,-4.16203559120931E-32,
-1.));
#12847=DIRECTION('',(4.16203559120935E-32,-4.16203559120931E-32,-1.));
#12848=DIRECTION('',(4.16203559120935E-32,-4.16203559120931E-32,-1.));
#12849=DIRECTION('center_axis',(-1.,-1.04744440165294E-14,-4.16203559120931E-32));
#12850=DIRECTION('ref_axis',(4.16203559120935E-32,-4.16203559120931E-32,
-1.));
#12851=DIRECTION('center_axis',(-1.,-1.04744440165294E-14,-4.16203559120931E-32));
#12852=DIRECTION('ref_axis',(4.16203559120935E-32,-4.16203559120931E-32,
-1.));
#12853=DIRECTION('center_axis',(-1.,-1.04744440165294E-14,-4.16203559120931E-32));
#12854=DIRECTION('ref_axis',(4.16203559120935E-32,-4.16203559120931E-32,
-1.));
#12855=DIRECTION('',(4.16203559120935E-32,-4.16203559120931E-32,-1.));
#12856=DIRECTION('center_axis',(-1.04744440165294E-14,1.,-4.16203559120935E-32));
#12857=DIRECTION('ref_axis',(-4.16203559120935E-32,4.16203559120931E-32,
1.));
#12858=DIRECTION('',(4.16203559120935E-32,-4.16203559120931E-32,-1.));
#12859=DIRECTION('center_axis',(-1.,-1.04744440165294E-14,-4.16203559120931E-32));
#12860=DIRECTION('ref_axis',(4.16203559120935E-32,-4.16203559120931E-32,
-1.));
#12861=DIRECTION('center_axis',(0.,0.,1.));
#12862=DIRECTION('ref_axis',(1.,0.,0.));
#12863=DIRECTION('',(0.,0.,1.));
#12864=DIRECTION('center_axis',(0.,0.,1.));
#12865=DIRECTION('ref_axis',(-1.,0.,0.));
#12866=DIRECTION('center_axis',(0.,0.,1.));
#12867=DIRECTION('ref_axis',(1.,0.,0.));
#12868=DIRECTION('',(0.,0.,1.));
#12869=DIRECTION('center_axis',(0.,0.,1.));
#12870=DIRECTION('ref_axis',(1.,0.,0.));
#12871=DIRECTION('',(0.,0.,1.));
#12872=DIRECTION('center_axis',(0.,0.,1.));
#12873=DIRECTION('ref_axis',(1.,0.,0.));
#12874=DIRECTION('',(0.,0.,1.));
#12875=DIRECTION('center_axis',(0.,0.,1.));
#12876=DIRECTION('ref_axis',(1.,0.,0.));
#12877=DIRECTION('',(0.,0.,1.));
#12878=DIRECTION('center_axis',(0.,0.,1.));
#12879=DIRECTION('ref_axis',(1.,0.,0.));
#12880=DIRECTION('',(0.,0.,1.));
#12881=DIRECTION('center_axis',(0.,0.,1.));
#12882=DIRECTION('ref_axis',(1.,0.,0.));
#12883=DIRECTION('',(0.,0.,1.));
#12884=DIRECTION('center_axis',(0.,0.,1.));
#12885=DIRECTION('ref_axis',(1.,0.,0.));
#12886=DIRECTION('',(0.,0.,1.));
#12887=DIRECTION('center_axis',(0.,0.,1.));
#12888=DIRECTION('ref_axis',(1.,0.,0.));
#12889=DIRECTION('',(0.,0.,1.));
#12890=DIRECTION('center_axis',(0.,0.,1.));
#12891=DIRECTION('ref_axis',(1.,0.,0.));
#12892=DIRECTION('',(0.,0.,1.));
#12893=DIRECTION('center_axis',(0.,0.,1.));
#12894=DIRECTION('ref_axis',(1.,0.,0.));
#12895=DIRECTION('',(0.,0.,1.));
#12896=DIRECTION('center_axis',(0.,0.,1.));
#12897=DIRECTION('ref_axis',(1.,0.,0.));
#12898=DIRECTION('',(0.,0.,1.));
#12899=DIRECTION('center_axis',(0.,0.,1.));
#12900=DIRECTION('ref_axis',(1.,0.,0.));
#12901=DIRECTION('',(0.,0.,1.));
#12902=DIRECTION('center_axis',(0.,0.,1.));
#12903=DIRECTION('ref_axis',(1.,0.,0.));
#12904=DIRECTION('',(0.,0.,1.));
#12905=DIRECTION('center_axis',(0.,0.,1.));
#12906=DIRECTION('ref_axis',(1.,0.,0.));
#12907=DIRECTION('',(0.,0.,1.));
#12908=DIRECTION('center_axis',(0.,0.,1.));
#12909=DIRECTION('ref_axis',(1.,0.,0.));
#12910=DIRECTION('',(0.,0.,1.));
#12911=DIRECTION('center_axis',(0.,0.,1.));
#12912=DIRECTION('ref_axis',(1.,0.,0.));
#12913=DIRECTION('',(0.,0.,1.));
#12914=DIRECTION('center_axis',(0.,0.,1.));
#12915=DIRECTION('ref_axis',(1.,0.,0.));
#12916=DIRECTION('',(0.,0.,1.));
#12917=DIRECTION('center_axis',(0.,0.,1.));
#12918=DIRECTION('ref_axis',(1.,0.,0.));
#12919=DIRECTION('',(0.,0.,1.));
#12920=DIRECTION('center_axis',(0.,0.,1.));
#12921=DIRECTION('ref_axis',(1.,0.,0.));
#12922=DIRECTION('',(0.,0.,1.));
#12923=DIRECTION('center_axis',(0.,0.,1.));
#12924=DIRECTION('ref_axis',(-1.,0.,0.));
#12925=DIRECTION('center_axis',(0.,0.,1.));
#12926=DIRECTION('ref_axis',(1.,0.,0.));
#12927=DIRECTION('',(0.,0.,1.));
#12928=DIRECTION('center_axis',(0.,0.,1.));
#12929=DIRECTION('ref_axis',(1.,0.,0.));
#12930=DIRECTION('',(0.,0.,1.));
#12931=DIRECTION('center_axis',(0.,0.,1.));
#12932=DIRECTION('ref_axis',(1.,0.,0.));
#12933=DIRECTION('',(0.,0.,1.));
#12934=DIRECTION('center_axis',(0.,0.,1.));
#12935=DIRECTION('ref_axis',(1.,0.,0.));
#12936=DIRECTION('',(0.,0.,1.));
#12937=DIRECTION('center_axis',(0.,0.,1.));
#12938=DIRECTION('ref_axis',(1.,0.,0.));
#12939=DIRECTION('',(0.,0.,1.));
#12940=DIRECTION('center_axis',(0.,0.,1.));
#12941=DIRECTION('ref_axis',(1.,0.,0.));
#12942=DIRECTION('',(0.,0.,1.));
#12943=DIRECTION('center_axis',(0.,0.,1.));
#12944=DIRECTION('ref_axis',(1.,0.,0.));
#12945=DIRECTION('',(0.,0.,1.));
#12946=DIRECTION('center_axis',(0.,0.,1.));
#12947=DIRECTION('ref_axis',(1.,0.,0.));
#12948=DIRECTION('',(0.,0.,1.));
#12949=DIRECTION('center_axis',(0.,0.,1.));
#12950=DIRECTION('ref_axis',(1.,0.,0.));
#12951=DIRECTION('',(0.,0.,1.));
#12952=DIRECTION('center_axis',(0.,0.,1.));
#12953=DIRECTION('ref_axis',(1.,0.,0.));
#12954=DIRECTION('',(0.,0.,1.));
#12955=DIRECTION('center_axis',(0.,0.,1.));
#12956=DIRECTION('ref_axis',(1.,0.,0.));
#12957=DIRECTION('',(0.,0.,1.));
#12958=DIRECTION('center_axis',(0.,0.,1.));
#12959=DIRECTION('ref_axis',(1.,0.,0.));
#12960=DIRECTION('',(0.,0.,1.));
#12961=DIRECTION('center_axis',(0.,0.,1.));
#12962=DIRECTION('ref_axis',(1.,0.,0.));
#12963=DIRECTION('',(0.,0.,1.));
#12964=DIRECTION('center_axis',(0.,0.,1.));
#12965=DIRECTION('ref_axis',(1.,0.,0.));
#12966=DIRECTION('',(0.,0.,1.));
#12967=DIRECTION('center_axis',(0.,0.,1.));
#12968=DIRECTION('ref_axis',(1.,0.,0.));
#12969=DIRECTION('',(0.,0.,1.));
#12970=DIRECTION('center_axis',(0.,0.,1.));
#12971=DIRECTION('ref_axis',(1.,0.,0.));
#12972=DIRECTION('',(0.,0.,1.));
#12973=DIRECTION('center_axis',(0.,0.,1.));
#12974=DIRECTION('ref_axis',(1.,0.,0.));
#12975=DIRECTION('',(0.,0.,1.));
#12976=DIRECTION('center_axis',(0.,0.,1.));
#12977=DIRECTION('ref_axis',(1.,0.,0.));
#12978=DIRECTION('',(0.,0.,1.));
#12979=DIRECTION('center_axis',(0.,0.,1.));
#12980=DIRECTION('ref_axis',(1.,0.,0.));
#12981=DIRECTION('',(0.,0.,1.));
#12982=DIRECTION('center_axis',(0.,0.,1.));
#12983=DIRECTION('ref_axis',(-1.,-7.9041468616686E-13,0.));
#12984=DIRECTION('center_axis',(0.,0.,1.));
#12985=DIRECTION('ref_axis',(1.,0.,0.));
#12986=DIRECTION('',(0.,0.,1.));
#12987=DIRECTION('center_axis',(0.,0.,1.));
#12988=DIRECTION('ref_axis',(1.,0.,0.));
#12989=DIRECTION('',(0.,0.,1.));
#12990=DIRECTION('center_axis',(0.,0.,1.));
#12991=DIRECTION('ref_axis',(1.,0.,0.));
#12992=DIRECTION('',(0.,0.,1.));
#12993=DIRECTION('center_axis',(0.,0.,1.));
#12994=DIRECTION('ref_axis',(1.,0.,0.));
#12995=DIRECTION('',(0.,0.,1.));
#12996=DIRECTION('center_axis',(0.,0.,1.));
#12997=DIRECTION('ref_axis',(1.,0.,0.));
#12998=DIRECTION('',(0.,0.,1.));
#12999=DIRECTION('center_axis',(0.,0.,1.));
#13000=DIRECTION('ref_axis',(1.,0.,0.));
#13001=DIRECTION('',(0.,0.,1.));
#13002=DIRECTION('center_axis',(0.,0.,1.));
#13003=DIRECTION('ref_axis',(1.,0.,0.));
#13004=DIRECTION('',(0.,0.,1.));
#13005=DIRECTION('center_axis',(0.,0.,1.));
#13006=DIRECTION('ref_axis',(1.,0.,0.));
#13007=DIRECTION('',(0.,0.,1.));
#13008=DIRECTION('center_axis',(0.,0.,1.));
#13009=DIRECTION('ref_axis',(1.,0.,0.));
#13010=DIRECTION('',(0.,0.,1.));
#13011=DIRECTION('center_axis',(0.,0.,1.));
#13012=DIRECTION('ref_axis',(1.,0.,0.));
#13013=DIRECTION('',(0.,0.,1.));
#13014=DIRECTION('center_axis',(0.,0.,1.));
#13015=DIRECTION('ref_axis',(1.,0.,0.));
#13016=DIRECTION('',(0.,0.,1.));
#13017=DIRECTION('center_axis',(0.,0.,1.));
#13018=DIRECTION('ref_axis',(1.,0.,0.));
#13019=DIRECTION('',(0.,0.,1.));
#13020=DIRECTION('center_axis',(0.,0.,1.));
#13021=DIRECTION('ref_axis',(1.,0.,0.));
#13022=DIRECTION('',(0.,0.,1.));
#13023=DIRECTION('center_axis',(0.,0.,1.));
#13024=DIRECTION('ref_axis',(1.,0.,0.));
#13025=DIRECTION('',(0.,0.,1.));
#13026=DIRECTION('center_axis',(0.,0.,1.));
#13027=DIRECTION('ref_axis',(1.,0.,0.));
#13028=DIRECTION('',(0.,0.,1.));
#13029=DIRECTION('center_axis',(0.,0.,1.));
#13030=DIRECTION('ref_axis',(1.,0.,0.));
#13031=DIRECTION('',(0.,0.,1.));
#13032=DIRECTION('center_axis',(0.,0.,1.));
#13033=DIRECTION('ref_axis',(1.,0.,0.));
#13034=DIRECTION('',(0.,0.,1.));
#13035=DIRECTION('center_axis',(0.,0.,1.));
#13036=DIRECTION('ref_axis',(1.,0.,0.));
#13037=DIRECTION('',(0.,0.,1.));
#13038=DIRECTION('center_axis',(0.,0.,1.));
#13039=DIRECTION('ref_axis',(1.,0.,0.));
#13040=DIRECTION('',(0.,0.,1.));
#13041=DIRECTION('center_axis',(0.,0.,1.));
#13042=DIRECTION('ref_axis',(-1.,1.82123199577617E-15,0.));
#13043=DIRECTION('center_axis',(0.,0.,1.));
#13044=DIRECTION('ref_axis',(1.,0.,0.));
#13045=DIRECTION('',(0.,0.,1.));
#13046=DIRECTION('center_axis',(0.,0.,1.));
#13047=DIRECTION('ref_axis',(1.,0.,0.));
#13048=DIRECTION('',(0.,0.,1.));
#13049=DIRECTION('center_axis',(0.,0.,1.));
#13050=DIRECTION('ref_axis',(1.,0.,0.));
#13051=DIRECTION('',(0.,0.,1.));
#13052=DIRECTION('center_axis',(0.,0.,1.));
#13053=DIRECTION('ref_axis',(1.,0.,0.));
#13054=DIRECTION('',(0.,0.,1.));
#13055=DIRECTION('center_axis',(0.,0.,1.));
#13056=DIRECTION('ref_axis',(1.,0.,0.));
#13057=DIRECTION('',(0.,0.,1.));
#13058=DIRECTION('center_axis',(0.,0.,1.));
#13059=DIRECTION('ref_axis',(1.,0.,0.));
#13060=DIRECTION('',(0.,0.,1.));
#13061=DIRECTION('center_axis',(0.,0.,1.));
#13062=DIRECTION('ref_axis',(1.,0.,0.));
#13063=DIRECTION('',(0.,0.,1.));
#13064=DIRECTION('center_axis',(0.,0.,1.));
#13065=DIRECTION('ref_axis',(1.,0.,0.));
#13066=DIRECTION('',(0.,0.,1.));
#13067=DIRECTION('center_axis',(0.,0.,1.));
#13068=DIRECTION('ref_axis',(1.,0.,0.));
#13069=DIRECTION('',(0.,0.,1.));
#13070=DIRECTION('center_axis',(0.,0.,1.));
#13071=DIRECTION('ref_axis',(1.,0.,0.));
#13072=DIRECTION('',(0.,0.,1.));
#13073=DIRECTION('center_axis',(0.,0.,1.));
#13074=DIRECTION('ref_axis',(1.,0.,0.));
#13075=DIRECTION('',(0.,0.,1.));
#13076=DIRECTION('center_axis',(0.,0.,1.));
#13077=DIRECTION('ref_axis',(1.,0.,0.));
#13078=DIRECTION('',(0.,0.,1.));
#13079=DIRECTION('center_axis',(0.,0.,1.));
#13080=DIRECTION('ref_axis',(1.,0.,0.));
#13081=DIRECTION('',(0.,0.,1.));
#13082=DIRECTION('center_axis',(0.,0.,1.));
#13083=DIRECTION('ref_axis',(1.,0.,0.));
#13084=DIRECTION('',(0.,0.,1.));
#13085=DIRECTION('center_axis',(0.,0.,1.));
#13086=DIRECTION('ref_axis',(1.,0.,0.));
#13087=DIRECTION('',(0.,0.,1.));
#13088=DIRECTION('center_axis',(0.,0.,1.));
#13089=DIRECTION('ref_axis',(1.,0.,0.));
#13090=DIRECTION('',(0.,0.,1.));
#13091=DIRECTION('center_axis',(0.,0.,1.));
#13092=DIRECTION('ref_axis',(1.,0.,0.));
#13093=DIRECTION('',(0.,0.,1.));
#13094=DIRECTION('center_axis',(0.,0.,-1.));
#13095=DIRECTION('ref_axis',(-1.14926154660527E-15,1.,0.));
#13096=DIRECTION('',(0.,0.,1.));
#13097=DIRECTION('center_axis',(0.,0.,1.));
#13098=DIRECTION('ref_axis',(-1.14926154660527E-15,1.,0.));
#13099=DIRECTION('center_axis',(0.,0.,-1.));
#13100=DIRECTION('ref_axis',(-1.14926154660527E-15,1.,0.));
#13101=DIRECTION('',(0.,0.,1.));
#13102=DIRECTION('center_axis',(0.,0.,1.));
#13103=DIRECTION('ref_axis',(-1.14926154660527E-15,1.,0.));
#13104=DIRECTION('center_axis',(0.,0.,-1.));
#13105=DIRECTION('ref_axis',(-1.14926154660527E-15,1.,0.));
#13106=DIRECTION('',(0.,0.,1.));
#13107=DIRECTION('center_axis',(0.,0.,-1.));
#13108=DIRECTION('ref_axis',(-1.14926154660527E-15,1.,0.));
#13109=DIRECTION('',(0.,0.,1.));
#13110=DIRECTION('center_axis',(0.,0.,-1.));
#13111=DIRECTION('ref_axis',(-1.14926154660527E-15,1.,0.));
#13112=DIRECTION('',(0.,0.,1.));
#13113=DIRECTION('center_axis',(0.,0.,-1.));
#13114=DIRECTION('ref_axis',(-1.14926154660527E-15,1.,0.));
#13115=DIRECTION('',(0.,0.,1.));
#13116=DIRECTION('center_axis',(0.,0.,-1.));
#13117=DIRECTION('ref_axis',(-1.14926154660527E-15,1.,0.));
#13118=DIRECTION('',(0.,0.,1.));
#13119=DIRECTION('',(0.,0.,-1.));
#13120=DIRECTION('center_axis',(0.,0.,-1.));
#13121=DIRECTION('ref_axis',(1.,8.04483082623694E-15,0.));
#13122=DIRECTION('',(0.,0.,1.));
#13123=DIRECTION('center_axis',(0.,0.,1.));
#13124=DIRECTION('ref_axis',(1.,8.04483082623694E-15,0.));
#13125=DIRECTION('center_axis',(0.,0.,-1.));
#13126=DIRECTION('ref_axis',(1.,8.04483082623694E-15,0.));
#13127=DIRECTION('',(0.,0.,1.));
#13128=DIRECTION('center_axis',(0.,0.,1.));
#13129=DIRECTION('ref_axis',(1.,8.04483082623694E-15,0.));
#13130=DIRECTION('center_axis',(0.,0.,-1.));
#13131=DIRECTION('ref_axis',(1.,8.04483082623694E-15,0.));
#13132=DIRECTION('',(0.,0.,1.));
#13133=DIRECTION('center_axis',(0.,0.,-1.));
#13134=DIRECTION('ref_axis',(1.,8.04483082623694E-15,0.));
#13135=DIRECTION('',(0.,0.,1.));
#13136=DIRECTION('center_axis',(0.,0.,-1.));
#13137=DIRECTION('ref_axis',(1.,8.04483082623694E-15,0.));
#13138=DIRECTION('',(0.,0.,1.));
#13139=DIRECTION('center_axis',(0.,0.,-1.));
#13140=DIRECTION('ref_axis',(1.,8.04483082623694E-15,0.));
#13141=DIRECTION('',(0.,0.,1.));
#13142=DIRECTION('center_axis',(0.,0.,-1.));
#13143=DIRECTION('ref_axis',(1.,8.04483082623694E-15,0.));
#13144=DIRECTION('',(0.,0.,1.));
#13145=DIRECTION('',(0.,0.,-1.));
#13146=DIRECTION('center_axis',(0.,0.,-1.));
#13147=DIRECTION('ref_axis',(1.14926154660527E-15,-1.,0.));
#13148=DIRECTION('',(0.,0.,1.));
#13149=DIRECTION('center_axis',(0.,0.,1.));
#13150=DIRECTION('ref_axis',(1.14926154660527E-15,-1.,0.));
#13151=DIRECTION('center_axis',(0.,0.,-1.));
#13152=DIRECTION('ref_axis',(1.14926154660527E-15,-1.,0.));
#13153=DIRECTION('',(0.,0.,1.));
#13154=DIRECTION('center_axis',(0.,0.,1.));
#13155=DIRECTION('ref_axis',(1.14926154660527E-15,-1.,0.));
#13156=DIRECTION('center_axis',(0.,0.,-1.));
#13157=DIRECTION('ref_axis',(1.14926154660527E-15,-1.,0.));
#13158=DIRECTION('',(0.,0.,1.));
#13159=DIRECTION('center_axis',(0.,0.,-1.));
#13160=DIRECTION('ref_axis',(1.14926154660527E-15,-1.,0.));
#13161=DIRECTION('',(0.,0.,1.));
#13162=DIRECTION('center_axis',(0.,0.,-1.));
#13163=DIRECTION('ref_axis',(1.14926154660527E-15,-1.,0.));
#13164=DIRECTION('',(0.,0.,1.));
#13165=DIRECTION('center_axis',(0.,0.,-1.));
#13166=DIRECTION('ref_axis',(1.14926154660527E-15,-1.,0.));
#13167=DIRECTION('',(0.,0.,1.));
#13168=DIRECTION('center_axis',(0.,0.,-1.));
#13169=DIRECTION('ref_axis',(1.14926154660527E-15,-1.,0.));
#13170=DIRECTION('',(0.,0.,1.));
#13171=DIRECTION('',(0.,0.,-1.));
#13172=DIRECTION('center_axis',(0.,0.,-1.));
#13173=DIRECTION('ref_axis',(-1.,0.,0.));
#13174=DIRECTION('',(0.,0.,1.));
#13175=DIRECTION('center_axis',(0.,0.,1.));
#13176=DIRECTION('ref_axis',(-1.,0.,0.));
#13177=DIRECTION('center_axis',(0.,0.,-1.));
#13178=DIRECTION('ref_axis',(-1.,0.,0.));
#13179=DIRECTION('',(0.,0.,1.));
#13180=DIRECTION('center_axis',(0.,0.,1.));
#13181=DIRECTION('ref_axis',(-1.,0.,0.));
#13182=DIRECTION('center_axis',(0.,0.,-1.));
#13183=DIRECTION('ref_axis',(-1.,0.,0.));
#13184=DIRECTION('',(0.,0.,1.));
#13185=DIRECTION('center_axis',(0.,0.,-1.));
#13186=DIRECTION('ref_axis',(-1.,0.,0.));
#13187=DIRECTION('',(0.,0.,1.));
#13188=DIRECTION('center_axis',(0.,0.,-1.));
#13189=DIRECTION('ref_axis',(-1.,0.,0.));
#13190=DIRECTION('',(0.,0.,1.));
#13191=DIRECTION('center_axis',(0.,0.,-1.));
#13192=DIRECTION('ref_axis',(-1.,0.,0.));
#13193=DIRECTION('',(0.,0.,1.));
#13194=DIRECTION('center_axis',(0.,0.,-1.));
#13195=DIRECTION('ref_axis',(-1.,0.,0.));
#13196=DIRECTION('',(0.,0.,1.));
#13197=DIRECTION('',(0.,0.,-1.));
#13198=DIRECTION('center_axis',(0.,0.,-1.));
#13199=DIRECTION('ref_axis',(-1.,0.,0.));
#13200=DIRECTION('center_axis',(0.,0.,-1.));
#13201=DIRECTION('ref_axis',(1.14926154660527E-15,-1.,0.));
#13202=DIRECTION('center_axis',(0.,0.,-1.));
#13203=DIRECTION('ref_axis',(1.,8.04483082623694E-15,0.));
#13204=DIRECTION('center_axis',(0.,0.,-1.));
#13205=DIRECTION('ref_axis',(-1.14926154660527E-15,1.,0.));
#13206=DIRECTION('center_axis',(0.,0.,1.));
#13207=DIRECTION('ref_axis',(1.,0.,0.));
#13208=DIRECTION('center_axis',(0.,0.,1.));
#13209=DIRECTION('ref_axis',(-1.,-5.46369598732852E-15,0.));
#13210=DIRECTION('center_axis',(0.,0.,1.));
#13211=DIRECTION('ref_axis',(1.,0.,0.));
#13212=DIRECTION('center_axis',(0.,0.,1.));
#13213=DIRECTION('ref_axis',(-1.,-3.64246399155235E-15,0.));
#13214=DIRECTION('center_axis',(0.,0.,1.));
#13215=DIRECTION('ref_axis',(1.,0.,0.));
#13216=DIRECTION('center_axis',(0.,0.,1.));
#13217=DIRECTION('ref_axis',(-1.,1.82123199577617E-15,0.));
#13218=DIRECTION('center_axis',(0.,0.,1.));
#13219=DIRECTION('ref_axis',(1.,0.,0.));
#13220=DIRECTION('center_axis',(0.,0.,1.));
#13221=DIRECTION('ref_axis',(-1.,-9.10615997888087E-16,0.));
#13222=DIRECTION('center_axis',(0.,0.,1.));
#13223=DIRECTION('ref_axis',(1.,0.,0.));
#13224=DIRECTION('center_axis',(0.,0.,1.));
#13225=DIRECTION('ref_axis',(-1.,0.,0.));
#13226=DIRECTION('',(0.,0.,1.));
#13227=DIRECTION('center_axis',(0.,0.,-1.));
#13228=DIRECTION('ref_axis',(1.,0.,0.));
#13229=DIRECTION('center_axis',(0.,0.,1.));
#13230=DIRECTION('ref_axis',(1.,0.,0.));
#13231=DIRECTION('center_axis',(0.,0.,1.));
#13232=DIRECTION('ref_axis',(1.,0.,0.));
#13233=DIRECTION('',(0.,0.,1.));
#13234=DIRECTION('center_axis',(0.,0.,1.));
#13235=DIRECTION('ref_axis',(1.,0.,0.));
#13236=DIRECTION('center_axis',(0.,0.,-1.));
#13237=DIRECTION('ref_axis',(-1.,0.,0.));
#13238=DIRECTION('center_axis',(0.,0.,-1.));
#13239=DIRECTION('ref_axis',(-1.,0.,0.));
#13240=DIRECTION('',(-0.707106781186555,8.65956056235503E-17,0.70710678118654));
#13241=DIRECTION('center_axis',(0.,0.,1.));
#13242=DIRECTION('ref_axis',(-1.,0.,0.));
#13243=DIRECTION('center_axis',(0.,0.,-1.));
#13244=DIRECTION('ref_axis',(-1.,0.,0.));
#13245=DIRECTION('',(0.,0.,1.));
#13246=DIRECTION('center_axis',(0.,0.,1.));
#13247=DIRECTION('ref_axis',(1.,0.,0.));
#13248=DIRECTION('center_axis',(4.16203559120935E-32,4.16203559120936E-32,
1.));
#13249=DIRECTION('ref_axis',(-3.21990436376205E-15,1.,-4.16203559120935E-32));
#13250=DIRECTION('center_axis',(9.19047099336175E-15,3.40905954562136E-15,
1.));
#13251=DIRECTION('ref_axis',(0.596254243270102,0.802795663529891,-8.21663554738274E-15));
#13252=DIRECTION('',(2.36341181601185E-15,-0.707106781186549,0.707106781186546));
#13253=DIRECTION('center_axis',(0.,0.,-1.));
#13254=DIRECTION('ref_axis',(-1.,0.,0.));
#13255=DIRECTION('center_axis',(0.,8.3240711824187E-32,1.));
#13256=DIRECTION('ref_axis',(-1.,0.,0.));
#13257=DIRECTION('center_axis',(0.,0.,1.));
#13258=DIRECTION('ref_axis',(-0.802795663529893,0.5962542432701,0.));
#13259=DIRECTION('',(0.707106781186549,8.65956056235496E-17,0.707106781186546));
#13260=DIRECTION('center_axis',(0.,0.,-1.));
#13261=DIRECTION('ref_axis',(-1.,0.,0.));
#13262=DIRECTION('center_axis',(-4.16203559120935E-32,4.16203559120931E-32,
1.));
#13263=DIRECTION('ref_axis',(1.04646891822267E-14,-1.,4.16203559120935E-32));
#13264=DIRECTION('center_axis',(9.19047099336175E-15,3.40905954562148E-15,
1.));
#13265=DIRECTION('ref_axis',(-0.596254243270094,-0.802795663529897,8.21663554738278E-15));
#13266=DIRECTION('',(-7.48624828938557E-15,0.707106781186549,0.707106781186546));
#13267=DIRECTION('center_axis',(0.,0.,-1.));
#13268=DIRECTION('ref_axis',(-1.,0.,0.));
#13269=DIRECTION('center_axis',(0.,0.,1.));
#13270=DIRECTION('ref_axis',(1.,0.,0.));
#13271=DIRECTION('center_axis',(0.,0.,1.));
#13272=DIRECTION('ref_axis',(0.802795663529893,-0.5962542432701,0.));
#13273=DIRECTION('',(-0.707106781186549,-8.65956056235495E-17,0.707106781186546));
#13274=DIRECTION('center_axis',(0.,0.,-1.));
#13275=DIRECTION('ref_axis',(-1.,0.,0.));
#13276=DIRECTION('center_axis',(2.88512032359387E-6,-9.62952063919659E-7,
-0.999999999995374));
#13277=DIRECTION('ref_axis',(-0.910167431629583,0.414240565845088,-3.02483636272151E-6));
#13278=DIRECTION('',(0.509030150079891,0.700633705437601,0.500000717113906));
#13279=DIRECTION('center_axis',(-5.73319914530485E-6,1.03122865517202E-5,
-0.999999999930394));
#13280=DIRECTION('ref_axis',(-0.400826900807492,0.916153805564928,1.17456610143768E-5));
#13281=DIRECTION('',(-0.509034825310574,-0.700630697427327,0.500000172443501));
#13282=DIRECTION('center_axis',(-0.809020620080864,0.587780261877828,-5.55040215556246E-6));
#13283=DIRECTION('ref_axis',(-0.587780261886882,-0.809020620093325,3.00207577931475E-21));
#13284=DIRECTION('',(-4.49056928125163E-6,3.26216978819017E-6,0.999999999984597));
#13285=DIRECTION('center_axis',(0.,0.,1.));
#13286=DIRECTION('ref_axis',(1.,0.,0.));
#13287=DIRECTION('',(-1.,1.63653158111019E-16,0.));
#13288=DIRECTION('',(-0.707106781186551,0.707106781186544,0.));
#13289=DIRECTION('',(3.27306316222039E-16,1.,0.));
#13290=DIRECTION('',(0.707106781186551,0.707106781186544,0.));
#13291=DIRECTION('',(-1.,-1.63653158111019E-16,0.));
#13292=DIRECTION('',(0.707106781186551,-0.707106781186544,0.));
#13293=DIRECTION('',(0.,-1.,0.));
#13294=DIRECTION('',(-0.707106781186551,-0.707106781186544,0.));
#13295=DIRECTION('center_axis',(9.62952046063973E-7,2.88512025876916E-6,
-0.999999999995374));
#13296=DIRECTION('ref_axis',(-0.414240565845042,-0.910167431629604,-3.02483629632364E-6));
#13297=DIRECTION('center_axis',(-1.03122864674752E-5,-5.73319909310356E-6,
-0.999999999930394));
#13298=DIRECTION('ref_axis',(-0.916153805570372,-0.40082690079505,1.17456609162565E-5));
#13299=DIRECTION('center_axis',(-2.88512008141766E-6,9.62951976338086E-7,
-0.999999999995374));
#13300=DIRECTION('ref_axis',(0.910167431629613,-0.414240565845021,-3.0248361060208E-6));
#13301=DIRECTION('center_axis',(5.73319910393675E-6,-1.03122864820549E-5,
-0.999999999930394));
#13302=DIRECTION('ref_axis',(0.400826900807403,-0.916153805564967,1.17456609339711E-5));
#13303=DIRECTION('center_axis',(-9.62952042711932E-7,-2.88512027353277E-6,
-0.999999999995374));
#13304=DIRECTION('ref_axis',(0.41424056584503,0.910167431629609,-3.02483630837245E-6));
#13305=DIRECTION('center_axis',(1.0312286495339E-5,5.73319911396724E-6,
-0.999999999930394));
#13306=DIRECTION('ref_axis',(0.916153805564476,0.400826900808526,1.17456609501632E-5));
#13307=DIRECTION('',(0.700633705437605,-0.509030150079883,0.500000717113908));
#13308=DIRECTION('',(-0.700630697427374,0.509034825310594,0.500000172443415));
#13309=DIRECTION('center_axis',(0.58778026187782,0.80902062008087,-5.55040215556246E-6));
#13310=DIRECTION('ref_axis',(-0.809020620093331,0.587780261886873,-9.35224649526989E-22));
#13311=DIRECTION('',(3.26216982371735E-6,4.49056924572438E-6,0.999999999984597));
#13312=DIRECTION('',(-0.509030150079891,-0.700633705437601,0.500000717113906));
#13313=DIRECTION('',(0.509034825310574,0.700630697427327,0.500000172443501));
#13314=DIRECTION('center_axis',(0.809020620080864,-0.587780261877828,-5.55040215556246E-6));
#13315=DIRECTION('ref_axis',(0.587780261886882,0.809020620093325,3.00207577931475E-21));
#13316=DIRECTION('',(4.49056928125163E-6,-3.26216978819017E-6,0.999999999984597));
#13317=DIRECTION('',(-0.700633705437603,0.509030150079887,0.500000717113907));
#13318=DIRECTION('',(0.700630697427361,-0.509034825310594,0.500000172443434));
#13319=DIRECTION('center_axis',(-0.587780261877825,-0.809020620080866,-5.55040215556247E-6));
#13320=DIRECTION('ref_axis',(0.809020620093328,-0.587780261886879,3.26781804448781E-21));
#13321=DIRECTION('',(-3.26216982371737E-6,-4.4905692457244E-6,0.999999999984597));
#13322=DIRECTION('center_axis',(0.,0.,1.));
#13323=DIRECTION('ref_axis',(1.,0.,0.));
#13324=DIRECTION('center_axis',(0.,0.,1.));
#13325=DIRECTION('ref_axis',(1.,0.,0.));
#13326=DIRECTION('center_axis',(0.707106781186544,-0.707106781186551,0.));
#13327=DIRECTION('ref_axis',(0.707106781186551,0.707106781186544,0.));
#13328=DIRECTION('',(0.,0.,-1.));
#13329=DIRECTION('',(0.707106781186551,0.707106781186544,0.));
#13330=DIRECTION('',(0.,0.,-1.));
#13331=DIRECTION('center_axis',(1.,1.02283223819387E-16,0.));
#13332=DIRECTION('ref_axis',(-1.02283223819387E-16,1.,0.));
#13333=DIRECTION('',(0.,0.,-1.));
#13334=DIRECTION('',(-1.02283223819387E-16,1.,0.));
#13335=DIRECTION('center_axis',(-0.707106781186551,-0.707106781186544,0.));
#13336=DIRECTION('ref_axis',(0.707106781186544,-0.707106781186551,0.));
#13337=DIRECTION('center_axis',(0.382683432365102,0.923879532511282,1.23463181525019E-15));
#13338=DIRECTION('ref_axis',(0.923879532511282,-0.382683432365102,-1.12630623213688E-12));
#13339=DIRECTION('',(-0.707106781186551,-0.707106781186544,0.));
#13340=DIRECTION('center_axis',(0.923879532511286,0.382683432365093,-1.27204490056077E-15));
#13341=DIRECTION('ref_axis',(0.382683432365093,-0.923879532511286,2.44180953280602E-12));
#13342=DIRECTION('center_axis',(0.,-1.,0.));
#13343=DIRECTION('ref_axis',(0.,0.,-1.));
#13344=DIRECTION('',(1.,0.,0.));
#13345=DIRECTION('',(0.,0.,-1.));
#13346=DIRECTION('center_axis',(0.707106781186544,0.707106781186551,0.));
#13347=DIRECTION('ref_axis',(-0.707106781186551,0.707106781186544,0.));
#13348=DIRECTION('',(0.,0.,-1.));
#13349=DIRECTION('',(-0.707106781186551,0.707106781186544,0.));
#13350=DIRECTION('center_axis',(1.02283223819387E-16,-1.,0.));
#13351=DIRECTION('ref_axis',(1.,1.02283223819387E-16,0.));
#13352=DIRECTION('center_axis',(-0.382683432365102,0.923879532511282,-4.48957023727334E-16));
#13353=DIRECTION('ref_axis',(0.923879532511282,0.382683432365102,2.16580847215386E-12));
#13354=DIRECTION('',(1.02283223819387E-16,-1.,0.));
#13355=DIRECTION('center_axis',(-2.04566447638774E-16,1.,0.));
#13356=DIRECTION('ref_axis',(-1.,-2.04566447638774E-16,0.));
#13357=DIRECTION('',(0.,0.,-1.));
#13358=DIRECTION('',(-1.,-2.04566447638774E-16,0.));
#13359=DIRECTION('center_axis',(0.707106781186551,-0.707106781186544,0.));
#13360=DIRECTION('ref_axis',(0.707106781186544,0.707106781186551,0.));
#13361=DIRECTION('center_axis',(0.923879532511285,-0.382683432365095,4.56439640789447E-15));
#13362=DIRECTION('ref_axis',(0.382683432365095,0.923879532511285,-1.55608578712059E-12));
#13363=DIRECTION('',(0.707106781186551,-0.707106781186544,0.));
#13364=DIRECTION('center_axis',(-0.707106781186544,0.707106781186551,0.));
#13365=DIRECTION('ref_axis',(-0.707106781186551,-0.707106781186544,0.));
#13366=DIRECTION('',(0.,0.,-1.));
#13367=DIRECTION('',(-0.707106781186551,-0.707106781186544,0.));
#13368=DIRECTION('center_axis',(1.,2.04566447638774E-16,0.));
#13369=DIRECTION('ref_axis',(-2.04566447638774E-16,1.,0.));
#13370=DIRECTION('center_axis',(0.923879532511291,0.382683432365081,1.79582809490932E-14));
#13371=DIRECTION('ref_axis',(0.382683432365081,-0.92387953251129,-4.11849825226955E-13));
#13372=DIRECTION('',(1.,2.04566447638774E-16,0.));
#13373=DIRECTION('center_axis',(-1.,0.,0.));
#13374=DIRECTION('ref_axis',(0.,0.,1.));
#13375=DIRECTION('',(0.,0.,-1.));
#13376=DIRECTION('',(0.,-1.,0.));
#13377=DIRECTION('center_axis',(0.707106781186551,0.707106781186544,0.));
#13378=DIRECTION('ref_axis',(-0.707106781186544,0.707106781186551,0.));
#13379=DIRECTION('center_axis',(0.382683432365092,0.923879532511286,-1.31694060293351E-14));
#13380=DIRECTION('ref_axis',(0.923879532511286,-0.382683432365092,-1.05940768985082E-12));
#13381=DIRECTION('',(0.707106781186551,0.707106781186544,0.));
#13382=DIRECTION('center_axis',(-0.707106781186544,-0.707106781186551,0.));
#13383=DIRECTION('ref_axis',(0.707106781186551,-0.707106781186544,0.));
#13384=DIRECTION('',(0.707106781186551,-0.707106781186544,0.));
#13385=DIRECTION('center_axis',(0.,1.,0.));
#13386=DIRECTION('ref_axis',(0.,0.,1.));
#13387=DIRECTION('center_axis',(-0.382683432365094,0.923879532511285,8.45535728019809E-15));
#13388=DIRECTION('ref_axis',(0.923879532511285,0.382683432365094,-2.63399123634393E-12));
#13389=DIRECTION('',(0.,1.,0.));
#13390=DIRECTION('center_axis',(-0.707106781186551,0.707106781186544,0.));
#13391=DIRECTION('ref_axis',(-0.707106781186544,-0.707106781186551,0.));
#13392=DIRECTION('center_axis',(0.923879532511292,-0.382683432365078,1.6162452854184E-14));
#13393=DIRECTION('ref_axis',(0.382683432365078,0.923879532511292,-1.85973161387526E-12));
#13394=DIRECTION('',(-0.707106781186551,0.707106781186544,0.));
#13395=DIRECTION('center_axis',(-1.,0.,0.));
#13396=DIRECTION('ref_axis',(0.,0.,1.));
#13397=DIRECTION('',(-1.,0.,0.));
#13398=DIRECTION('center_axis',(0.,0.,-1.));
#13399=DIRECTION('ref_axis',(-1.,0.,0.));
#13400=DIRECTION('center_axis',(0.,0.,-1.));
#13401=DIRECTION('ref_axis',(-1.,0.,0.));
#13402=DIRECTION('',(-0.707106781186547,8.65956056235493E-17,0.707106781186548));
#13403=DIRECTION('center_axis',(0.,0.,-1.));
#13404=DIRECTION('ref_axis',(1.,-8.88178419700125E-16,0.));
#13405=DIRECTION('center_axis',(0.,0.,1.));
#13406=DIRECTION('ref_axis',(1.,0.,0.));
#13407=DIRECTION('center_axis',(0.,0.,-1.));
#13408=DIRECTION('ref_axis',(-1.,0.,0.));
#13409=DIRECTION('center_axis',(0.,0.,1.));
#13410=DIRECTION('ref_axis',(1.,0.,0.));
#13411=DIRECTION('center_axis',(0.,0.,-1.));
#13412=DIRECTION('ref_axis',(1.,-8.88178419700125E-16,0.));
#13413=DIRECTION('center_axis',(0.,0.,1.));
#13414=DIRECTION('ref_axis',(1.,0.,0.));
#13415=DIRECTION('',(-0.707106781186549,-8.65956056235495E-17,0.707106781186546));
#13416=DIRECTION('center_axis',(0.,0.,1.));
#13417=DIRECTION('ref_axis',(1.,0.,0.));
#13418=DIRECTION('center_axis',(0.,0.,-1.));
#13419=DIRECTION('ref_axis',(-1.,0.,0.));
#13420=DIRECTION('center_axis',(0.,0.,1.));
#13421=DIRECTION('ref_axis',(-1.,0.,0.));
#13422=DIRECTION('',(0.,0.,1.));
#13423=DIRECTION('',(0.,0.,-1.));
#13424=DIRECTION('center_axis',(0.,0.,-1.));
#13425=DIRECTION('ref_axis',(-1.,0.,0.));
#13426=DIRECTION('',(0.,0.,1.));
#13427=DIRECTION('center_axis',(0.,0.,1.));
#13428=DIRECTION('ref_axis',(1.,0.,0.));
#13429=DIRECTION('center_axis',(0.,0.,-1.));
#13430=DIRECTION('ref_axis',(-1.,0.,0.));
#13431=DIRECTION('center_axis',(0.,0.,-1.));
#13432=DIRECTION('ref_axis',(-1.,0.,0.));
#13433=DIRECTION('',(1.,0.,0.));
#13434=DIRECTION('center_axis',(0.,-1.,0.));
#13435=DIRECTION('ref_axis',(0.,0.,-1.));
#13436=DIRECTION('center_axis',(0.,0.,-1.));
#13437=DIRECTION('ref_axis',(-1.,0.,0.));
#13438=DIRECTION('center_axis',(0.,0.,-1.));
#13439=DIRECTION('ref_axis',(-1.,0.,0.));
#13440=DIRECTION('',(0.,0.,-1.));
#13441=DIRECTION('center_axis',(0.,0.,-1.));
#13442=DIRECTION('ref_axis',(-1.,0.,0.));
#13443=DIRECTION('center_axis',(0.,0.,-1.));
#13444=DIRECTION('ref_axis',(-1.,0.,0.));
#13445=DIRECTION('center_axis',(0.,0.,-1.));
#13446=DIRECTION('ref_axis',(-1.,0.,0.));
#13447=DIRECTION('',(0.707106781186532,-8.65956056235475E-17,-0.707106781186563));
#13448=DIRECTION('center_axis',(0.,0.,1.));
#13449=DIRECTION('ref_axis',(-1.,0.,0.));
#13450=DIRECTION('center_axis',(0.,0.,-1.));
#13451=DIRECTION('ref_axis',(-1.,0.,0.));
#13452=DIRECTION('center_axis',(0.,0.,-1.));
#13453=DIRECTION('ref_axis',(-1.,0.,0.));
#13454=DIRECTION('',(0.707106781186532,-8.65956056235475E-17,-0.707106781186563));
#13455=DIRECTION('center_axis',(0.,0.,1.));
#13456=DIRECTION('ref_axis',(-1.,0.,0.));
#13457=DIRECTION('center_axis',(0.,0.,-1.));
#13458=DIRECTION('ref_axis',(-1.,0.,0.));
#13459=DIRECTION('center_axis',(0.,0.,-1.));
#13460=DIRECTION('ref_axis',(-1.,0.,0.));
#13461=DIRECTION('',(0.707106781186532,-8.65956056235475E-17,-0.707106781186563));
#13462=DIRECTION('center_axis',(0.,0.,1.));
#13463=DIRECTION('ref_axis',(-1.,0.,0.));
#13464=DIRECTION('center_axis',(0.,0.,-1.));
#13465=DIRECTION('ref_axis',(-1.,0.,0.));
#13466=DIRECTION('center_axis',(0.,0.,-1.));
#13467=DIRECTION('ref_axis',(-1.,0.,0.));
#13468=DIRECTION('',(0.707106781186532,-8.65956056235475E-17,-0.707106781186563));
#13469=DIRECTION('center_axis',(0.,0.,1.));
#13470=DIRECTION('ref_axis',(-1.,0.,0.));
#13471=DIRECTION('center_axis',(0.,0.,-1.));
#13472=DIRECTION('ref_axis',(-1.,0.,0.));
#13473=DIRECTION('center_axis',(0.,0.,-1.));
#13474=DIRECTION('ref_axis',(-1.,0.,0.));
#13475=DIRECTION('',(0.,0.,-1.));
#13476=DIRECTION('center_axis',(0.,0.,-1.));
#13477=DIRECTION('ref_axis',(-1.,0.,0.));
#13478=DIRECTION('center_axis',(0.,0.,-1.));
#13479=DIRECTION('ref_axis',(-1.,0.,0.));
#13480=DIRECTION('',(0.,0.,-1.));
#13481=DIRECTION('center_axis',(0.,0.,-1.));
#13482=DIRECTION('ref_axis',(-1.,0.,0.));
#13483=DIRECTION('center_axis',(0.,0.,-1.));
#13484=DIRECTION('ref_axis',(-1.,0.,0.));
#13485=DIRECTION('',(0.,0.,-1.));
#13486=DIRECTION('center_axis',(0.,0.,-1.));
#13487=DIRECTION('ref_axis',(-1.,0.,0.));
#13488=DIRECTION('center_axis',(0.,0.,-1.));
#13489=DIRECTION('ref_axis',(-1.,0.,0.));
#13490=DIRECTION('',(0.,0.,-1.));
#13491=DIRECTION('center_axis',(0.,0.,1.));
#13492=DIRECTION('ref_axis',(1.,0.,0.));
#13493=DIRECTION('center_axis',(0.,0.,1.));
#13494=DIRECTION('ref_axis',(-1.,0.,0.));
#13495=DIRECTION('',(0.,0.,1.));
#13496=DIRECTION('center_axis',(0.,0.,-1.));
#13497=DIRECTION('ref_axis',(1.,0.,0.));
#13498=DIRECTION('center_axis',(0.,0.,-1.));
#13499=DIRECTION('ref_axis',(-1.,0.,0.));
#13500=DIRECTION('center_axis',(0.,0.,-1.));
#13501=DIRECTION('ref_axis',(-1.,0.,0.));
#13502=DIRECTION('center_axis',(0.,0.,-1.));
#13503=DIRECTION('ref_axis',(-1.,0.,0.));
#13504=DIRECTION('center_axis',(0.,0.,-1.));
#13505=DIRECTION('ref_axis',(-1.,0.,0.));
#13506=DIRECTION('center_axis',(0.,1.,0.));
#13507=DIRECTION('ref_axis',(0.,0.,1.));
#13508=DIRECTION('',(1.,0.,0.));
#13509=DIRECTION('',(0.,0.,-1.));
#13510=DIRECTION('',(-1.,0.,0.));
#13511=DIRECTION('',(2.64713952874444E-16,0.,1.));
#13512=DIRECTION('center_axis',(0.,0.,-1.));
#13513=DIRECTION('ref_axis',(-1.,0.,0.));
#13514=DIRECTION('',(-1.,0.,0.));
#13515=DIRECTION('',(0.,1.,0.));
#13516=DIRECTION('',(0.,1.,0.));
#13517=DIRECTION('center_axis',(-1.,0.,2.64713952874444E-16));
#13518=DIRECTION('ref_axis',(2.64713952874444E-16,0.,1.));
#13519=DIRECTION('',(2.64713952874444E-16,0.,1.));
#13520=DIRECTION('',(0.,1.,0.));
#13521=DIRECTION('center_axis',(0.,0.,1.));
#13522=DIRECTION('ref_axis',(1.,0.,0.));
#13523=DIRECTION('',(1.,0.,0.));
#13524=DIRECTION('',(0.,1.,0.));
#13525=DIRECTION('center_axis',(1.,0.,0.));
#13526=DIRECTION('ref_axis',(0.,0.,-1.));
#13527=DIRECTION('',(0.,0.,-1.));
#13528=DIRECTION('center_axis',(0.,-1.,0.));
#13529=DIRECTION('ref_axis',(0.,0.,-1.));
#13530=DIRECTION('',(0.,0.,-1.));
#13531=DIRECTION('',(-1.,0.,0.));
#13532=DIRECTION('',(1.90771507937448E-16,0.,1.));
#13533=DIRECTION('',(1.,0.,0.));
#13534=DIRECTION('center_axis',(0.,0.,1.));
#13535=DIRECTION('ref_axis',(1.,0.,0.));
#13536=DIRECTION('',(0.,-1.,0.));
#13537=DIRECTION('',(-1.,0.,0.));
#13538=DIRECTION('',(0.,-1.,0.));
#13539=DIRECTION('center_axis',(0.,0.,-1.));
#13540=DIRECTION('ref_axis',(-1.,0.,0.));
#13541=DIRECTION('',(-1.,-2.04566447638774E-16,0.));
#13542=DIRECTION('',(-0.707106781186551,0.707106781186544,0.));
#13543=DIRECTION('',(-1.02283223819387E-16,1.,0.));
#13544=DIRECTION('',(0.707106781186551,0.707106781186544,0.));
#13545=DIRECTION('',(1.,0.,0.));
#13546=DIRECTION('',(0.707106781186551,-0.707106781186544,0.));
#13547=DIRECTION('',(0.,-1.,0.));
#13548=DIRECTION('',(-0.707106781186551,-0.707106781186544,0.));
#13549=DIRECTION('center_axis',(0.707106781186551,0.707106781186544,0.));
#13550=DIRECTION('ref_axis',(-0.707106781186544,0.707106781186551,0.));
#13551=DIRECTION('center_axis',(-0.923879532511288,-0.382683432365087,-4.48957023727335E-16));
#13552=DIRECTION('ref_axis',(0.382683432365087,-0.923879532511288,-3.69328470883498E-12));
#13553=DIRECTION('center_axis',(-0.382683432365071,-0.923879532511295,2.72741391914358E-14));
#13554=DIRECTION('ref_axis',(0.923879532511295,-0.382683432365071,-5.58285843927778E-12));
#13555=DIRECTION('',(-0.707106781186551,-0.707106781186544,0.));
#13556=DIRECTION('center_axis',(-1.02283223819387E-16,1.,0.));
#13557=DIRECTION('ref_axis',(-1.,-1.02283223819387E-16,0.));
#13558=DIRECTION('center_axis',(0.382683432365102,-0.923879532511282,-4.48957023727337E-16));
#13559=DIRECTION('ref_axis',(0.923879532511282,0.382683432365102,-3.82113308819835E-12));
#13560=DIRECTION('',(1.02283223819387E-16,-1.,0.));
#13561=DIRECTION('center_axis',(-0.707106781186551,0.707106781186544,0.));
#13562=DIRECTION('ref_axis',(-0.707106781186544,-0.707106781186551,0.));
#13563=DIRECTION('center_axis',(-0.923879532511285,0.382683432365094,2.39443745987918E-15));
#13564=DIRECTION('ref_axis',(0.382683432365094,0.923879532511285,-7.29302575246149E-12));
#13565=DIRECTION('',(0.707106781186551,-0.707106781186544,0.));
#13566=DIRECTION('center_axis',(1.,1.02283223819387E-16,0.));
#13567=DIRECTION('ref_axis',(-1.02283223819387E-16,1.,0.));
#13568=DIRECTION('',(0.,0.,-1.));
#13569=DIRECTION('',(0.,0.,-1.));
#13570=DIRECTION('',(0.,-1.,0.));
#13571=DIRECTION('center_axis',(-1.,-2.04566447638774E-16,0.));
#13572=DIRECTION('ref_axis',(2.04566447638774E-16,-1.,0.));
#13573=DIRECTION('center_axis',(-0.923879532511293,-0.382683432365076,1.27204490056078E-14));
#13574=DIRECTION('ref_axis',(0.382683432365076,-0.923879532511293,1.41474115456993E-12));
#13575=DIRECTION('',(1.,2.04566447638774E-16,0.));
#13576=DIRECTION('center_axis',(0.707106781186544,0.707106781186551,0.));
#13577=DIRECTION('ref_axis',(-0.707106781186551,0.707106781186544,0.));
#13578=DIRECTION('',(0.,0.,-1.));
#13579=DIRECTION('',(0.707106781186551,-0.707106781186544,0.));
#13580=DIRECTION('center_axis',(-0.707106781186551,-0.707106781186544,0.));
#13581=DIRECTION('ref_axis',(0.707106781186544,-0.707106781186551,0.));
#13582=DIRECTION('center_axis',(-0.382683432365091,-0.923879532511286,-5.83644130845536E-15));
#13583=DIRECTION('ref_axis',(0.923879532511286,-0.382683432365091,1.78782837061874E-12));
#13584=DIRECTION('',(0.707106781186551,0.707106781186544,0.));
#13585=DIRECTION('center_axis',(-2.04566447638774E-16,1.,0.));
#13586=DIRECTION('ref_axis',(-1.,-2.04566447638774E-16,0.));
#13587=DIRECTION('',(0.,0.,-1.));
#13588=DIRECTION('',(-1.,-1.63653158111019E-16,0.));
#13589=DIRECTION('center_axis',(0.,-1.,0.));
#13590=DIRECTION('ref_axis',(0.,0.,-1.));
#13591=DIRECTION('center_axis',(0.382683432365094,-0.923879532511285,8.45535728019803E-15));
#13592=DIRECTION('ref_axis',(0.923879532511285,0.382683432365094,-1.28017687415757E-12));
#13593=DIRECTION('',(0.,1.,0.));
#13594=DIRECTION('center_axis',(-0.707106781186544,0.707106781186551,0.));
#13595=DIRECTION('ref_axis',(-0.707106781186551,-0.707106781186544,0.));
#13596=DIRECTION('',(0.,0.,-1.));
#13597=DIRECTION('',(0.707106781186551,0.707106781186544,0.));
#13598=DIRECTION('center_axis',(0.707106781186551,-0.707106781186544,0.));
#13599=DIRECTION('ref_axis',(0.707106781186544,0.707106781186551,0.));
#13600=DIRECTION('center_axis',(-0.923879532511291,0.382683432365079,1.50400602948654E-14));
#13601=DIRECTION('ref_axis',(0.382683432365079,0.923879532511291,-1.73217448820192E-12));
#13602=DIRECTION('',(-0.707106781186551,0.707106781186544,0.));
#13603=DIRECTION('center_axis',(-1.,0.,0.));
#13604=DIRECTION('ref_axis',(0.,0.,1.));
#13605=DIRECTION('',(0.,0.,-1.));
#13606=DIRECTION('',(3.27306316222039E-16,1.,0.));
#13607=DIRECTION('center_axis',(0.707106781186544,-0.707106781186551,0.));
#13608=DIRECTION('ref_axis',(0.707106781186551,0.707106781186544,0.));
#13609=DIRECTION('',(0.,0.,-1.));
#13610=DIRECTION('',(-0.707106781186551,-0.707106781186544,0.));
#13611=DIRECTION('center_axis',(1.,0.,-1.90771507937448E-16));
#13612=DIRECTION('ref_axis',(-1.90771507937448E-16,0.,-1.));
#13613=DIRECTION('center_axis',(1.,0.,-1.90771507937448E-16));
#13614=DIRECTION('ref_axis',(-1.90771507937448E-16,0.,-1.));
#13615=DIRECTION('',(1.90771507937448E-16,0.,1.));
#13616=DIRECTION('',(0.,-1.,0.));
#13617=DIRECTION('center_axis',(0.,0.,-1.));
#13618=DIRECTION('ref_axis',(-1.,0.,0.));
#13619=DIRECTION('',(1.,0.,0.));
#13620=DIRECTION('',(0.,-1.,0.));
#13621=DIRECTION('center_axis',(-1.,0.,0.));
#13622=DIRECTION('ref_axis',(0.,0.,1.));
#13623=DIRECTION('',(0.,0.,-1.));
#13624=DIRECTION('center_axis',(-1.,0.,0.));
#13625=DIRECTION('ref_axis',(0.,0.,1.));
#13626=DIRECTION('center_axis',(1.,0.,0.));
#13627=DIRECTION('ref_axis',(0.,0.,-1.));
#13628=DIRECTION('',(-1.,0.,0.));
#13629=DIRECTION('',(-1.,0.,0.));
#13630=DIRECTION('center_axis',(-0.707106781186544,-0.707106781186551,0.));
#13631=DIRECTION('ref_axis',(0.707106781186551,-0.707106781186544,0.));
#13632=DIRECTION('',(0.,0.,-1.));
#13633=DIRECTION('',(-0.707106781186551,0.707106781186544,0.));
#13634=DIRECTION('center_axis',(0.,-1.,0.));
#13635=DIRECTION('ref_axis',(0.,0.,-1.));
#13636=DIRECTION('',(-1.,1.63653158111019E-16,0.));
#13637=DIRECTION('center_axis',(0.,0.,1.));
#13638=DIRECTION('ref_axis',(1.,0.,0.));
#13639=DIRECTION('center_axis',(0.,0.,-1.));
#13640=DIRECTION('ref_axis',(-1.,0.,0.));
#13641=DIRECTION('center_axis',(0.,0.,1.));
#13642=DIRECTION('ref_axis',(1.,0.,0.));
#13643=DIRECTION('center_axis',(0.,0.,-1.));
#13644=DIRECTION('ref_axis',(1.,0.,0.));
#13645=DIRECTION('',(0.,0.,1.));
#13646=DIRECTION('center_axis',(0.,0.,1.));
#13647=DIRECTION('ref_axis',(-1.,0.,0.));
#13648=DIRECTION('center_axis',(0.,0.,1.));
#13649=DIRECTION('ref_axis',(1.,0.,0.));
#13650=DIRECTION('center_axis',(0.,0.,1.));
#13651=DIRECTION('ref_axis',(1.,0.,0.));
#13652=DIRECTION('',(0.,0.,1.));
#13653=DIRECTION('center_axis',(0.,0.,1.));
#13654=DIRECTION('ref_axis',(-1.,0.,0.));
#13655=DIRECTION('center_axis',(0.,0.,1.));
#13656=DIRECTION('ref_axis',(1.,0.,0.));
#13657=DIRECTION('center_axis',(0.,0.,1.));
#13658=DIRECTION('ref_axis',(1.,0.,0.));
#13659=DIRECTION('',(0.,0.,1.));
#13660=DIRECTION('center_axis',(0.,0.,1.));
#13661=DIRECTION('ref_axis',(-1.,0.,0.));
#13662=DIRECTION('center_axis',(0.,0.,1.));
#13663=DIRECTION('ref_axis',(1.,0.,0.));
#13664=DIRECTION('center_axis',(0.,0.,1.));
#13665=DIRECTION('ref_axis',(1.,0.,0.));
#13666=DIRECTION('',(0.,0.,1.));
#13667=DIRECTION('center_axis',(0.,0.,1.));
#13668=DIRECTION('ref_axis',(-1.,0.,0.));
#13669=DIRECTION('center_axis',(0.,0.,1.));
#13670=DIRECTION('ref_axis',(1.,0.,0.));
#13671=DIRECTION('center_axis',(0.,0.,1.));
#13672=DIRECTION('ref_axis',(1.,0.,0.));
#13673=DIRECTION('',(0.,0.,1.));
#13674=DIRECTION('center_axis',(0.,0.,1.));
#13675=DIRECTION('ref_axis',(-1.,0.,0.));
#13676=DIRECTION('center_axis',(0.,0.,1.));
#13677=DIRECTION('ref_axis',(1.,0.,0.));
#13678=DIRECTION('',(0.707106781186552,-0.707106781186543,0.));
#13679=DIRECTION('',(-2.38943891978177E-16,-1.,0.));
#13680=DIRECTION('',(0.707106781186551,0.707106781186544,0.));
#13681=DIRECTION('',(1.,0.,0.));
#13682=DIRECTION('',(0.707106781186551,-0.707106781186544,0.));
#13683=DIRECTION('',(-2.38943891978177E-16,1.,0.));
#13684=DIRECTION('',(0.707106781186551,0.707106781186544,0.));
#13685=DIRECTION('',(1.,0.,0.));
#13686=DIRECTION('center_axis',(0.,0.,-1.));
#13687=DIRECTION('ref_axis',(-1.,0.,0.));
#13688=DIRECTION('',(0.707106781186551,-0.707106781186544,0.));
#13689=DIRECTION('',(1.,0.,0.));
#13690=DIRECTION('',(0.707106781186551,0.707106781186544,0.));
#13691=DIRECTION('',(-2.38943891978177E-16,1.,0.));
#13692=DIRECTION('',(0.707106781186551,-0.707106781186544,0.));
#13693=DIRECTION('',(1.,0.,0.));
#13694=DIRECTION('',(0.707106781186552,0.707106781186543,0.));
#13695=DIRECTION('',(-2.38943891978177E-16,-1.,0.));
#13696=DIRECTION('center_axis',(0.,-1.,0.));
#13697=DIRECTION('ref_axis',(0.,0.,-1.));
#13698=DIRECTION('',(0.,0.,1.));
#13699=DIRECTION('',(0.,0.,1.));
#13700=DIRECTION('center_axis',(-0.707106781186544,-0.707106781186551,0.));
#13701=DIRECTION('ref_axis',(0.707106781186551,-0.707106781186544,0.));
#13702=DIRECTION('',(0.,0.,1.));
#13703=DIRECTION('center_axis',(0.707106781186544,-0.707106781186551,0.));
#13704=DIRECTION('ref_axis',(0.707106781186551,0.707106781186544,0.));
#13705=DIRECTION('',(0.,0.,1.));
#13706=DIRECTION('center_axis',(0.707106781186543,-0.707106781186552,0.));
#13707=DIRECTION('ref_axis',(0.707106781186552,0.707106781186543,0.));
#13708=DIRECTION('',(0.,0.,1.));
#13709=DIRECTION('',(0.,0.,1.));
#13710=DIRECTION('center_axis',(-0.707106781186544,-0.707106781186551,0.));
#13711=DIRECTION('ref_axis',(0.707106781186551,-0.707106781186544,0.));
#13712=DIRECTION('',(0.,0.,1.));
#13713=DIRECTION('',(0.,0.,1.));
#13714=DIRECTION('center_axis',(1.,2.38943891978177E-16,0.));
#13715=DIRECTION('ref_axis',(-2.38943891978177E-16,1.,0.));
#13716=DIRECTION('center_axis',(0.,-1.,0.));
#13717=DIRECTION('ref_axis',(0.,0.,-1.));
#13718=DIRECTION('center_axis',(-1.,2.38943891978176E-16,0.));
#13719=DIRECTION('ref_axis',(-2.38943891978176E-16,-1.,0.));
#13720=DIRECTION('center_axis',(0.,0.,1.));
#13721=DIRECTION('ref_axis',(1.,0.,0.));
#13722=DIRECTION('center_axis',(0.,0.,1.));
#13723=DIRECTION('ref_axis',(1.,0.,0.));
#13724=DIRECTION('center_axis',(0.,0.,1.));
#13725=DIRECTION('ref_axis',(1.,0.,0.));
#13726=DIRECTION('center_axis',(0.,0.,1.));
#13727=DIRECTION('ref_axis',(1.,0.,0.));
#13728=DIRECTION('axis',(0.,0.,1.));
#13729=DIRECTION('refdir',(1.,0.,0.));
#13730=DIRECTION('axis',(0.,0.,1.));
#13731=DIRECTION('refdir',(1.,0.,0.));
#13732=DIRECTION('center_axis',(-1.,0.,0.));
#13733=DIRECTION('ref_axis',(0.,-1.,0.));
#13734=DIRECTION('center_axis',(1.,0.,2.22044604925031E-16));
#13735=DIRECTION('ref_axis',(0.,-1.,0.));
#13736=DIRECTION('',(0.707106781186548,-0.707106781186547,8.65956056235492E-17));
#13737=DIRECTION('center_axis',(-1.,0.,-2.22044604925031E-16));
#13738=DIRECTION('ref_axis',(0.,-1.,0.));
#13739=DIRECTION('center_axis',(-1.,0.,0.));
#13740=DIRECTION('ref_axis',(0.,-1.,0.));
#13741=DIRECTION('center_axis',(-1.,0.,-2.22044604925031E-16));
#13742=DIRECTION('ref_axis',(0.,-1.,0.));
#13743=DIRECTION('',(1.,0.,0.));
#13744=DIRECTION('center_axis',(-1.,0.,-2.22044604925031E-16));
#13745=DIRECTION('ref_axis',(0.,-1.,0.));
#13746=DIRECTION('center_axis',(-1.,5.47382212626881E-48,-2.22044604925031E-16));
#13747=DIRECTION('ref_axis',(-5.47382212626881E-48,-1.,-1.21543267145725E-63));
#13748=DIRECTION('center_axis',(1.,0.,0.));
#13749=DIRECTION('ref_axis',(0.,-1.,0.));
#13750=DIRECTION('',(-0.707106781186548,-0.707106781186547,-8.65956056235492E-17));
#13751=DIRECTION('center_axis',(1.,0.,2.22044604925031E-16));
#13752=DIRECTION('ref_axis',(0.,-1.,0.));
#13753=DIRECTION('center_axis',(-1.,0.,-2.22044604925031E-16));
#13754=DIRECTION('ref_axis',(0.,-1.,0.));
#13755=DIRECTION('center_axis',(1.,-5.47382212626881E-48,2.22044604925031E-16));
#13756=DIRECTION('ref_axis',(-5.47382212626881E-48,-1.,-1.21543267145725E-63));
#13757=DIRECTION('center_axis',(-1.,0.,0.));
#13758=DIRECTION('ref_axis',(0.,-1.,0.));
#13759=DIRECTION('',(-1.,0.,0.));
#13760=DIRECTION('axis',(0.,0.,1.));
#13761=DIRECTION('refdir',(1.,0.,0.));
#13762=DIRECTION('center_axis',(1.,0.,0.));
#13763=DIRECTION('ref_axis',(0.,1.,0.));
#13764=DIRECTION('center_axis',(-1.,0.,0.));
#13765=DIRECTION('ref_axis',(0.,1.,0.));
#13766=DIRECTION('',(1.,0.,0.));
#13767=DIRECTION('center_axis',(-1.,0.,0.));
#13768=DIRECTION('ref_axis',(0.,1.,0.));
#13769=DIRECTION('center_axis',(1.,0.,0.));
#13770=DIRECTION('ref_axis',(0.,1.,0.));
#13771=DIRECTION('center_axis',(1.,0.,0.));
#13772=DIRECTION('ref_axis',(0.,1.,0.));
#13773=DIRECTION('',(-1.,0.,0.));
#13774=DIRECTION('center_axis',(1.,0.,0.));
#13775=DIRECTION('ref_axis',(0.,1.,0.));
#13776=DIRECTION('center_axis',(1.,0.,0.));
#13777=DIRECTION('ref_axis',(0.,1.,0.));
#13778=DIRECTION('center_axis',(1.,0.,0.));
#13779=DIRECTION('ref_axis',(0.,1.,0.));
#13780=DIRECTION('axis',(0.,0.,1.));
#13781=DIRECTION('refdir',(1.,0.,0.));
#13782=DIRECTION('center_axis',(0.,0.,-1.));
#13783=DIRECTION('ref_axis',(-1.,0.,0.));
#13784=DIRECTION('center_axis',(0.,0.,-1.));
#13785=DIRECTION('ref_axis',(-1.,0.,0.));
#13786=DIRECTION('',(0.500000000000001,-6.12323399573678E-17,-0.866025403784438));
#13787=DIRECTION('center_axis',(0.,0.,1.));
#13788=DIRECTION('ref_axis',(-1.,0.,0.));
#13789=DIRECTION('center_axis',(0.,0.,1.));
#13790=DIRECTION('ref_axis',(-1.,0.,0.));
#13791=DIRECTION('center_axis',(0.,0.,1.));
#13792=DIRECTION('ref_axis',(-1.,0.,0.));
#13793=DIRECTION('',(0.500000000000001,6.12323399573678E-17,0.866025403784438));
#13794=DIRECTION('center_axis',(0.,0.,-1.));
#13795=DIRECTION('ref_axis',(-1.,0.,0.));
#13796=DIRECTION('center_axis',(0.499999999999999,-0.866025403784439,0.));
#13797=DIRECTION('ref_axis',(-0.866025403784439,-0.499999999999999,0.));
#13798=DIRECTION('',(0.,0.,1.));
#13799=DIRECTION('',(0.,0.,-1.));
#13800=DIRECTION('center_axis',(1.,-7.20364017026615E-16,0.));
#13801=DIRECTION('ref_axis',(-7.20364017026615E-16,-1.,0.));
#13802=DIRECTION('',(0.,0.,1.));
#13803=DIRECTION('center_axis',(0.,0.,1.));
#13804=DIRECTION('ref_axis',(-1.,0.,0.));
#13805=DIRECTION('',(-0.86602540378444,-1.06057523872491E-16,-0.499999999999998));
#13806=DIRECTION('center_axis',(0.,0.,-1.));
#13807=DIRECTION('ref_axis',(1.,0.,0.));
#13808=DIRECTION('center_axis',(-0.500000000000001,-0.866025403784438,0.));
#13809=DIRECTION('ref_axis',(-0.866025403784438,0.500000000000001,0.));
#13810=DIRECTION('',(0.,0.,1.));
#13811=DIRECTION('center_axis',(-1.,8.4282869694135E-16,0.));
#13812=DIRECTION('ref_axis',(8.4282869694135E-16,1.,0.));
#13813=DIRECTION('',(0.,0.,1.));
#13814=DIRECTION('center_axis',(-0.499999999999999,0.866025403784439,0.));
#13815=DIRECTION('ref_axis',(0.866025403784439,0.499999999999999,0.));
#13816=DIRECTION('',(0.,0.,1.));
#13817=DIRECTION('center_axis',(0.500000000000001,0.866025403784438,0.));
#13818=DIRECTION('ref_axis',(0.866025403784438,-0.500000000000001,0.));
#13819=DIRECTION('center_axis',(0.,0.,1.));
#13820=DIRECTION('ref_axis',(1.,0.,0.));
#13821=DIRECTION('center_axis',(0.,0.,-1.));
#13822=DIRECTION('ref_axis',(1.,0.,0.));
#13823=DIRECTION('center_axis',(0.,0.,-1.));
#13824=DIRECTION('ref_axis',(-1.,0.,0.));
#13825=DIRECTION('',(-0.86602540378444,1.06057523872491E-16,0.499999999999998));
#13826=DIRECTION('center_axis',(0.,0.,-1.));
#13827=DIRECTION('ref_axis',(-1.,0.,0.));
#13828=DIRECTION('center_axis',(0.,0.,-1.));
#13829=DIRECTION('ref_axis',(-1.,0.,0.));
#13830=DIRECTION('',(0.,0.,-1.));
#13831=DIRECTION('axis',(0.,0.,1.));
#13832=DIRECTION('refdir',(1.,0.,0.));
#13833=DIRECTION('center_axis',(0.,0.,1.));
#13834=DIRECTION('ref_axis',(1.,0.,0.));
#13835=DIRECTION('center_axis',(0.,0.,1.));
#13836=DIRECTION('ref_axis',(1.,0.,0.));
#13837=DIRECTION('',(0.,0.,1.));
#13838=DIRECTION('center_axis',(0.,0.,1.));
#13839=DIRECTION('ref_axis',(1.,0.,0.));
#13840=DIRECTION('center_axis',(0.,0.,1.));
#13841=DIRECTION('ref_axis',(1.,0.,0.));
#13842=DIRECTION('center_axis',(0.,0.,1.));
#13843=DIRECTION('ref_axis',(1.,0.,0.));
#13844=DIRECTION('center_axis',(-1.22464679914735E-16,1.,0.));
#13845=DIRECTION('ref_axis',(-1.,-1.22464679914735E-16,0.));
#13846=DIRECTION('center_axis',(0.,0.,1.));
#13847=DIRECTION('ref_axis',(1.,0.,0.));
#13848=DIRECTION('center_axis',(0.,0.,1.));
#13849=DIRECTION('ref_axis',(1.,0.,0.));
#13850=DIRECTION('',(0.,0.,1.));
#13851=DIRECTION('center_axis',(0.,0.,1.));
#13852=DIRECTION('ref_axis',(1.,0.,0.));
#13853=DIRECTION('center_axis',(0.,0.,1.));
#13854=DIRECTION('ref_axis',(1.,0.,0.));
#13855=DIRECTION('',(0.707106781186547,8.65956056235492E-17,-0.707106781186548));
#13856=DIRECTION('center_axis',(0.,0.,1.));
#13857=DIRECTION('ref_axis',(1.,0.,0.));
#13858=DIRECTION('center_axis',(0.,0.,1.));
#13859=DIRECTION('ref_axis',(1.,0.,0.));
#13860=DIRECTION('center_axis',(0.,0.,1.));
#13861=DIRECTION('ref_axis',(1.,0.,0.));
#13862=DIRECTION('center_axis',(0.,0.,1.));
#13863=DIRECTION('ref_axis',(1.,0.,0.));
#13864=DIRECTION('',(0.,0.,-1.));
#13865=DIRECTION('center_axis',(0.,0.,-1.));
#13866=DIRECTION('ref_axis',(-1.,0.,0.));
#13867=DIRECTION('',(-0.707106781186547,8.65956056235493E-17,0.707106781186548));
#13868=DIRECTION('center_axis',(0.,0.,1.));
#13869=DIRECTION('ref_axis',(1.,0.,0.));
#13870=DIRECTION('center_axis',(0.,0.,1.));
#13871=DIRECTION('ref_axis',(1.,0.,0.));
#13872=DIRECTION('center_axis',(0.,0.,-1.));
#13873=DIRECTION('ref_axis',(-1.,0.,0.));
#13874=DIRECTION('center_axis',(0.,0.,1.));
#13875=DIRECTION('ref_axis',(1.,0.,0.));
#13876=DIRECTION('center_axis',(0.,0.,1.));
#13877=DIRECTION('ref_axis',(1.,0.,0.));
#13878=DIRECTION('',(0.,0.,-1.));
#13879=DIRECTION('center_axis',(0.,0.,1.));
#13880=DIRECTION('ref_axis',(1.,0.,0.));
#13881=DIRECTION('center_axis',(0.,0.,1.));
#13882=DIRECTION('ref_axis',(1.,0.,0.));
#13883=DIRECTION('center_axis',(-1.22464679914735E-16,1.,0.));
#13884=DIRECTION('ref_axis',(-1.,-1.22464679914735E-16,0.));
#13885=DIRECTION('center_axis',(0.,0.,1.));
#13886=DIRECTION('ref_axis',(1.,0.,0.));
#13887=DIRECTION('center_axis',(0.,0.,1.));
#13888=DIRECTION('ref_axis',(1.,0.,0.));
#13889=DIRECTION('center_axis',(0.,0.,1.));
#13890=DIRECTION('ref_axis',(1.,0.,0.));
#13891=DIRECTION('',(0.,0.,1.));
#13892=DIRECTION('center_axis',(0.,0.,1.));
#13893=DIRECTION('ref_axis',(1.,0.,0.));
#13894=DIRECTION('center_axis',(0.,0.,1.));
#13895=DIRECTION('ref_axis',(1.,0.,0.));
#13896=DIRECTION('',(-0.707106781186549,-8.65956056235495E-17,0.707106781186546));
#13897=DIRECTION('center_axis',(0.,0.,1.));
#13898=DIRECTION('ref_axis',(1.,0.,0.));
#13899=DIRECTION('center_axis',(0.,0.,-1.));
#13900=DIRECTION('ref_axis',(-1.,0.,0.));
#13901=DIRECTION('center_axis',(0.,0.,1.));
#13902=DIRECTION('ref_axis',(1.,0.,0.));
#13903=DIRECTION('center_axis',(0.,0.,1.));
#13904=DIRECTION('ref_axis',(1.,0.,0.));
#13905=DIRECTION('center_axis',(0.,0.,1.));
#13906=DIRECTION('ref_axis',(1.,0.,0.));
#13907=DIRECTION('',(-0.707106781186549,-8.65956056235495E-17,0.707106781186546));
#13908=DIRECTION('center_axis',(0.,0.,1.));
#13909=DIRECTION('ref_axis',(1.,0.,0.));
#13910=DIRECTION('center_axis',(0.,0.,1.));
#13911=DIRECTION('ref_axis',(1.,0.,0.));
#13912=DIRECTION('center_axis',(0.,0.,1.));
#13913=DIRECTION('ref_axis',(1.,0.,0.));
#13914=DIRECTION('center_axis',(0.,0.,1.));
#13915=DIRECTION('ref_axis',(1.,0.,0.));
#13916=DIRECTION('',(0.,0.,1.));
#13917=DIRECTION('center_axis',(0.,0.,-1.));
#13918=DIRECTION('ref_axis',(-1.,0.,0.));
#13919=DIRECTION('',(0.707106781186547,-8.65956056235492E-17,-0.707106781186548));
#13920=DIRECTION('center_axis',(0.,0.,1.));
#13921=DIRECTION('ref_axis',(1.,0.,0.));
#13922=DIRECTION('center_axis',(0.,0.,1.));
#13923=DIRECTION('ref_axis',(1.,0.,0.));
#13924=DIRECTION('center_axis',(0.,0.,1.));
#13925=DIRECTION('ref_axis',(1.,0.,0.));
#13926=DIRECTION('',(0.,0.,-1.));
#13927=DIRECTION('center_axis',(0.,0.,1.));
#13928=DIRECTION('ref_axis',(1.,0.,0.));
#13929=DIRECTION('center_axis',(0.,0.,1.));
#13930=DIRECTION('ref_axis',(1.,0.,0.));
#13931=DIRECTION('center_axis',(0.,0.,1.));
#13932=DIRECTION('ref_axis',(1.,0.,0.));
#13933=DIRECTION('center_axis',(-1.22464679914735E-16,1.,0.));
#13934=DIRECTION('ref_axis',(-1.,-1.22464679914735E-16,0.));
#13935=DIRECTION('center_axis',(0.,0.,1.));
#13936=DIRECTION('ref_axis',(1.,0.,0.));
#13937=DIRECTION('center_axis',(0.,0.,1.));
#13938=DIRECTION('ref_axis',(1.,0.,0.));
#13939=DIRECTION('',(0.,0.,-1.));
#13940=DIRECTION('center_axis',(0.,0.,1.));
#13941=DIRECTION('ref_axis',(1.,0.,0.));
#13942=DIRECTION('center_axis',(0.,0.,1.));
#13943=DIRECTION('ref_axis',(1.,0.,0.));
#13944=DIRECTION('center_axis',(0.,0.,1.));
#13945=DIRECTION('ref_axis',(1.,0.,0.));
#13946=DIRECTION('',(0.707106781186549,8.65956056235495E-17,-0.707106781186546));
#13947=DIRECTION('center_axis',(0.,0.,-1.));
#13948=DIRECTION('ref_axis',(-1.,0.,0.));
#13949=DIRECTION('center_axis',(0.,0.,-1.));
#13950=DIRECTION('ref_axis',(-1.,0.,0.));
#13951=DIRECTION('center_axis',(0.,0.,1.));
#13952=DIRECTION('ref_axis',(1.,0.,0.));
#13953=DIRECTION('center_axis',(-1.,0.,0.));
#13954=DIRECTION('ref_axis',(0.,1.,0.));
#13955=DIRECTION('center_axis',(0.,1.22464679914735E-16,1.));
#13956=DIRECTION('ref_axis',(0.,-1.,1.22464679914735E-16));
#13957=DIRECTION('center_axis',(-0.809016994374946,0.587785252292475,0.));
#13958=DIRECTION('ref_axis',(0.587785252292475,0.809016994374946,0.));
#13959=DIRECTION('center_axis',(7.19829327805999E-17,9.9076007261709E-17,
1.));
#13960=DIRECTION('ref_axis',(-0.587785252292475,-0.809016994374946,1.22464679914735E-16));
#13961=DIRECTION('center_axis',(-0.309016994374945,0.951056516295154,0.));
#13962=DIRECTION('ref_axis',(0.951056516295154,0.309016994374945,0.));
#13963=DIRECTION('center_axis',(1.16470831848909E-16,3.78436673043412E-17,
1.));
#13964=DIRECTION('ref_axis',(-0.951056516295154,-0.309016994374945,1.22464679914735E-16));
#13965=DIRECTION('center_axis',(0.309016994374952,0.951056516295152,0.));
#13966=DIRECTION('ref_axis',(0.951056516295152,-0.309016994374952,0.));
#13967=DIRECTION('center_axis',(1.16470831848909E-16,-3.78436673043421E-17,
1.));
#13968=DIRECTION('ref_axis',(-0.951056516295152,0.309016994374952,1.22464679914735E-16));
#13969=DIRECTION('center_axis',(0.809016994374951,0.587785252292469,0.));
#13970=DIRECTION('ref_axis',(0.587785252292469,-0.809016994374951,0.));
#13971=DIRECTION('center_axis',(7.19829327805991E-17,-9.90760072617096E-17,
1.));
#13972=DIRECTION('ref_axis',(-0.587785252292469,0.809016994374951,1.22464679914735E-16));
#13973=DIRECTION('center_axis',(1.,-7.32967169076673E-15,0.));
#13974=DIRECTION('ref_axis',(-7.32967169076675E-15,-1.,0.));
#13975=DIRECTION('center_axis',(-8.97625897489847E-31,-1.22464679914735E-16,
1.));
#13976=DIRECTION('ref_axis',(7.32967169076675E-15,1.,1.22464679914735E-16));
#13977=DIRECTION('center_axis',(0.809016994374942,-0.587785252292481,0.));
#13978=DIRECTION('ref_axis',(-0.587785252292481,-0.809016994374942,0.));
#13979=DIRECTION('center_axis',(-7.19829327806006E-17,-9.90760072617085E-17,
1.));
#13980=DIRECTION('ref_axis',(0.587785252292481,0.809016994374942,1.22464679914735E-16));
#13981=DIRECTION('center_axis',(0.309016994374938,-0.951056516295157,0.));
#13982=DIRECTION('ref_axis',(-0.951056516295157,-0.309016994374938,0.));
#13983=DIRECTION('center_axis',(-1.1647083184891E-16,-3.78436673043403E-17,
1.));
#13984=DIRECTION('ref_axis',(0.951056516295157,0.309016994374938,1.22464679914735E-16));
#13985=DIRECTION('center_axis',(-0.309016994374958,-0.95105651629515,0.));
#13986=DIRECTION('ref_axis',(-0.95105651629515,0.309016994374958,0.));
#13987=DIRECTION('center_axis',(-1.16470831848909E-16,3.78436673043428E-17,
1.));
#13988=DIRECTION('ref_axis',(0.95105651629515,-0.309016994374958,1.22464679914735E-16));
#13989=DIRECTION('center_axis',(-0.809016994374955,-0.587785252292462,0.));
#13990=DIRECTION('ref_axis',(-0.587785252292462,0.809016994374955,0.));
#13991=DIRECTION('center_axis',(-7.19829327805983E-17,9.90760072617101E-17,
1.));
#13992=DIRECTION('ref_axis',(0.587785252292462,-0.809016994374955,1.22464679914735E-16));
#13993=DIRECTION('',(0.,0.,1.));
#13994=DIRECTION('',(1.,0.,0.));
#13995=DIRECTION('',(0.,0.,1.));
#13996=DIRECTION('',(1.,0.,0.));
#13997=DIRECTION('',(-1.,-1.11022302462515E-16,1.40165656858926E-15));
#13998=DIRECTION('',(-1.40165656858926E-15,-2.35733825192999E-31,-1.));
#13999=DIRECTION('',(1.,1.11022302462516E-16,-3.33066907387547E-16));
#14000=DIRECTION('',(-3.33066907387547E-16,-5.55111512312579E-17,-1.));
#14001=DIRECTION('',(1.,1.11022302462516E-16,-3.33066907387547E-16));
#14002=DIRECTION('',(-3.33066907387547E-16,-5.55111512312579E-17,-1.));
#14003=DIRECTION('axis',(0.,0.,1.));
#14004=DIRECTION('refdir',(1.,0.,0.));
#14005=DIRECTION('center_axis',(1.,0.,1.02489030670754E-15));
#14006=DIRECTION('ref_axis',(1.02489030670754E-15,0.,-1.));
#14007=DIRECTION('',(-1.02489030670754E-15,0.,1.));
#14008=DIRECTION('',(0.,1.,0.));
#14009=DIRECTION('',(1.02489030670754E-15,0.,-1.));
#14010=DIRECTION('',(0.,1.,0.));
#14011=DIRECTION('center_axis',(-1.,0.,-1.02489030670754E-15));
#14012=DIRECTION('ref_axis',(-1.02489030670754E-15,0.,1.));
#14013=DIRECTION('',(-1.02489030670754E-15,0.,1.));
#14014=DIRECTION('',(0.,1.,0.));
#14015=DIRECTION('',(1.02489030670754E-15,0.,-1.));
#14016=DIRECTION('',(0.,1.,0.));
#14017=DIRECTION('center_axis',(1.,0.,1.02489030670754E-15));
#14018=DIRECTION('ref_axis',(1.02489030670754E-15,0.,-1.));
#14019=DIRECTION('',(0.,1.,0.));
#14020=DIRECTION('',(1.02489030670754E-15,0.,-1.));
#14021=DIRECTION('',(0.,1.,0.));
#14022=DIRECTION('',(-1.02489030670754E-15,0.,1.));
#14023=DIRECTION('center_axis',(1.02489030670754E-15,0.,-1.));
#14024=DIRECTION('ref_axis',(-1.,0.,-1.02489030670754E-15));
#14025=DIRECTION('',(0.,1.,0.));
#14026=DIRECTION('',(1.,0.,1.02489030670754E-15));
#14027=DIRECTION('',(0.,1.,0.));
#14028=DIRECTION('',(-1.,0.,-1.02489030670754E-15));
#14029=DIRECTION('center_axis',(-1.,0.,-1.02489030670754E-15));
#14030=DIRECTION('ref_axis',(-1.02489030670754E-15,0.,1.));
#14031=DIRECTION('',(0.,1.,0.));
#14032=DIRECTION('',(-1.02489030670754E-15,0.,1.));
#14033=DIRECTION('',(0.,1.,0.));
#14034=DIRECTION('',(1.02489030670754E-15,0.,-1.));
#14035=DIRECTION('center_axis',(0.,-1.,0.));
#14036=DIRECTION('ref_axis',(-1.,0.,-1.02489030670754E-15));
#14037=DIRECTION('center_axis',(0.,-1.,0.));
#14038=DIRECTION('ref_axis',(-1.,0.,-1.02489030670754E-15));
#14039=DIRECTION('',(0.,-1.,0.));
#14040=DIRECTION('center_axis',(0.,1.,0.));
#14041=DIRECTION('ref_axis',(-1.,0.,-1.02489030670754E-15));
#14042=DIRECTION('center_axis',(-1.02489030670754E-15,0.,1.));
#14043=DIRECTION('ref_axis',(1.,0.,1.02489030670754E-15));
#14044=DIRECTION('',(0.,1.,0.));
#14045=DIRECTION('',(-1.,0.,-1.02489030670754E-15));
#14046=DIRECTION('',(0.,1.,0.));
#14047=DIRECTION('',(1.,0.,1.02489030670754E-15));
#14048=DIRECTION('center_axis',(1.,0.,8.41193286835436E-16));
#14049=DIRECTION('ref_axis',(8.41193286835436E-16,0.,-1.));
#14050=DIRECTION('',(-8.41193286835436E-16,0.,1.));
#14051=DIRECTION('',(0.,1.,0.));
#14052=DIRECTION('',(-8.41193286835436E-16,0.,1.));
#14053=DIRECTION('',(0.,1.,0.));
#14054=DIRECTION('center_axis',(0.707106781186547,0.,0.707106781186548));
#14055=DIRECTION('ref_axis',(0.707106781186548,0.,-0.707106781186547));
#14056=DIRECTION('',(-0.707106781186548,0.,0.707106781186547));
#14057=DIRECTION('',(-0.707106781186548,0.,0.707106781186547));
#14058=DIRECTION('center_axis',(-0.707106781186547,0.,-0.707106781186548));
#14059=DIRECTION('ref_axis',(-0.707106781186548,0.,0.707106781186547));
#14060=DIRECTION('',(-0.707106781186548,0.,0.707106781186547));
#14061=DIRECTION('',(0.,1.,0.));
#14062=DIRECTION('',(0.707106781186548,0.,-0.707106781186547));
#14063=DIRECTION('center_axis',(-5.24835571952591E-16,0.,-1.));
#14064=DIRECTION('ref_axis',(-1.,0.,5.24835571952591E-16));
#14065=DIRECTION('',(-1.,0.,5.24835571952591E-16));
#14066=DIRECTION('',(0.,1.,0.));
#14067=DIRECTION('',(1.,0.,-5.24835571952591E-16));
#14068=DIRECTION('center_axis',(1.,0.,-8.04181361684024E-17));
#14069=DIRECTION('ref_axis',(-8.04181361684024E-17,0.,-1.));
#14070=DIRECTION('',(8.04181361684024E-17,0.,1.));
#14071=DIRECTION('',(0.,1.,0.));
#14072=DIRECTION('',(8.04181361684024E-17,0.,1.));
#14073=DIRECTION('center_axis',(8.41193286835436E-16,0.,-1.));
#14074=DIRECTION('ref_axis',(-1.,0.,-8.41193286835436E-16));
#14075=DIRECTION('',(1.,0.,8.41193286835436E-16));
#14076=DIRECTION('',(0.,1.,0.));
#14077=DIRECTION('',(1.,0.,8.41193286835436E-16));
#14078=DIRECTION('center_axis',(-0.707106781186547,0.,-0.707106781186548));
#14079=DIRECTION('ref_axis',(-0.707106781186548,0.,0.707106781186547));
#14080=DIRECTION('',(-0.707106781186548,0.,0.707106781186547));
#14081=DIRECTION('',(0.,1.,0.));
#14082=DIRECTION('',(0.707106781186548,0.,-0.707106781186547));
#14083=DIRECTION('center_axis',(-1.,0.,-3.89980473439034E-16));
#14084=DIRECTION('ref_axis',(-3.89980473439034E-16,0.,1.));
#14085=DIRECTION('',(-3.89980473439034E-16,0.,1.));
#14086=DIRECTION('',(0.,1.,0.));
#14087=DIRECTION('',(3.89980473439034E-16,0.,-1.));
#14088=DIRECTION('center_axis',(0.,-1.,0.));
#14089=DIRECTION('ref_axis',(7.50253143458634E-15,0.,-1.));
#14090=DIRECTION('center_axis',(0.,-1.,0.));
#14091=DIRECTION('ref_axis',(7.50253143458634E-15,0.,-1.));
#14092=DIRECTION('',(0.,1.,0.));
#14093=DIRECTION('center_axis',(0.,1.,0.));
#14094=DIRECTION('ref_axis',(7.50253143458634E-15,0.,-1.));
#14095=DIRECTION('center_axis',(-8.41193286835436E-16,0.,1.));
#14096=DIRECTION('ref_axis',(1.,0.,8.41193286835436E-16));
#14097=DIRECTION('',(1.,0.,8.41193286835436E-16));
#14098=DIRECTION('',(0.,1.,0.));
#14099=DIRECTION('',(-1.,0.,-8.41193286835436E-16));
#14100=DIRECTION('center_axis',(0.707106781186546,0.,0.707106781186549));
#14101=DIRECTION('ref_axis',(0.707106781186549,0.,-0.707106781186546));
#14102=DIRECTION('',(-0.707106781186549,0.,0.707106781186546));
#14103=DIRECTION('',(0.,1.,0.));
#14104=DIRECTION('',(-0.707106781186549,0.,0.707106781186546));
#14105=DIRECTION('center_axis',(1.,0.,8.41193286835436E-16));
#14106=DIRECTION('ref_axis',(8.41193286835436E-16,0.,-1.));
#14107=DIRECTION('',(8.41193286835436E-16,0.,-1.));
#14108=DIRECTION('',(0.,1.,0.));
#14109=DIRECTION('',(-8.41193286835436E-16,0.,1.));
#14110=DIRECTION('center_axis',(8.41193286835436E-16,0.,-1.));
#14111=DIRECTION('ref_axis',(-1.,0.,-8.41193286835436E-16));
#14112=DIRECTION('',(-1.,0.,-8.41193286835436E-16));
#14113=DIRECTION('',(1.,0.,8.41193286835436E-16));
#14114=DIRECTION('center_axis',(-1.,0.,-9.63657966750171E-16));
#14115=DIRECTION('ref_axis',(-9.63657966750171E-16,0.,1.));
#14116=DIRECTION('',(9.63657966750171E-16,0.,-1.));
#14117=DIRECTION('',(0.,1.,0.));
#14118=DIRECTION('',(9.63657966750171E-16,0.,-1.));
#14119=DIRECTION('',(0.,1.,0.));
#14120=DIRECTION('center_axis',(-0.707106781186547,0.,-0.707106781186548));
#14121=DIRECTION('ref_axis',(-0.707106781186548,0.,0.707106781186547));
#14122=DIRECTION('',(0.707106781186548,0.,-0.707106781186547));
#14123=DIRECTION('',(0.707106781186548,0.,-0.707106781186547));
#14124=DIRECTION('center_axis',(0.707106781186547,0.,0.707106781186548));
#14125=DIRECTION('ref_axis',(0.707106781186548,0.,-0.707106781186547));
#14126=DIRECTION('',(0.707106781186548,0.,-0.707106781186547));
#14127=DIRECTION('',(-0.707106781186548,0.,0.707106781186547));
#14128=DIRECTION('center_axis',(-0.707106781186546,0.,-0.707106781186549));
#14129=DIRECTION('ref_axis',(-0.707106781186549,0.,0.707106781186546));
#14130=DIRECTION('',(0.707106781186549,0.,-0.707106781186546));
#14131=DIRECTION('',(0.,1.,0.));
#14132=DIRECTION('',(0.707106781186549,0.,-0.707106781186546));
#14133=DIRECTION('',(0.,1.,0.));
#14134=DIRECTION('center_axis',(-1.,0.,-9.63657966750171E-16));
#14135=DIRECTION('ref_axis',(-9.63657966750171E-16,0.,1.));
#14136=DIRECTION('',(-9.63657966750171E-16,0.,1.));
#14137=DIRECTION('',(0.,1.,0.));
#14138=DIRECTION('',(9.63657966750171E-16,0.,-1.));
#14139=DIRECTION('center_axis',(-9.63657966750171E-16,0.,1.));
#14140=DIRECTION('ref_axis',(1.,0.,9.63657966750171E-16));
#14141=DIRECTION('',(1.,0.,9.63657966750171E-16));
#14142=DIRECTION('',(-1.,0.,-9.63657966750171E-16));
#14143=DIRECTION('center_axis',(-1.02489030670754E-15,0.,1.));
#14144=DIRECTION('ref_axis',(1.,0.,1.02489030670754E-15));
#14145=DIRECTION('',(-1.,0.,-1.02489030670754E-15));
#14146=DIRECTION('',(0.,1.,0.));
#14147=DIRECTION('',(-1.,0.,-1.02489030670754E-15));
#14148=DIRECTION('',(0.,1.,0.));
#14149=DIRECTION('center_axis',(-0.707106781186548,0.,0.707106781186547));
#14150=DIRECTION('ref_axis',(0.707106781186547,0.,0.707106781186548));
#14151=DIRECTION('',(-0.707106781186547,0.,-0.707106781186548));
#14152=DIRECTION('',(-0.707106781186547,0.,-0.707106781186548));
#14153=DIRECTION('center_axis',(0.707106781186548,0.,-0.707106781186547));
#14154=DIRECTION('ref_axis',(-0.707106781186547,0.,-0.707106781186548));
#14155=DIRECTION('',(-0.707106781186547,0.,-0.707106781186548));
#14156=DIRECTION('',(0.,1.,0.));
#14157=DIRECTION('',(0.707106781186547,0.,0.707106781186548));
#14158=DIRECTION('center_axis',(1.,0.,-3.41138552080488E-16));
#14159=DIRECTION('ref_axis',(-3.41138552080488E-16,0.,-1.));
#14160=DIRECTION('',(-3.41138552080488E-16,0.,-1.));
#14161=DIRECTION('',(0.,1.,0.));
#14162=DIRECTION('',(3.41138552080488E-16,0.,1.));
#14163=DIRECTION('center_axis',(-1.03278883703701E-16,0.,1.));
#14164=DIRECTION('ref_axis',(1.,0.,1.03278883703701E-16));
#14165=DIRECTION('',(-1.,0.,-1.03278883703701E-16));
#14166=DIRECTION('',(0.,1.,0.));
#14167=DIRECTION('',(-1.,0.,-1.03278883703701E-16));
#14168=DIRECTION('center_axis',(1.,0.,1.02489030670754E-15));
#14169=DIRECTION('ref_axis',(1.02489030670754E-15,0.,-1.));
#14170=DIRECTION('',(-1.02489030670754E-15,0.,1.));
#14171=DIRECTION('',(0.,1.,0.));
#14172=DIRECTION('',(-1.02489030670754E-15,0.,1.));
#14173=DIRECTION('center_axis',(0.707106781186548,0.,-0.707106781186547));
#14174=DIRECTION('ref_axis',(-0.707106781186547,0.,-0.707106781186548));
#14175=DIRECTION('',(-0.707106781186547,0.,-0.707106781186548));
#14176=DIRECTION('',(0.,1.,0.));
#14177=DIRECTION('',(0.707106781186547,0.,0.707106781186548));
#14178=DIRECTION('center_axis',(5.73677493311137E-16,0.,-1.));
#14179=DIRECTION('ref_axis',(-1.,0.,-5.73677493311137E-16));
#14180=DIRECTION('',(-1.,0.,-5.73677493311137E-16));
#14181=DIRECTION('',(0.,1.,0.));
#14182=DIRECTION('',(1.,0.,5.73677493311137E-16));
#14183=DIRECTION('center_axis',(0.,-1.,0.));
#14184=DIRECTION('ref_axis',(1.,0.,7.68622845445844E-15));
#14185=DIRECTION('center_axis',(0.,-1.,0.));
#14186=DIRECTION('ref_axis',(1.,0.,7.68622845445844E-15));
#14187=DIRECTION('',(0.,1.,0.));
#14188=DIRECTION('center_axis',(0.,1.,0.));
#14189=DIRECTION('ref_axis',(1.,0.,7.68622845445844E-15));
#14190=DIRECTION('center_axis',(-1.,0.,-1.02489030670754E-15));
#14191=DIRECTION('ref_axis',(-1.02489030670754E-15,0.,1.));
#14192=DIRECTION('',(-1.02489030670754E-15,0.,1.));
#14193=DIRECTION('',(0.,1.,0.));
#14194=DIRECTION('',(1.02489030670754E-15,0.,-1.));
#14195=DIRECTION('center_axis',(-0.707106781186549,0.,0.707106781186546));
#14196=DIRECTION('ref_axis',(0.707106781186546,0.,0.707106781186549));
#14197=DIRECTION('',(-0.707106781186546,0.,-0.707106781186549));
#14198=DIRECTION('',(0.,1.,0.));
#14199=DIRECTION('',(-0.707106781186546,0.,-0.707106781186549));
#14200=DIRECTION('center_axis',(-1.02489030670754E-15,0.,1.));
#14201=DIRECTION('ref_axis',(1.,0.,1.02489030670754E-15));
#14202=DIRECTION('',(1.,0.,1.02489030670754E-15));
#14203=DIRECTION('',(0.,1.,0.));
#14204=DIRECTION('',(-1.,0.,-1.02489030670754E-15));
#14205=DIRECTION('center_axis',(1.,0.,1.02489030670754E-15));
#14206=DIRECTION('ref_axis',(1.02489030670754E-15,0.,-1.));
#14207=DIRECTION('',(1.02489030670754E-15,0.,-1.));
#14208=DIRECTION('',(-1.02489030670754E-15,0.,1.));
#14209=DIRECTION('center_axis',(0.707106781186548,0.,-0.707106781186547));
#14210=DIRECTION('ref_axis',(-0.707106781186547,0.,-0.707106781186548));
#14211=DIRECTION('',(0.707106781186547,0.,0.707106781186548));
#14212=DIRECTION('',(0.707106781186547,0.,0.707106781186548));
#14213=DIRECTION('center_axis',(-0.707106781186548,0.,0.707106781186547));
#14214=DIRECTION('ref_axis',(0.707106781186547,0.,0.707106781186548));
#14215=DIRECTION('',(0.707106781186547,0.,0.707106781186548));
#14216=DIRECTION('',(0.,1.,0.));
#14217=DIRECTION('',(-0.707106781186547,0.,-0.707106781186548));
#14218=DIRECTION('center_axis',(-1.,0.,4.63603231995223E-16));
#14219=DIRECTION('ref_axis',(4.63603231995223E-16,0.,1.));
#14220=DIRECTION('',(4.63603231995223E-16,0.,1.));
#14221=DIRECTION('',(0.,1.,0.));
#14222=DIRECTION('',(-4.63603231995223E-16,0.,-1.));
#14223=DIRECTION('center_axis',(-1.91857962110348E-17,0.,-1.));
#14224=DIRECTION('ref_axis',(-1.,0.,1.91857962110348E-17));
#14225=DIRECTION('',(1.,0.,-1.91857962110348E-17));
#14226=DIRECTION('',(0.,1.,0.));
#14227=DIRECTION('',(1.,0.,-1.91857962110348E-17));
#14228=DIRECTION('center_axis',(-1.,0.,-9.02425626792803E-16));
#14229=DIRECTION('ref_axis',(-9.02425626792803E-16,0.,1.));
#14230=DIRECTION('',(9.02425626792803E-16,0.,-1.));
#14231=DIRECTION('',(0.,1.,0.));
#14232=DIRECTION('',(9.02425626792803E-16,0.,-1.));
#14233=DIRECTION('center_axis',(-0.707106781186548,0.,0.707106781186547));
#14234=DIRECTION('ref_axis',(0.707106781186547,0.,0.707106781186548));
#14235=DIRECTION('',(0.707106781186547,0.,0.707106781186548));
#14236=DIRECTION('',(0.,1.,0.));
#14237=DIRECTION('',(-0.707106781186547,0.,-0.707106781186548));
#14238=DIRECTION('center_axis',(4.94455241362763E-16,0.,1.));
#14239=DIRECTION('ref_axis',(1.,0.,-4.94455241362763E-16));
#14240=DIRECTION('',(-1.,0.,4.94455241362763E-16));
#14241=DIRECTION('',(-1.,0.,4.94455241362763E-16));
#14242=DIRECTION('',(0.,1.,0.));
#14243=DIRECTION('center_axis',(1.,0.,0.));
#14244=DIRECTION('ref_axis',(0.,0.,-1.));
#14245=DIRECTION('',(0.,0.,1.));
#14246=DIRECTION('',(0.,0.,1.));
#14247=DIRECTION('',(0.,1.,0.));
#14248=DIRECTION('center_axis',(0.,1.,0.));
#14249=DIRECTION('ref_axis',(-1.,0.,-1.22464679914735E-16));
#14250=DIRECTION('',(1.,0.,4.51212813396402E-16));
#14251=DIRECTION('',(1.,0.,6.12323399573677E-17));
#14252=DIRECTION('',(-0.707106781186548,0.,-0.707106781186547));
#14253=DIRECTION('',(-6.12323399573677E-17,0.,1.));
#14254=DIRECTION('',(-1.,0.,-6.12323399573677E-17));
#14255=DIRECTION('',(6.12323399573677E-17,0.,-1.));
#14256=DIRECTION('',(-0.707106781186547,0.,-0.707106781186548));
#14257=DIRECTION('',(1.,0.,0.));
#14258=DIRECTION('',(0.707106781186548,0.,-0.707106781186547));
#14259=DIRECTION('',(1.36602885878803E-15,0.,-1.));
#14260=DIRECTION('',(1.,0.,9.21611423003838E-16));
#14261=DIRECTION('',(0.,0.,1.));
#14262=DIRECTION('',(0.707106781186548,0.,-0.707106781186547));
#14263=DIRECTION('',(1.,0.,4.51212813396402E-16));
#14264=DIRECTION('center_axis',(0.,1.,0.));
#14265=DIRECTION('ref_axis',(-1.,0.,6.6613381477509E-15));
#14266=DIRECTION('',(0.,0.,1.));
#14267=DIRECTION('',(0.707106781186547,0.,-0.707106781186548));
#14268=DIRECTION('',(-1.,0.,0.));
#14269=DIRECTION('',(0.,0.,-1.));
#14270=DIRECTION('',(1.,0.,0.));
#14271=DIRECTION('',(0.707106781186548,0.,-0.707106781186547));
#14272=DIRECTION('',(0.,0.,1.));
#14273=DIRECTION('',(0.707106781186547,0.,0.707106781186548));
#14274=DIRECTION('',(1.,0.,1.54972587866013E-15));
#14275=DIRECTION('',(-1.10530844287594E-15,0.,1.));
#14276=DIRECTION('',(-1.,0.,-1.83697019872103E-16));
#14277=DIRECTION('',(0.707106781186547,0.,0.707106781186548));
#14278=DIRECTION('',(-6.34909833268504E-16,0.,1.));
#14279=DIRECTION('center_axis',(0.,1.,0.));
#14280=DIRECTION('ref_axis',(-6.4776411278788E-15,0.,-1.));
#14281=DIRECTION('',(-1.,0.,-1.83697019872103E-16));
#14282=DIRECTION('',(0.707106781186548,0.,0.707106781186547));
#14283=DIRECTION('',(1.83697019872103E-16,0.,-1.));
#14284=DIRECTION('',(1.,0.,1.83697019872103E-16));
#14285=DIRECTION('',(-1.83697019872103E-16,0.,1.));
#14286=DIRECTION('',(0.707106781186547,0.,0.707106781186548));
#14287=DIRECTION('',(-1.,0.,0.));
#14288=DIRECTION('',(-0.707106781186548,0.,0.707106781186547));
#14289=DIRECTION('',(-1.48849353870276E-15,0.,1.));
#14290=DIRECTION('',(-1.,0.,-1.04407610291857E-15));
#14291=DIRECTION('',(1.22464679914735E-16,0.,-1.));
#14292=DIRECTION('',(-0.707106781186548,0.,0.707106781186547));
#14293=DIRECTION('',(-0.707106781186548,0.,0.707106781186547));
#14294=DIRECTION('',(0.,0.,-1.));
#14295=DIRECTION('',(-0.707106781186547,0.,-0.707106781186548));
#14296=DIRECTION('',(0.,0.,1.));
#14297=DIRECTION('',(1.,0.,4.94455241362763E-16));
#14298=DIRECTION('center_axis',(0.,-1.,0.));
#14299=DIRECTION('ref_axis',(1.,0.,0.));
#14300=DIRECTION('center_axis',(-4.94455241362763E-16,0.,1.));
#14301=DIRECTION('ref_axis',(1.,0.,4.94455241362763E-16));
#14302=DIRECTION('',(0.,1.,0.));
#14303=DIRECTION('',(1.,0.,4.94455241362763E-16));
#14304=DIRECTION('center_axis',(-1.,0.,0.));
#14305=DIRECTION('ref_axis',(0.,0.,1.));
#14306=DIRECTION('',(0.,1.,0.));
#14307=DIRECTION('',(0.,0.,1.));
#14308=DIRECTION('center_axis',(1.,0.,0.));
#14309=DIRECTION('ref_axis',(0.,0.,-1.));
#14310=DIRECTION('',(0.,1.,0.));
#14311=DIRECTION('',(0.,0.,-1.));
#14312=DIRECTION('',(0.,1.,0.));
#14313=DIRECTION('center_axis',(0.,0.,1.));
#14314=DIRECTION('ref_axis',(1.,0.,0.));
#14315=DIRECTION('',(0.,1.,0.));
#14316=DIRECTION('',(0.,1.,0.));
#14317=DIRECTION('',(1.,0.,0.));
#14318=DIRECTION('center_axis',(-1.,0.,0.));
#14319=DIRECTION('ref_axis',(0.,0.,1.));
#14320=DIRECTION('',(0.,1.,0.));
#14321=DIRECTION('',(0.,0.,1.));
#14322=DIRECTION('',(0.,1.,0.));
#14323=DIRECTION('center_axis',(0.,1.,0.));
#14324=DIRECTION('ref_axis',(1.,0.,0.));
#14325=DIRECTION('',(0.,1.,0.));
#14326=DIRECTION('center_axis',(0.,-1.,0.));
#14327=DIRECTION('ref_axis',(1.,0.,0.));
#14328=DIRECTION('center_axis',(0.,0.,-1.));
#14329=DIRECTION('ref_axis',(-1.,0.,0.));
#14330=DIRECTION('',(0.,1.,0.));
#14331=DIRECTION('',(0.,1.,0.));
#14332=DIRECTION('',(-1.,0.,0.));
#14333=DIRECTION('center_axis',(1.,0.,1.83697019872103E-16));
#14334=DIRECTION('ref_axis',(1.83697019872103E-16,0.,-1.));
#14335=DIRECTION('',(0.,1.,0.));
#14336=DIRECTION('',(1.83697019872103E-16,0.,-1.));
#14337=DIRECTION('',(0.,1.,0.));
#14338=DIRECTION('center_axis',(0.707106781186548,0.,-0.707106781186547));
#14339=DIRECTION('ref_axis',(-0.707106781186547,0.,-0.707106781186548));
#14340=DIRECTION('',(-0.707106781186547,0.,-0.707106781186548));
#14341=DIRECTION('center_axis',(-0.707106781186548,0.,0.707106781186547));
#14342=DIRECTION('ref_axis',(0.707106781186547,0.,0.707106781186548));
#14343=DIRECTION('',(0.707106781186547,0.,0.707106781186548));
#14344=DIRECTION('',(0.,1.,0.));
#14345=DIRECTION('center_axis',(-1.54972587866013E-15,0.,1.));
#14346=DIRECTION('ref_axis',(1.,0.,1.54972587866013E-15));
#14347=DIRECTION('',(1.,0.,1.54972587866013E-15));
#14348=DIRECTION('',(0.,1.,0.));
#14349=DIRECTION('center_axis',(1.,0.,1.10530844287594E-15));
#14350=DIRECTION('ref_axis',(1.10530844287594E-15,0.,-1.));
#14351=DIRECTION('',(1.10530844287594E-15,0.,-1.));
#14352=DIRECTION('',(0.,1.,0.));
#14353=DIRECTION('center_axis',(-1.83697019872103E-16,0.,1.));
#14354=DIRECTION('ref_axis',(1.,0.,1.83697019872103E-16));
#14355=DIRECTION('',(1.,0.,1.83697019872103E-16));
#14356=DIRECTION('',(0.,1.,0.));
#14357=DIRECTION('center_axis',(-0.707106781186548,0.,0.707106781186547));
#14358=DIRECTION('ref_axis',(0.707106781186547,0.,0.707106781186548));
#14359=DIRECTION('',(0.707106781186547,0.,0.707106781186548));
#14360=DIRECTION('',(0.,1.,0.));
#14361=DIRECTION('center_axis',(-1.,0.,-6.34909833268504E-16));
#14362=DIRECTION('ref_axis',(-6.34909833268504E-16,0.,1.));
#14363=DIRECTION('',(-6.34909833268504E-16,0.,1.));
#14364=DIRECTION('',(0.,1.,0.));
#14365=DIRECTION('center_axis',(0.,1.,0.));
#14366=DIRECTION('ref_axis',(-6.4776411278788E-15,0.,-1.));
#14367=DIRECTION('center_axis',(0.,1.,0.));
#14368=DIRECTION('ref_axis',(-6.4776411278788E-15,0.,-1.));
#14369=DIRECTION('',(0.,1.,0.));
#14370=DIRECTION('center_axis',(1.83697019872103E-16,0.,-1.));
#14371=DIRECTION('ref_axis',(-1.,0.,-1.83697019872103E-16));
#14372=DIRECTION('',(-1.,0.,-1.83697019872103E-16));
#14373=DIRECTION('',(0.,1.,0.));
#14374=DIRECTION('center_axis',(0.707106781186547,0.,-0.707106781186548));
#14375=DIRECTION('ref_axis',(-0.707106781186548,0.,-0.707106781186547));
#14376=DIRECTION('',(-0.707106781186548,0.,-0.707106781186547));
#14377=DIRECTION('',(0.,1.,0.));
#14378=DIRECTION('center_axis',(1.,0.,1.83697019872103E-16));
#14379=DIRECTION('ref_axis',(1.83697019872103E-16,0.,-1.));
#14380=DIRECTION('',(1.83697019872103E-16,0.,-1.));
#14381=DIRECTION('',(0.,1.,0.));
#14382=DIRECTION('center_axis',(-1.83697019872103E-16,0.,1.));
#14383=DIRECTION('ref_axis',(1.,0.,1.83697019872103E-16));
#14384=DIRECTION('',(1.,0.,1.83697019872103E-16));
#14385=DIRECTION('center_axis',(-1.,0.,-6.12323399573677E-17));
#14386=DIRECTION('ref_axis',(-6.12323399573677E-17,0.,1.));
#14387=DIRECTION('',(0.,1.,0.));
#14388=DIRECTION('',(-6.12323399573677E-17,0.,1.));
#14389=DIRECTION('',(0.,1.,0.));
#14390=DIRECTION('center_axis',(-0.707106781186548,0.,0.707106781186547));
#14391=DIRECTION('ref_axis',(0.707106781186547,0.,0.707106781186548));
#14392=DIRECTION('',(0.707106781186547,0.,0.707106781186548));
#14393=DIRECTION('center_axis',(0.707106781186548,0.,-0.707106781186547));
#14394=DIRECTION('ref_axis',(-0.707106781186547,0.,-0.707106781186548));
#14395=DIRECTION('',(-0.707106781186547,0.,-0.707106781186548));
#14396=DIRECTION('center_axis',(-6.12323399573677E-17,0.,1.));
#14397=DIRECTION('ref_axis',(1.,0.,6.12323399573677E-17));
#14398=DIRECTION('',(1.,0.,6.12323399573677E-17));
#14399=DIRECTION('',(0.,1.,0.));
#14400=DIRECTION('center_axis',(-0.707106781186547,0.,0.707106781186548));
#14401=DIRECTION('ref_axis',(0.707106781186548,0.,0.707106781186547));
#14402=DIRECTION('',(0.707106781186548,0.,0.707106781186547));
#14403=DIRECTION('',(0.,1.,0.));
#14404=DIRECTION('center_axis',(-1.,0.,-6.12323399573677E-17));
#14405=DIRECTION('ref_axis',(-6.12323399573677E-17,0.,1.));
#14406=DIRECTION('',(-6.12323399573677E-17,0.,1.));
#14407=DIRECTION('',(0.,1.,0.));
#14408=DIRECTION('center_axis',(6.12323399573677E-17,0.,-1.));
#14409=DIRECTION('ref_axis',(-1.,0.,-6.12323399573677E-17));
#14410=DIRECTION('',(-1.,0.,-6.12323399573677E-17));
#14411=DIRECTION('center_axis',(0.,0.,-1.));
#14412=DIRECTION('ref_axis',(-1.,0.,0.));
#14413=DIRECTION('',(0.,1.,0.));
#14414=DIRECTION('',(-1.,0.,0.));
#14415=DIRECTION('',(0.,1.,0.));
#14416=DIRECTION('center_axis',(-0.707106781186547,0.,-0.707106781186548));
#14417=DIRECTION('ref_axis',(-0.707106781186548,0.,0.707106781186547));
#14418=DIRECTION('',(-0.707106781186548,0.,0.707106781186547));
#14419=DIRECTION('center_axis',(0.707106781186547,0.,0.707106781186548));
#14420=DIRECTION('ref_axis',(0.707106781186548,0.,-0.707106781186547));
#14421=DIRECTION('',(0.707106781186548,0.,-0.707106781186547));
#14422=DIRECTION('',(0.,1.,0.));
#14423=DIRECTION('center_axis',(1.,0.,1.36602885878803E-15));
#14424=DIRECTION('ref_axis',(1.36602885878803E-15,0.,-1.));
#14425=DIRECTION('',(1.36602885878803E-15,0.,-1.));
#14426=DIRECTION('',(0.,1.,0.));
#14427=DIRECTION('center_axis',(9.21611423003838E-16,0.,-1.));
#14428=DIRECTION('ref_axis',(-1.,0.,-9.21611423003838E-16));
#14429=DIRECTION('',(-1.,0.,-9.21611423003838E-16));
#14430=DIRECTION('',(0.,1.,0.));
#14431=DIRECTION('center_axis',(1.,0.,0.));
#14432=DIRECTION('ref_axis',(0.,0.,-1.));
#14433=DIRECTION('',(0.,0.,-1.));
#14434=DIRECTION('',(0.,1.,0.));
#14435=DIRECTION('center_axis',(0.707106781186547,0.,0.707106781186548));
#14436=DIRECTION('ref_axis',(0.707106781186548,0.,-0.707106781186547));
#14437=DIRECTION('',(0.707106781186548,0.,-0.707106781186547));
#14438=DIRECTION('',(0.,1.,0.));
#14439=DIRECTION('center_axis',(-4.51212813396402E-16,0.,1.));
#14440=DIRECTION('ref_axis',(1.,0.,4.51212813396402E-16));
#14441=DIRECTION('',(1.,0.,4.51212813396402E-16));
#14442=DIRECTION('',(0.,1.,0.));
#14443=DIRECTION('center_axis',(0.,1.,0.));
#14444=DIRECTION('ref_axis',(-1.,0.,6.6613381477509E-15));
#14445=DIRECTION('center_axis',(0.,1.,0.));
#14446=DIRECTION('ref_axis',(-1.,0.,6.6613381477509E-15));
#14447=DIRECTION('',(0.,1.,0.));
#14448=DIRECTION('center_axis',(-1.,0.,0.));
#14449=DIRECTION('ref_axis',(0.,0.,1.));
#14450=DIRECTION('',(0.,0.,1.));
#14451=DIRECTION('',(0.,1.,0.));
#14452=DIRECTION('center_axis',(-0.707106781186548,0.,-0.707106781186547));
#14453=DIRECTION('ref_axis',(-0.707106781186547,0.,0.707106781186548));
#14454=DIRECTION('',(-0.707106781186547,0.,0.707106781186548));
#14455=DIRECTION('',(0.,1.,0.));
#14456=DIRECTION('center_axis',(0.,0.,-1.));
#14457=DIRECTION('ref_axis',(-1.,0.,0.));
#14458=DIRECTION('',(-1.,0.,0.));
#14459=DIRECTION('',(0.,1.,0.));
#14460=DIRECTION('center_axis',(1.,0.,0.));
#14461=DIRECTION('ref_axis',(0.,0.,-1.));
#14462=DIRECTION('',(0.,0.,-1.));
#14463=DIRECTION('center_axis',(0.707106781186547,0.,0.707106781186548));
#14464=DIRECTION('ref_axis',(0.707106781186548,0.,-0.707106781186547));
#14465=DIRECTION('',(0.707106781186548,0.,-0.707106781186547));
#14466=DIRECTION('center_axis',(-0.707106781186547,0.,-0.707106781186548));
#14467=DIRECTION('ref_axis',(-0.707106781186548,0.,0.707106781186547));
#14468=DIRECTION('',(-0.707106781186548,0.,0.707106781186547));
#14469=DIRECTION('',(0.,1.,0.));
#14470=DIRECTION('center_axis',(-1.,0.,-1.48849353870276E-15));
#14471=DIRECTION('ref_axis',(-1.48849353870276E-15,0.,1.));
#14472=DIRECTION('',(-1.48849353870276E-15,0.,1.));
#14473=DIRECTION('',(0.,1.,0.));
#14474=DIRECTION('center_axis',(-1.04407610291857E-15,0.,1.));
#14475=DIRECTION('ref_axis',(1.,0.,1.04407610291857E-15));
#14476=DIRECTION('',(1.,0.,1.04407610291857E-15));
#14477=DIRECTION('',(0.,1.,0.));
#14478=DIRECTION('center_axis',(-1.,0.,-1.22464679914735E-16));
#14479=DIRECTION('ref_axis',(-1.22464679914735E-16,0.,1.));
#14480=DIRECTION('',(-1.22464679914735E-16,0.,1.));
#14481=DIRECTION('',(0.,1.,0.));
#14482=DIRECTION('center_axis',(-0.707106781186547,0.,-0.707106781186548));
#14483=DIRECTION('ref_axis',(-0.707106781186548,0.,0.707106781186547));
#14484=DIRECTION('',(-0.707106781186548,0.,0.707106781186547));
#14485=DIRECTION('',(0.,1.,0.));
#14486=DIRECTION('center_axis',(5.73677493311137E-16,0.,-1.));
#14487=DIRECTION('ref_axis',(-1.,0.,-5.73677493311137E-16));
#14488=DIRECTION('',(-1.,0.,-5.73677493311137E-16));
#14489=DIRECTION('center_axis',(0.,1.,0.));
#14490=DIRECTION('ref_axis',(-1.,0.,-1.22464679914735E-16));
#14491=DIRECTION('axis',(0.,0.,1.));
#14492=DIRECTION('refdir',(1.,0.,0.));
#14493=DIRECTION('center_axis',(2.24770354660149E-47,-8.64291075969854E-33,
1.));
#14494=DIRECTION('ref_axis',(1.,1.12331423616832E-95,-2.24770354660149E-47));
#14495=DIRECTION('center_axis',(-1.97812547909132E-47,-3.45804190325652E-32,
1.));
#14496=DIRECTION('ref_axis',(1.,-3.6491105917259E-95,1.97812547909132E-47));
#14497=DIRECTION('center_axis',(-2.24770354660149E-47,8.64291075969854E-33,
-1.));
#14498=DIRECTION('ref_axis',(1.,1.94267011675346E-79,-2.24770354660149E-47));
#14499=DIRECTION('center_axis',(0.,0.,1.));
#14500=DIRECTION('ref_axis',(1.,0.,0.));
#14501=DIRECTION('center_axis',(-9.86076131526267E-32,5.23079214264925E-32,
1.));
#14502=DIRECTION('ref_axis',(1.,-4.21761455916246E-79,9.86076131526267E-32));
#14503=DIRECTION('',(0.,0.,-1.));
#14504=DIRECTION('center_axis',(-1.97812547909132E-47,-3.45804190325652E-32,
1.));
#14505=DIRECTION('ref_axis',(1.,-6.84044079659716E-79,1.97812547909132E-47));
#14506=DIRECTION('center_axis',(-1.97812547909132E-47,-3.45804190325652E-32,
1.));
#14507=DIRECTION('ref_axis',(1.,-3.6491105917259E-95,1.97812547909132E-47));
#14508=DIRECTION('center_axis',(-1.97812547909132E-47,-3.45804190325652E-32,
1.));
#14509=DIRECTION('ref_axis',(1.,-6.84044079659716E-79,1.97812547909132E-47));
#14510=DIRECTION('center_axis',(-1.97812547909132E-47,-3.45804190325652E-32,
1.));
#14511=DIRECTION('ref_axis',(1.,-3.6491105917259E-95,1.97812547909132E-47));
#14512=DIRECTION('center_axis',(-1.97812547909132E-47,-3.45804190325652E-32,
1.));
#14513=DIRECTION('ref_axis',(1.,-3.6491105917259E-95,1.97812547909132E-47));
#14514=DIRECTION('center_axis',(0.,0.,1.));
#14515=DIRECTION('ref_axis',(1.,0.,0.));
#14516=DIRECTION('',(0.,0.,-1.));
#14517=DIRECTION('center_axis',(-1.97812547909132E-47,-3.45804190325652E-32,
1.));
#14518=DIRECTION('ref_axis',(1.,-6.84044079659716E-79,1.97812547909132E-47));
#14519=DIRECTION('center_axis',(0.,0.,1.));
#14520=DIRECTION('ref_axis',(1.,0.,0.));
#14521=DIRECTION('',(0.,0.,-1.));
#14522=DIRECTION('center_axis',(-1.97812547909132E-47,-3.45804190325652E-32,
1.));
#14523=DIRECTION('ref_axis',(1.,-3.6491105917259E-95,1.97812547909132E-47));
#14524=DIRECTION('center_axis',(1.97812547909132E-47,3.45804190325652E-32,
-1.));
#14525=DIRECTION('ref_axis',(1.,-6.84044079659716E-79,1.97812547909132E-47));
#14526=DIRECTION('center_axis',(0.,0.,1.));
#14527=DIRECTION('ref_axis',(1.,0.,0.));
#14528=DIRECTION('',(0.,0.,1.));
#14529=DIRECTION('axis',(0.,0.,1.));
#14530=DIRECTION('refdir',(1.,0.,0.));
#14531=DIRECTION('center_axis',(7.40148683083437E-16,0.,-1.));
#14532=DIRECTION('ref_axis',(-1.,0.,-7.40148683083437E-16));
#14533=DIRECTION('center_axis',(-5.73677493311137E-16,1.09476442525376E-47,
1.));
#14534=DIRECTION('ref_axis',(-1.,4.74333763175827E-79,-5.73677493311137E-16));
#14535=DIRECTION('',(7.40148683083437E-16,0.,-1.));
#14536=DIRECTION('center_axis',(-5.73677493311137E-16,1.09476442525376E-47,
1.));
#14537=DIRECTION('ref_axis',(-1.,4.74333763175827E-79,-5.73677493311137E-16));
#14538=DIRECTION('center_axis',(-1.,0.,-7.40148683083437E-16));
#14539=DIRECTION('ref_axis',(0.,1.,0.));
#14540=DIRECTION('',(0.,1.,0.));
#14541=DIRECTION('',(7.40148683083437E-16,0.,-1.));
#14542=DIRECTION('',(0.,1.,0.));
#14543=DIRECTION('',(7.40148683083437E-16,0.,-1.));
#14544=DIRECTION('center_axis',(0.,1.,0.));
#14545=DIRECTION('ref_axis',(1.,0.,5.73677493311137E-16));
#14546=DIRECTION('',(1.,0.,5.73677493311137E-16));
#14547=DIRECTION('',(1.,0.,5.73677493311137E-16));
#14548=DIRECTION('',(7.40148683083437E-16,0.,-1.));
#14549=DIRECTION('center_axis',(1.,-3.55020428439413E-33,7.40148683083437E-16));
#14550=DIRECTION('ref_axis',(1.22343830028454E-32,-1.,-2.13262384275027E-17));
#14551=DIRECTION('',(1.22343830028454E-32,-1.,-2.13262384275027E-17));
#14552=DIRECTION('',(1.22343830028454E-32,-1.,-2.13262384275027E-17));
#14553=DIRECTION('',(7.40148683083437E-16,0.,-1.));
#14554=DIRECTION('center_axis',(0.,-1.,0.));
#14555=DIRECTION('ref_axis',(-1.,0.,-4.75766751584917E-16));
#14556=DIRECTION('',(-1.,0.,-4.75766751584917E-16));
#14557=DIRECTION('',(-1.,0.,-4.75766751584917E-16));
#14558=DIRECTION('center_axis',(-1.,0.,-7.40148683083437E-16));
#14559=DIRECTION('ref_axis',(0.,1.,0.));
#14560=DIRECTION('',(0.,1.,0.));
#14561=DIRECTION('',(7.40148683083437E-16,0.,-1.));
#14562=DIRECTION('',(0.,1.,0.));
#14563=DIRECTION('',(7.40148683083437E-16,0.,-1.));
#14564=DIRECTION('center_axis',(0.,1.,0.));
#14565=DIRECTION('ref_axis',(1.,0.,5.73677493311137E-16));
#14566=DIRECTION('',(1.,0.,5.73677493311137E-16));
#14567=DIRECTION('',(1.,0.,5.73677493311137E-16));
#14568=DIRECTION('',(7.40148683083437E-16,0.,-1.));
#14569=DIRECTION('center_axis',(1.,-3.55020428439413E-33,7.40148683083437E-16));
#14570=DIRECTION('ref_axis',(1.22343830028454E-32,-1.,-2.13262384275027E-17));
#14571=DIRECTION('',(1.22343830028454E-32,-1.,-2.13262384275027E-17));
#14572=DIRECTION('',(1.22343830028454E-32,-1.,-2.13262384275027E-17));
#14573=DIRECTION('',(7.40148683083437E-16,0.,-1.));
#14574=DIRECTION('center_axis',(0.,-1.,0.));
#14575=DIRECTION('ref_axis',(-1.,0.,-4.75766751584917E-16));
#14576=DIRECTION('',(-1.,0.,-4.75766751584917E-16));
#14577=DIRECTION('',(-1.,0.,-4.75766751584917E-16));
#14578=DIRECTION('center_axis',(7.40148683083437E-16,0.,-1.));
#14579=DIRECTION('ref_axis',(-1.,0.,-7.40148683083437E-16));
#14580=DIRECTION('center_axis',(-5.73677493311137E-16,1.09476442525376E-47,
1.));
#14581=DIRECTION('ref_axis',(-1.,4.74333763175827E-79,-5.73677493311137E-16));
#14582=DIRECTION('',(7.40148683083437E-16,0.,-1.));
#14583=DIRECTION('center_axis',(-5.73677493311137E-16,1.09476442525376E-47,
1.));
#14584=DIRECTION('ref_axis',(-1.,4.74333763175827E-79,-5.73677493311137E-16));
#14585=DIRECTION('center_axis',(7.40148683083437E-16,0.,-1.));
#14586=DIRECTION('ref_axis',(-1.,0.,-7.40148683083437E-16));
#14587=DIRECTION('center_axis',(-5.73677493311137E-16,1.09476442525376E-47,
1.));
#14588=DIRECTION('ref_axis',(-1.,4.74333763175827E-79,-5.73677493311137E-16));
#14589=DIRECTION('',(7.40148683083437E-16,0.,-1.));
#14590=DIRECTION('center_axis',(-5.73677493311137E-16,1.09476442525376E-47,
1.));
#14591=DIRECTION('ref_axis',(-1.,4.74333763175827E-79,-5.73677493311137E-16));
#14592=DIRECTION('center_axis',(-1.,0.,-7.40148683083437E-16));
#14593=DIRECTION('ref_axis',(0.,1.,0.));
#14594=DIRECTION('',(0.,1.,0.));
#14595=DIRECTION('',(7.40148683083437E-16,0.,-1.));
#14596=DIRECTION('',(0.,1.,0.));
#14597=DIRECTION('',(7.40148683083437E-16,0.,-1.));
#14598=DIRECTION('center_axis',(0.,1.,0.));
#14599=DIRECTION('ref_axis',(1.,0.,5.73677493311137E-16));
#14600=DIRECTION('',(1.,0.,5.73677493311137E-16));
#14601=DIRECTION('',(1.,0.,5.73677493311137E-16));
#14602=DIRECTION('',(7.40148683083437E-16,0.,-1.));
#14603=DIRECTION('center_axis',(1.,-3.55020428439413E-33,7.40148683083437E-16));
#14604=DIRECTION('ref_axis',(1.22343830028454E-32,-1.,-2.13262384275027E-17));
#14605=DIRECTION('',(1.22343830028454E-32,-1.,-2.13262384275027E-17));
#14606=DIRECTION('',(1.22343830028454E-32,-1.,-2.13262384275027E-17));
#14607=DIRECTION('',(7.40148683083437E-16,0.,-1.));
#14608=DIRECTION('center_axis',(0.,-1.,0.));
#14609=DIRECTION('ref_axis',(-1.,0.,-4.75766751584917E-16));
#14610=DIRECTION('',(-1.,0.,-4.75766751584917E-16));
#14611=DIRECTION('',(-1.,0.,-4.75766751584917E-16));
#14612=DIRECTION('center_axis',(7.40148683083437E-16,0.,-1.));
#14613=DIRECTION('ref_axis',(-1.,0.,-7.40148683083437E-16));
#14614=DIRECTION('center_axis',(-5.73677493311137E-16,1.09476442525376E-47,
1.));
#14615=DIRECTION('ref_axis',(-1.,4.74333763175827E-79,-5.73677493311137E-16));
#14616=DIRECTION('',(7.40148683083437E-16,0.,-1.));
#14617=DIRECTION('center_axis',(-5.73677493311137E-16,1.09476442525376E-47,
1.));
#14618=DIRECTION('ref_axis',(-1.,4.74333763175827E-79,-5.73677493311137E-16));
#14619=DIRECTION('center_axis',(7.40148683083437E-16,0.,-1.));
#14620=DIRECTION('ref_axis',(-1.,0.,-7.40148683083437E-16));
#14621=DIRECTION('center_axis',(-5.73677493311137E-16,1.09476442525376E-47,
1.));
#14622=DIRECTION('ref_axis',(-1.,4.74333763175827E-79,-5.73677493311137E-16));
#14623=DIRECTION('',(7.40148683083437E-16,0.,-1.));
#14624=DIRECTION('center_axis',(-5.73677493311137E-16,1.09476442525376E-47,
1.));
#14625=DIRECTION('ref_axis',(-1.,4.74333763175827E-79,-5.73677493311137E-16));
#14626=DIRECTION('center_axis',(0.,1.,0.));
#14627=DIRECTION('ref_axis',(1.,0.,5.73677493311137E-16));
#14628=DIRECTION('',(-1.,0.,-5.73677493311137E-16));
#14629=DIRECTION('',(7.40148683083437E-16,0.,-1.));
#14630=DIRECTION('',(1.,0.,5.73677493311137E-16));
#14631=DIRECTION('',(7.40148683083437E-16,0.,-1.));
#14632=DIRECTION('center_axis',(-1.,3.69640295643904E-34,-7.40148683083437E-16));
#14633=DIRECTION('ref_axis',(-1.27381992356653E-33,1.,2.22044604925031E-18));
#14634=DIRECTION('',(1.27381992356654E-33,-1.,-2.22044604925031E-18));
#14635=DIRECTION('',(-1.27381992356654E-33,1.,2.22044604925031E-18));
#14636=DIRECTION('',(7.40148683083437E-16,0.,-1.));
#14637=DIRECTION('center_axis',(0.,1.,0.));
#14638=DIRECTION('ref_axis',(1.,0.,3.77856009858697E-16));
#14639=DIRECTION('',(-1.,0.,-3.77856009858697E-16));
#14640=DIRECTION('',(1.,0.,3.77856009858697E-16));
#14641=DIRECTION('',(7.40148683083437E-16,0.,-1.));
#14642=DIRECTION('center_axis',(1.,2.22044604925031E-18,7.40148683083437E-16));
#14643=DIRECTION('ref_axis',(2.22044604925031E-18,-1.,1.27381992356654E-33));
#14644=DIRECTION('',(-2.22044604925031E-18,1.,-1.27381992356654E-33));
#14645=DIRECTION('',(2.22044604925031E-18,-1.,1.27381992356654E-33));
#14646=DIRECTION('',(7.40148683083437E-16,0.,-1.));
#14647=DIRECTION('center_axis',(0.,1.,0.));
#14648=DIRECTION('ref_axis',(1.,0.,5.73677493311137E-16));
#14649=DIRECTION('',(-1.,0.,-5.73677493311137E-16));
#14650=DIRECTION('',(1.,0.,5.73677493311137E-16));
#14651=DIRECTION('',(7.40148683083437E-16,0.,-1.));
#14652=DIRECTION('center_axis',(-1.,0.,-7.40148683083437E-16));
#14653=DIRECTION('ref_axis',(0.,1.,0.));
#14654=DIRECTION('',(0.,-1.,0.));
#14655=DIRECTION('',(0.,1.,0.));
#14656=DIRECTION('',(7.40148683083437E-16,0.,-1.));
#14657=DIRECTION('center_axis',(0.,1.,0.));
#14658=DIRECTION('ref_axis',(1.,0.,5.73677493311137E-16));
#14659=DIRECTION('',(-1.,0.,-5.73677493311137E-16));
#14660=DIRECTION('',(1.,0.,5.73677493311137E-16));
#14661=DIRECTION('',(7.40148683083437E-16,0.,-1.));
#14662=DIRECTION('center_axis',(1.,0.,7.40148683083437E-16));
#14663=DIRECTION('ref_axis',(0.,-1.,0.));
#14664=DIRECTION('',(0.,1.,0.));
#14665=DIRECTION('',(0.,-1.,0.));
#14666=DIRECTION('',(7.40148683083437E-16,0.,-1.));
#14667=DIRECTION('center_axis',(0.,1.,0.));
#14668=DIRECTION('ref_axis',(1.,0.,5.73677493311137E-16));
#14669=DIRECTION('',(-1.,0.,-5.73677493311137E-16));
#14670=DIRECTION('',(1.,0.,5.73677493311137E-16));
#14671=DIRECTION('',(7.40148683083437E-16,0.,-1.));
#14672=DIRECTION('center_axis',(7.40148683083437E-16,0.,-1.));
#14673=DIRECTION('ref_axis',(-1.,0.,-7.40148683083437E-16));
#14674=DIRECTION('center_axis',(5.73677493311137E-16,0.,-1.));
#14675=DIRECTION('ref_axis',(-1.,0.,-5.73677493311137E-16));
#14676=DIRECTION('center_axis',(5.73677493311137E-16,0.,-1.));
#14677=DIRECTION('ref_axis',(-1.,0.,-5.73677493311137E-16));
#14678=DIRECTION('',(7.40148683083437E-16,0.,-1.));
#14679=DIRECTION('center_axis',(-1.,0.,-7.40148683083437E-16));
#14680=DIRECTION('ref_axis',(0.,1.,0.));
#14681=DIRECTION('',(0.,-1.,0.));
#14682=DIRECTION('',(0.,1.,0.));
#14683=DIRECTION('',(7.40148683083437E-16,0.,-1.));
#14684=DIRECTION('center_axis',(7.40148683083437E-16,0.,-1.));
#14685=DIRECTION('ref_axis',(-8.88178419700122E-16,-1.,-6.57384087684173E-31));
#14686=DIRECTION('center_axis',(5.73677493311137E-16,0.,-1.));
#14687=DIRECTION('ref_axis',(-8.88178419700122E-16,-1.,-5.09527969426613E-31));
#14688=DIRECTION('center_axis',(5.73677493311137E-16,0.,-1.));
#14689=DIRECTION('ref_axis',(-8.88178419700122E-16,-1.,-5.09527969426613E-31));
#14690=DIRECTION('',(7.40148683083437E-16,0.,-1.));
#14691=DIRECTION('center_axis',(3.63363534449E-16,-1.,2.6894304150297E-31));
#14692=DIRECTION('ref_axis',(-1.,-3.63363534449E-16,-5.73677493311137E-16));
#14693=DIRECTION('',(1.,3.63363534449E-16,5.73677493311137E-16));
#14694=DIRECTION('',(-1.,-3.63363534449E-16,-5.73677493311137E-16));
#14695=DIRECTION('',(7.40148683083437E-16,0.,-1.));
#14696=DIRECTION('center_axis',(7.40148683083437E-16,0.,-1.));
#14697=DIRECTION('ref_axis',(1.,-1.77635683940025E-15,7.40148683083437E-16));
#14698=DIRECTION('center_axis',(5.73677493311137E-16,0.,-1.));
#14699=DIRECTION('ref_axis',(1.,-1.77635683940025E-15,5.73677493311137E-16));
#14700=DIRECTION('center_axis',(5.73677493311137E-16,0.,-1.));
#14701=DIRECTION('ref_axis',(1.,-1.77635683940025E-15,5.73677493311137E-16));
#14702=DIRECTION('',(7.40148683083437E-16,0.,-1.));
#14703=DIRECTION('center_axis',(1.,0.,7.40148683083437E-16));
#14704=DIRECTION('ref_axis',(0.,-1.,0.));
#14705=DIRECTION('',(0.,1.,0.));
#14706=DIRECTION('',(0.,-1.,0.));
#14707=DIRECTION('',(7.40148683083437E-16,0.,-1.));
#14708=DIRECTION('center_axis',(7.40148683083437E-16,0.,-1.));
#14709=DIRECTION('ref_axis',(-8.88178419700127E-16,1.,-6.57384087684177E-31));
#14710=DIRECTION('center_axis',(5.73677493311137E-16,0.,-1.));
#14711=DIRECTION('ref_axis',(-8.88178419700127E-16,1.,-5.09527969426616E-31));
#14712=DIRECTION('center_axis',(5.73677493311137E-16,0.,-1.));
#14713=DIRECTION('ref_axis',(-8.88178419700127E-16,1.,-5.09527969426616E-31));
#14714=DIRECTION('center_axis',(5.73677493311137E-16,0.,-1.));
#14715=DIRECTION('ref_axis',(-1.,0.,-5.73677493311137E-16));
#14716=DIRECTION('center_axis',(5.73677493311137E-16,0.,-1.));
#14717=DIRECTION('ref_axis',(-1.,0.,-5.73677493311137E-16));
#14718=DIRECTION('axis',(0.,0.,1.));
#14719=DIRECTION('refdir',(1.,0.,0.));
#14720=DIRECTION('center_axis',(-1.,0.,0.));
#14721=DIRECTION('ref_axis',(0.,1.,0.));
#14722=DIRECTION('',(-1.,0.,0.));
#14723=DIRECTION('center_axis',(-1.,0.,0.));
#14724=DIRECTION('ref_axis',(0.,1.,0.));
#14725=DIRECTION('',(-1.,0.,0.));
#14726=DIRECTION('center_axis',(0.,0.,1.));
#14727=DIRECTION('ref_axis',(1.,0.,0.));
#14728=DIRECTION('center_axis',(2.24770354660149E-47,-8.64291075969854E-33,
1.));
#14729=DIRECTION('ref_axis',(1.,1.94267011675346E-79,-2.24770354660149E-47));
#14730=DIRECTION('',(0.,0.,-1.));
#14731=DIRECTION('',(0.,0.,-1.));
#14732=DIRECTION('center_axis',(1.97812547909132E-47,3.45804190325652E-32,
-1.));
#14733=DIRECTION('ref_axis',(1.,-6.84044079659716E-79,1.97812547909132E-47));
#14734=DIRECTION('center_axis',(2.24770354660149E-47,-8.64291075969854E-33,
1.));
#14735=DIRECTION('ref_axis',(1.,1.12331423616832E-95,-2.24770354660149E-47));
#14736=DIRECTION('center_axis',(-2.24770354660149E-47,8.64291075969854E-33,
-1.));
#14737=DIRECTION('ref_axis',(1.,1.94267011675346E-79,-2.24770354660149E-47));
#14738=DIRECTION('center_axis',(-1.97812547909132E-47,-3.45804190325652E-32,
1.));
#14739=DIRECTION('ref_axis',(1.,-3.6491105917259E-95,1.97812547909132E-47));
#14740=DIRECTION('center_axis',(-1.97812547909132E-47,-3.45804190325652E-32,
1.));
#14741=DIRECTION('ref_axis',(1.,-3.6491105917259E-95,1.97812547909132E-47));
#14742=DIRECTION('center_axis',(-9.86076131526267E-32,5.23079214264925E-32,
1.));
#14743=DIRECTION('ref_axis',(1.,-4.21761455916246E-79,9.86076131526267E-32));
#14744=DIRECTION('center_axis',(0.,0.,1.));
#14745=DIRECTION('ref_axis',(1.,0.,0.));
#14746=DIRECTION('center_axis',(-1.97812547909132E-47,-3.45804190325652E-32,
1.));
#14747=DIRECTION('ref_axis',(1.,-3.6491105917259E-95,1.97812547909132E-47));
#14748=DIRECTION('',(0.,0.,-1.));
#14749=DIRECTION('center_axis',(-1.97812547909132E-47,-3.45804190325652E-32,
1.));
#14750=DIRECTION('ref_axis',(1.,-3.6491105917259E-95,1.97812547909132E-47));
#14751=DIRECTION('center_axis',(0.,0.,1.));
#14752=DIRECTION('ref_axis',(1.,0.,0.));
#14753=DIRECTION('',(0.,0.,-1.));
#14754=DIRECTION('center_axis',(1.97812547909132E-47,3.45804190325652E-32,
-1.));
#14755=DIRECTION('ref_axis',(1.,-6.84044079659716E-79,1.97812547909132E-47));
#14756=DIRECTION('center_axis',(0.,0.,1.));
#14757=DIRECTION('ref_axis',(1.,0.,0.));
#14758=DIRECTION('center_axis',(-7.78296498900683E-47,-2.83123199421538E-32,
-1.));
#14759=DIRECTION('ref_axis',(1.,3.60769778730949E-95,-7.78296498900683E-47));
#14760=DIRECTION('',(0.,0.,1.));
#14761=DIRECTION('',(0.,0.,1.));
#14762=DIRECTION('center_axis',(0.,0.,1.));
#14763=DIRECTION('ref_axis',(1.,0.,0.));
#14764=DIRECTION('center_axis',(-1.97812547909132E-47,-3.45804190325652E-32,
1.));
#14765=DIRECTION('ref_axis',(1.,-3.6491105917259E-95,1.97812547909132E-47));
#14766=DIRECTION('',(0.,0.,-1.));
#14767=DIRECTION('center_axis',(-1.97812547909132E-47,-3.45804190325652E-32,
1.));
#14768=DIRECTION('ref_axis',(1.,-3.6491105917259E-95,1.97812547909132E-47));
#14769=DIRECTION('center_axis',(-1.97812547909132E-47,-3.45804190325652E-32,
1.));
#14770=DIRECTION('ref_axis',(1.,-3.6491105917259E-95,1.97812547909132E-47));
#14771=DIRECTION('center_axis',(-1.97812547909132E-47,-3.45804190325652E-32,
1.));
#14772=DIRECTION('ref_axis',(1.,-3.6491105917259E-95,1.97812547909132E-47));
#14773=DIRECTION('axis',(0.,0.,1.));
#14774=DIRECTION('refdir',(1.,0.,0.));
#14775=DIRECTION('center_axis',(0.,0.,1.));
#14776=DIRECTION('ref_axis',(1.,0.,0.));
#14777=DIRECTION('center_axis',(0.,0.,-1.));
#14778=DIRECTION('ref_axis',(-1.,-1.54465812121761E-15,0.));
#14779=DIRECTION('',(0.,1.,0.));
#14780=DIRECTION('center_axis',(0.,0.,-1.));
#14781=DIRECTION('ref_axis',(1.,0.,0.));
#14782=DIRECTION('',(1.00381828627953E-18,-1.,0.));
#14783=DIRECTION('center_axis',(0.,0.,1.));
#14784=DIRECTION('ref_axis',(-1.,-1.86984930463184E-15,0.));
#14785=DIRECTION('',(0.,1.,0.));
#14786=DIRECTION('center_axis',(0.,0.,1.));
#14787=DIRECTION('ref_axis',(1.,0.,0.));
#14788=DIRECTION('',(0.,-1.,0.));
#14789=DIRECTION('center_axis',(-1.,0.,0.));
#14790=DIRECTION('ref_axis',(0.,-1.,0.));
#14791=DIRECTION('',(0.,0.,-1.));
#14792=DIRECTION('',(0.,-1.,0.));
#14793=DIRECTION('',(0.,0.,1.));
#14794=DIRECTION('center_axis',(0.,0.,1.));
#14795=DIRECTION('ref_axis',(1.,0.,0.));
#14796=DIRECTION('center_axis',(0.,0.,-1.));
#14797=DIRECTION('ref_axis',(1.,0.,0.));
#14798=DIRECTION('',(0.,0.,1.));
#14799=DIRECTION('center_axis',(1.,0.,0.));
#14800=DIRECTION('ref_axis',(0.,1.,0.));
#14801=DIRECTION('',(0.,1.,0.));
#14802=DIRECTION('',(0.,0.,1.));
#14803=DIRECTION('center_axis',(0.,0.,1.));
#14804=DIRECTION('ref_axis',(-1.,-1.86984930463184E-15,0.));
#14805=DIRECTION('center_axis',(0.,0.,-1.));
#14806=DIRECTION('ref_axis',(-1.,-1.86984930463184E-15,0.));
#14807=DIRECTION('center_axis',(-1.,0.,0.));
#14808=DIRECTION('ref_axis',(0.,-1.,0.));
#14809=DIRECTION('',(0.,0.,-1.));
#14810=DIRECTION('',(0.,-1.,0.));
#14811=DIRECTION('',(0.,0.,1.));
#14812=DIRECTION('center_axis',(0.,0.,1.));
#14813=DIRECTION('ref_axis',(1.,0.,0.));
#14814=DIRECTION('center_axis',(0.,0.,1.));
#14815=DIRECTION('ref_axis',(1.,0.,0.));
#14816=DIRECTION('',(0.,0.,1.));
#14817=DIRECTION('center_axis',(1.,1.00381828627953E-18,0.));
#14818=DIRECTION('ref_axis',(-1.00381828627953E-18,1.,0.));
#14819=DIRECTION('',(-1.00381828627953E-18,1.,0.));
#14820=DIRECTION('',(0.,0.,1.));
#14821=DIRECTION('center_axis',(0.,0.,1.));
#14822=DIRECTION('ref_axis',(-1.,-1.54465812121761E-15,0.));
#14823=DIRECTION('center_axis',(0.,0.,1.));
#14824=DIRECTION('ref_axis',(-1.,-1.54465812121761E-15,0.));
#14825=DIRECTION('center_axis',(0.,0.,1.));
#14826=DIRECTION('ref_axis',(1.,0.,0.));
#14827=DIRECTION('axis',(0.,0.,1.));
#14828=DIRECTION('refdir',(1.,0.,0.));
#14829=DIRECTION('center_axis',(-1.,0.,0.));
#14830=DIRECTION('ref_axis',(0.,-1.,0.));
#14831=DIRECTION('center_axis',(1.,0.,0.));
#14832=DIRECTION('ref_axis',(0.,-1.,0.));
#14833=DIRECTION('',(-1.,0.,0.));
#14834=DIRECTION('center_axis',(1.,0.,0.));
#14835=DIRECTION('ref_axis',(0.,-1.,0.));
#14836=DIRECTION('center_axis',(0.,1.,0.));
#14837=DIRECTION('ref_axis',(0.,0.,-1.));
#14838=DIRECTION('',(0.,0.,-1.));
#14839=DIRECTION('',(-1.,0.,0.));
#14840=DIRECTION('',(0.,0.,-1.));
#14841=DIRECTION('',(-1.,0.,0.));
#14842=DIRECTION('center_axis',(-1.,0.,0.));
#14843=DIRECTION('ref_axis',(0.,-1.,0.));
#14844=DIRECTION('center_axis',(1.,0.,0.));
#14845=DIRECTION('ref_axis',(0.,-1.,0.));
#14846=DIRECTION('center_axis',(1.,0.,0.));
#14847=DIRECTION('ref_axis',(0.,-1.,0.));
#14848=DIRECTION('',(-1.,0.,0.));
#14849=DIRECTION('center_axis',(0.,-1.,0.));
#14850=DIRECTION('ref_axis',(0.,0.,1.));
#14851=DIRECTION('',(0.,0.,1.));
#14852=DIRECTION('',(0.,0.,1.));
#14853=DIRECTION('',(-1.,0.,0.));
#14854=DIRECTION('center_axis',(-1.,0.,0.));
#14855=DIRECTION('ref_axis',(0.,1.,0.));
#14856=DIRECTION('center_axis',(1.,0.,0.));
#14857=DIRECTION('ref_axis',(0.,1.,0.));
#14858=DIRECTION('center_axis',(1.,0.,0.));
#14859=DIRECTION('ref_axis',(0.,1.,0.));
#14860=DIRECTION('center_axis',(-1.,0.,0.));
#14861=DIRECTION('ref_axis',(0.,-1.,0.));
#14862=DIRECTION('center_axis',(1.,0.,0.));
#14863=DIRECTION('ref_axis',(0.,-1.,0.));
#14864=DIRECTION('',(-1.,0.,0.));
#14865=DIRECTION('center_axis',(1.,0.,0.));
#14866=DIRECTION('ref_axis',(0.,-1.,0.));
#14867=DIRECTION('center_axis',(-1.,0.,0.));
#14868=DIRECTION('ref_axis',(0.,-1.,0.));
#14869=DIRECTION('center_axis',(1.,0.,0.));
#14870=DIRECTION('ref_axis',(0.,-1.,0.));
#14871=DIRECTION('',(-1.,0.,0.));
#14872=DIRECTION('center_axis',(1.,0.,0.));
#14873=DIRECTION('ref_axis',(0.,-1.,0.));
#14874=DIRECTION('center_axis',(-1.,0.,0.));
#14875=DIRECTION('ref_axis',(0.,-1.,0.));
#14876=DIRECTION('center_axis',(1.,0.,0.));
#14877=DIRECTION('ref_axis',(0.,-1.,0.));
#14878=DIRECTION('',(-1.,0.,0.));
#14879=DIRECTION('center_axis',(1.,0.,0.));
#14880=DIRECTION('ref_axis',(0.,-1.,0.));
#14881=DIRECTION('center_axis',(-1.,0.,0.));
#14882=DIRECTION('ref_axis',(0.,-1.,0.));
#14883=DIRECTION('center_axis',(1.,0.,0.));
#14884=DIRECTION('ref_axis',(0.,-1.,0.));
#14885=DIRECTION('',(-1.,0.,0.));
#14886=DIRECTION('center_axis',(1.,0.,0.));
#14887=DIRECTION('ref_axis',(0.,-1.,0.));
#14888=DIRECTION('center_axis',(-1.,0.,0.));
#14889=DIRECTION('ref_axis',(0.,-1.,0.));
#14890=DIRECTION('center_axis',(1.,0.,0.));
#14891=DIRECTION('ref_axis',(0.,-1.,0.));
#14892=DIRECTION('',(-1.,0.,0.));
#14893=DIRECTION('center_axis',(1.,0.,0.));
#14894=DIRECTION('ref_axis',(0.,-1.,0.));
#14895=DIRECTION('center_axis',(0.,1.,0.));
#14896=DIRECTION('ref_axis',(0.,0.,-1.));
#14897=DIRECTION('',(0.,0.,-1.));
#14898=DIRECTION('',(-1.,0.,0.));
#14899=DIRECTION('',(0.,0.,-1.));
#14900=DIRECTION('',(-1.,0.,0.));
#14901=DIRECTION('center_axis',(-1.,0.,0.));
#14902=DIRECTION('ref_axis',(0.,-1.,0.));
#14903=DIRECTION('center_axis',(1.,0.,0.));
#14904=DIRECTION('ref_axis',(0.,-1.,0.));
#14905=DIRECTION('center_axis',(1.,0.,0.));
#14906=DIRECTION('ref_axis',(0.,-1.,0.));
#14907=DIRECTION('',(-1.,0.,0.));
#14908=DIRECTION('center_axis',(0.,-1.,0.));
#14909=DIRECTION('ref_axis',(0.,0.,1.));
#14910=DIRECTION('',(0.,0.,1.));
#14911=DIRECTION('',(0.,0.,1.));
#14912=DIRECTION('',(-1.,0.,0.));
#14913=DIRECTION('center_axis',(-1.,0.,0.));
#14914=DIRECTION('ref_axis',(0.,1.,0.));
#14915=DIRECTION('center_axis',(1.,0.,0.));
#14916=DIRECTION('ref_axis',(0.,1.,0.));
#14917=DIRECTION('center_axis',(1.,0.,0.));
#14918=DIRECTION('ref_axis',(0.,1.,0.));
#14919=DIRECTION('center_axis',(0.,1.,0.));
#14920=DIRECTION('ref_axis',(0.,0.,-1.));
#14921=DIRECTION('',(0.,0.,-1.));
#14922=DIRECTION('',(-1.,0.,0.));
#14923=DIRECTION('',(0.,0.,-1.));
#14924=DIRECTION('',(-1.,0.,0.));
#14925=DIRECTION('center_axis',(-1.,0.,0.));
#14926=DIRECTION('ref_axis',(0.,-1.,0.));
#14927=DIRECTION('center_axis',(1.,0.,0.));
#14928=DIRECTION('ref_axis',(0.,-1.,0.));
#14929=DIRECTION('center_axis',(1.,0.,0.));
#14930=DIRECTION('ref_axis',(0.,-1.,0.));
#14931=DIRECTION('',(-1.,0.,0.));
#14932=DIRECTION('center_axis',(0.,-1.,0.));
#14933=DIRECTION('ref_axis',(0.,0.,1.));
#14934=DIRECTION('',(0.,0.,1.));
#14935=DIRECTION('',(0.,0.,1.));
#14936=DIRECTION('',(-1.,0.,0.));
#14937=DIRECTION('center_axis',(-1.,0.,0.));
#14938=DIRECTION('ref_axis',(0.,1.,0.));
#14939=DIRECTION('center_axis',(1.,0.,0.));
#14940=DIRECTION('ref_axis',(0.,1.,0.));
#14941=DIRECTION('center_axis',(1.,0.,0.));
#14942=DIRECTION('ref_axis',(0.,1.,0.));
#14943=DIRECTION('center_axis',(-1.,0.,0.));
#14944=DIRECTION('ref_axis',(0.,-1.,0.));
#14945=DIRECTION('center_axis',(1.,0.,0.));
#14946=DIRECTION('ref_axis',(0.,-1.,0.));
#14947=DIRECTION('',(-1.,0.,0.));
#14948=DIRECTION('center_axis',(1.,0.,0.));
#14949=DIRECTION('ref_axis',(0.,-1.,0.));
#14950=DIRECTION('center_axis',(-1.,0.,0.));
#14951=DIRECTION('ref_axis',(0.,-1.,0.));
#14952=DIRECTION('center_axis',(1.,0.,0.));
#14953=DIRECTION('ref_axis',(0.,-1.,0.));
#14954=DIRECTION('',(-1.,0.,0.));
#14955=DIRECTION('center_axis',(1.,0.,0.));
#14956=DIRECTION('ref_axis',(0.,-1.,0.));
#14957=DIRECTION('center_axis',(-1.,0.,0.));
#14958=DIRECTION('ref_axis',(0.,-1.,0.));
#14959=DIRECTION('center_axis',(1.,0.,0.));
#14960=DIRECTION('ref_axis',(0.,-1.,0.));
#14961=DIRECTION('',(-1.,0.,0.));
#14962=DIRECTION('center_axis',(1.,0.,0.));
#14963=DIRECTION('ref_axis',(0.,-1.,0.));
#14964=DIRECTION('center_axis',(-1.,0.,0.));
#14965=DIRECTION('ref_axis',(0.,-1.,0.));
#14966=DIRECTION('center_axis',(1.,0.,0.));
#14967=DIRECTION('ref_axis',(0.,-1.,0.));
#14968=DIRECTION('',(-1.,0.,0.));
#14969=DIRECTION('center_axis',(1.,0.,0.));
#14970=DIRECTION('ref_axis',(0.,-1.,0.));
#14971=DIRECTION('center_axis',(-1.,0.,0.));
#14972=DIRECTION('ref_axis',(0.,-1.,0.));
#14973=DIRECTION('center_axis',(1.,0.,0.));
#14974=DIRECTION('ref_axis',(0.,-1.,0.));
#14975=DIRECTION('',(-1.,0.,0.));
#14976=DIRECTION('center_axis',(1.,0.,0.));
#14977=DIRECTION('ref_axis',(0.,-1.,0.));
#14978=DIRECTION('center_axis',(0.,-1.,0.));
#14979=DIRECTION('ref_axis',(0.,0.,1.));
#14980=DIRECTION('',(0.,0.,1.));
#14981=DIRECTION('',(-1.,0.,0.));
#14982=DIRECTION('',(0.,0.,1.));
#14983=DIRECTION('',(-1.,0.,0.));
#14984=DIRECTION('center_axis',(-1.,0.,0.));
#14985=DIRECTION('ref_axis',(0.,1.,0.));
#14986=DIRECTION('center_axis',(1.,0.,0.));
#14987=DIRECTION('ref_axis',(0.,1.,0.));
#14988=DIRECTION('center_axis',(1.,0.,0.));
#14989=DIRECTION('ref_axis',(0.,1.,0.));
#14990=DIRECTION('',(-1.,0.,0.));
#14991=DIRECTION('center_axis',(0.,1.,0.));
#14992=DIRECTION('ref_axis',(0.,0.,-1.));
#14993=DIRECTION('',(0.,0.,-1.));
#14994=DIRECTION('',(0.,0.,-1.));
#14995=DIRECTION('',(-1.,0.,0.));
#14996=DIRECTION('center_axis',(-1.,0.,0.));
#14997=DIRECTION('ref_axis',(0.,-1.,0.));
#14998=DIRECTION('center_axis',(1.,0.,0.));
#14999=DIRECTION('ref_axis',(0.,-1.,0.));
#15000=DIRECTION('center_axis',(1.,0.,0.));
#15001=DIRECTION('ref_axis',(0.,-1.,0.));
#15002=DIRECTION('center_axis',(-1.,0.,0.));
#15003=DIRECTION('ref_axis',(0.,-1.,0.));
#15004=DIRECTION('center_axis',(1.,0.,0.));
#15005=DIRECTION('ref_axis',(0.,-1.,0.));
#15006=DIRECTION('',(-1.,0.,0.));
#15007=DIRECTION('center_axis',(1.,0.,0.));
#15008=DIRECTION('ref_axis',(0.,-1.,0.));
#15009=DIRECTION('center_axis',(-1.,0.,0.));
#15010=DIRECTION('ref_axis',(0.,-1.,0.));
#15011=DIRECTION('center_axis',(1.,0.,0.));
#15012=DIRECTION('ref_axis',(0.,-1.,0.));
#15013=DIRECTION('',(-1.,0.,0.));
#15014=DIRECTION('center_axis',(1.,0.,0.));
#15015=DIRECTION('ref_axis',(0.,-1.,0.));
#15016=DIRECTION('center_axis',(0.,1.,0.));
#15017=DIRECTION('ref_axis',(0.,0.,-1.));
#15018=DIRECTION('',(0.,0.,-1.));
#15019=DIRECTION('',(-1.,0.,0.));
#15020=DIRECTION('',(0.,0.,-1.));
#15021=DIRECTION('',(-1.,0.,0.));
#15022=DIRECTION('center_axis',(-1.,0.,0.));
#15023=DIRECTION('ref_axis',(0.,-1.,0.));
#15024=DIRECTION('center_axis',(1.,0.,0.));
#15025=DIRECTION('ref_axis',(0.,-1.,0.));
#15026=DIRECTION('center_axis',(1.,0.,0.));
#15027=DIRECTION('ref_axis',(0.,-1.,0.));
#15028=DIRECTION('',(-1.,0.,0.));
#15029=DIRECTION('center_axis',(0.,-1.,0.));
#15030=DIRECTION('ref_axis',(0.,0.,1.));
#15031=DIRECTION('',(0.,0.,1.));
#15032=DIRECTION('',(0.,0.,1.));
#15033=DIRECTION('',(-1.,0.,0.));
#15034=DIRECTION('center_axis',(-1.,0.,0.));
#15035=DIRECTION('ref_axis',(0.,1.,0.));
#15036=DIRECTION('center_axis',(1.,0.,0.));
#15037=DIRECTION('ref_axis',(0.,1.,0.));
#15038=DIRECTION('center_axis',(1.,0.,0.));
#15039=DIRECTION('ref_axis',(0.,1.,0.));
#15040=DIRECTION('center_axis',(0.,-1.,0.));
#15041=DIRECTION('ref_axis',(0.,0.,1.));
#15042=DIRECTION('',(0.,0.,1.));
#15043=DIRECTION('',(-1.,0.,0.));
#15044=DIRECTION('',(0.,0.,1.));
#15045=DIRECTION('',(-1.,0.,0.));
#15046=DIRECTION('center_axis',(-1.,0.,0.));
#15047=DIRECTION('ref_axis',(0.,1.,0.));
#15048=DIRECTION('center_axis',(1.,0.,0.));
#15049=DIRECTION('ref_axis',(0.,1.,0.));
#15050=DIRECTION('center_axis',(1.,0.,0.));
#15051=DIRECTION('ref_axis',(0.,1.,0.));
#15052=DIRECTION('',(-1.,0.,0.));
#15053=DIRECTION('center_axis',(0.,1.,0.));
#15054=DIRECTION('ref_axis',(0.,0.,-1.));
#15055=DIRECTION('',(0.,0.,-1.));
#15056=DIRECTION('',(0.,0.,-1.));
#15057=DIRECTION('',(-1.,0.,0.));
#15058=DIRECTION('center_axis',(-1.,0.,0.));
#15059=DIRECTION('ref_axis',(0.,-1.,0.));
#15060=DIRECTION('center_axis',(1.,0.,0.));
#15061=DIRECTION('ref_axis',(0.,-1.,0.));
#15062=DIRECTION('center_axis',(1.,0.,0.));
#15063=DIRECTION('ref_axis',(0.,-1.,0.));
#15064=DIRECTION('center_axis',(0.,1.,0.));
#15065=DIRECTION('ref_axis',(0.,0.,-1.));
#15066=DIRECTION('',(0.,0.,-1.));
#15067=DIRECTION('',(-1.,0.,0.));
#15068=DIRECTION('',(0.,0.,-1.));
#15069=DIRECTION('',(-1.,0.,0.));
#15070=DIRECTION('center_axis',(-1.,0.,0.));
#15071=DIRECTION('ref_axis',(0.,-1.,0.));
#15072=DIRECTION('center_axis',(1.,0.,0.));
#15073=DIRECTION('ref_axis',(0.,-1.,0.));
#15074=DIRECTION('center_axis',(1.,0.,0.));
#15075=DIRECTION('ref_axis',(0.,-1.,0.));
#15076=DIRECTION('',(-1.,0.,0.));
#15077=DIRECTION('center_axis',(0.,-1.,0.));
#15078=DIRECTION('ref_axis',(0.,0.,1.));
#15079=DIRECTION('',(0.,0.,1.));
#15080=DIRECTION('',(0.,0.,1.));
#15081=DIRECTION('',(-1.,0.,0.));
#15082=DIRECTION('center_axis',(-1.,0.,0.));
#15083=DIRECTION('ref_axis',(0.,1.,0.));
#15084=DIRECTION('center_axis',(1.,0.,0.));
#15085=DIRECTION('ref_axis',(0.,1.,0.));
#15086=DIRECTION('center_axis',(1.,0.,0.));
#15087=DIRECTION('ref_axis',(0.,1.,0.));
#15088=DIRECTION('center_axis',(0.,1.,0.));
#15089=DIRECTION('ref_axis',(0.,0.,-1.));
#15090=DIRECTION('',(0.,0.,-1.));
#15091=DIRECTION('',(-1.,0.,0.));
#15092=DIRECTION('',(0.,0.,-1.));
#15093=DIRECTION('',(-1.,0.,0.));
#15094=DIRECTION('center_axis',(-1.,0.,0.));
#15095=DIRECTION('ref_axis',(0.,-1.,0.));
#15096=DIRECTION('center_axis',(1.,0.,0.));
#15097=DIRECTION('ref_axis',(0.,-1.,0.));
#15098=DIRECTION('center_axis',(1.,0.,0.));
#15099=DIRECTION('ref_axis',(0.,-1.,0.));
#15100=DIRECTION('',(-1.,0.,0.));
#15101=DIRECTION('center_axis',(0.,-1.,0.));
#15102=DIRECTION('ref_axis',(0.,0.,1.));
#15103=DIRECTION('',(0.,0.,1.));
#15104=DIRECTION('',(0.,0.,1.));
#15105=DIRECTION('',(-1.,0.,0.));
#15106=DIRECTION('center_axis',(-1.,0.,0.));
#15107=DIRECTION('ref_axis',(0.,1.,0.));
#15108=DIRECTION('center_axis',(1.,0.,0.));
#15109=DIRECTION('ref_axis',(0.,1.,0.));
#15110=DIRECTION('center_axis',(1.,0.,0.));
#15111=DIRECTION('ref_axis',(0.,1.,0.));
#15112=DIRECTION('center_axis',(-1.,0.,0.));
#15113=DIRECTION('ref_axis',(0.,-1.,0.));
#15114=DIRECTION('center_axis',(1.,0.,0.));
#15115=DIRECTION('ref_axis',(0.,-1.,0.));
#15116=DIRECTION('',(-1.,0.,0.));
#15117=DIRECTION('center_axis',(1.,0.,0.));
#15118=DIRECTION('ref_axis',(0.,-1.,0.));
#15119=DIRECTION('center_axis',(-1.,0.,0.));
#15120=DIRECTION('ref_axis',(0.,-1.,0.));
#15121=DIRECTION('center_axis',(1.,0.,0.));
#15122=DIRECTION('ref_axis',(0.,-1.,0.));
#15123=DIRECTION('',(-1.,0.,0.));
#15124=DIRECTION('center_axis',(1.,0.,0.));
#15125=DIRECTION('ref_axis',(0.,-1.,0.));
#15126=DIRECTION('center_axis',(0.,1.49175803335835E-16,-1.));
#15127=DIRECTION('ref_axis',(0.,-1.,-1.49175803335835E-16));
#15128=DIRECTION('',(0.,1.,1.49175803335835E-16));
#15129=DIRECTION('',(-1.,0.,0.));
#15130=DIRECTION('',(0.,-1.,-1.49175803335835E-16));
#15131=DIRECTION('',(-1.,0.,0.));
#15132=DIRECTION('center_axis',(-1.,0.,0.));
#15133=DIRECTION('ref_axis',(0.,1.,-1.18423789293348E-14));
#15134=DIRECTION('center_axis',(-1.,0.,0.));
#15135=DIRECTION('ref_axis',(0.,1.,-1.18423789293348E-14));
#15136=DIRECTION('center_axis',(-1.,0.,0.));
#15137=DIRECTION('ref_axis',(0.,1.,-1.18423789293348E-14));
#15138=DIRECTION('',(-1.,0.,0.));
#15139=DIRECTION('center_axis',(0.,1.,0.));
#15140=DIRECTION('ref_axis',(0.,0.,-1.));
#15141=DIRECTION('',(0.,0.,1.));
#15142=DIRECTION('',(0.,0.,-1.));
#15143=DIRECTION('',(-1.,0.,0.));
#15144=DIRECTION('center_axis',(-1.,0.,0.));
#15145=DIRECTION('ref_axis',(0.,1.18423789293349E-14,1.));
#15146=DIRECTION('center_axis',(-1.,0.,0.));
#15147=DIRECTION('ref_axis',(0.,1.18423789293349E-14,1.));
#15148=DIRECTION('center_axis',(-1.,0.,0.));
#15149=DIRECTION('ref_axis',(0.,1.18423789293349E-14,1.));
#15150=DIRECTION('',(-1.,0.,0.));
#15151=DIRECTION('center_axis',(0.,0.,1.));
#15152=DIRECTION('ref_axis',(0.,1.,0.));
#15153=DIRECTION('',(0.,-1.,0.));
#15154=DIRECTION('',(0.,1.,0.));
#15155=DIRECTION('',(-1.,0.,0.));
#15156=DIRECTION('center_axis',(-1.,0.,0.));
#15157=DIRECTION('ref_axis',(0.,-1.,1.18423789293348E-14));
#15158=DIRECTION('center_axis',(-1.,0.,0.));
#15159=DIRECTION('ref_axis',(0.,-1.,1.18423789293348E-14));
#15160=DIRECTION('center_axis',(-1.,0.,0.));
#15161=DIRECTION('ref_axis',(0.,-1.,1.18423789293348E-14));
#15162=DIRECTION('',(-1.,0.,0.));
#15163=DIRECTION('center_axis',(0.,-1.,0.));
#15164=DIRECTION('ref_axis',(0.,0.,1.));
#15165=DIRECTION('',(0.,0.,-1.));
#15166=DIRECTION('',(0.,0.,1.));
#15167=DIRECTION('',(-1.,0.,0.));
#15168=DIRECTION('center_axis',(-1.,0.,0.));
#15169=DIRECTION('ref_axis',(0.,-1.18423789293348E-14,-1.));
#15170=DIRECTION('center_axis',(-1.,0.,0.));
#15171=DIRECTION('ref_axis',(0.,-1.18423789293348E-14,-1.));
#15172=DIRECTION('center_axis',(-1.,0.,0.));
#15173=DIRECTION('ref_axis',(0.,-1.18423789293348E-14,-1.));
#15174=DIRECTION('center_axis',(-1.,0.,0.));
#15175=DIRECTION('ref_axis',(0.,-1.,0.));
#15176=DIRECTION('center_axis',(-1.,0.,0.));
#15177=DIRECTION('ref_axis',(0.,-1.,0.));
#15178=DIRECTION('axis',(0.,0.,1.));
#15179=DIRECTION('refdir',(1.,0.,0.));
#15180=DIRECTION('center_axis',(0.,0.,-1.));
#15181=DIRECTION('ref_axis',(1.,0.,0.));
#15182=DIRECTION('center_axis',(0.,0.,-1.));
#15183=DIRECTION('ref_axis',(1.,0.,0.));
#15184=DIRECTION('',(0.,0.,-1.));
#15185=DIRECTION('center_axis',(0.,0.,1.));
#15186=DIRECTION('ref_axis',(1.,0.,0.));
#15187=DIRECTION('center_axis',(0.,0.,-1.));
#15188=DIRECTION('ref_axis',(1.,0.,0.));
#15189=DIRECTION('center_axis',(0.,0.,-1.));
#15190=DIRECTION('ref_axis',(1.,0.,0.));
#15191=DIRECTION('',(0.,0.,-1.));
#15192=DIRECTION('center_axis',(0.,0.,1.));
#15193=DIRECTION('ref_axis',(1.,0.,0.));
#15194=DIRECTION('center_axis',(0.,0.,-1.));
#15195=DIRECTION('ref_axis',(1.,0.,0.));
#15196=DIRECTION('center_axis',(0.,-1.13806187638273E-62,-1.));
#15197=DIRECTION('ref_axis',(1.,0.,0.));
#15198=DIRECTION('',(0.,0.,-1.));
#15199=DIRECTION('center_axis',(0.,1.13806187638273E-62,1.));
#15200=DIRECTION('ref_axis',(1.,0.,0.));
#15201=DIRECTION('center_axis',(0.,0.,-1.));
#15202=DIRECTION('ref_axis',(1.,0.,0.));
#15203=DIRECTION('center_axis',(0.,0.,-1.));
#15204=DIRECTION('ref_axis',(1.,0.,0.));
#15205=DIRECTION('',(0.,0.,-1.));
#15206=DIRECTION('center_axis',(0.,0.,1.));
#15207=DIRECTION('ref_axis',(1.,0.,0.));
#15208=DIRECTION('center_axis',(0.,0.,-1.));
#15209=DIRECTION('ref_axis',(1.,0.,0.));
#15210=DIRECTION('center_axis',(0.,0.,-1.));
#15211=DIRECTION('ref_axis',(1.,0.,0.));
#15212=DIRECTION('',(0.,0.,-1.));
#15213=DIRECTION('center_axis',(0.,0.,1.));
#15214=DIRECTION('ref_axis',(1.,0.,0.));
#15215=DIRECTION('center_axis',(0.,0.,-1.));
#15216=DIRECTION('ref_axis',(-1.,1.42108547152022E-14,0.));
#15217=DIRECTION('center_axis',(-1.98364274472311E-31,1.40137711657962E-17,
1.));
#15218=DIRECTION('ref_axis',(-1.,1.42108547152022E-14,-3.97511940521531E-31));
#15219=DIRECTION('',(0.,0.,-1.));
#15220=DIRECTION('center_axis',(1.98364274472311E-31,-1.40137711657962E-17,
-1.));
#15221=DIRECTION('ref_axis',(-1.,1.42108547152022E-14,-3.97511940521531E-31));
#15222=DIRECTION('',(0.,0.,-1.));
#15223=DIRECTION('center_axis',(2.368475785867E-15,-1.,0.));
#15224=DIRECTION('ref_axis',(-1.,-2.368475785867E-15,4.56151843855735E-49));
#15225=DIRECTION('',(-1.,-2.368475785867E-15,4.56151843855735E-49));
#15226=DIRECTION('',(-1.,-2.368475785867E-15,4.56151843855735E-49));
#15227=DIRECTION('',(0.,0.,-1.));
#15228=DIRECTION('center_axis',(0.,0.,-1.));
#15229=DIRECTION('ref_axis',(8.88178419700138E-16,-1.,0.));
#15230=DIRECTION('center_axis',(-5.36441819030946E-47,1.60253698400202E-32,
1.));
#15231=DIRECTION('ref_axis',(8.88178419700138E-16,-1.,1.60253698400202E-32));
#15232=DIRECTION('center_axis',(5.36441819030946E-47,-1.60253698400202E-32,
-1.));
#15233=DIRECTION('ref_axis',(8.88178419700138E-16,-1.,1.60253698400202E-32));
#15234=DIRECTION('',(0.,0.,-1.));
#15235=DIRECTION('center_axis',(1.,-6.41527552355446E-17,0.));
#15236=DIRECTION('ref_axis',(-6.41527552355446E-17,-1.,6.85517916879725E-33));
#15237=DIRECTION('',(-6.41527552355446E-17,-1.,6.85517916879725E-33));
#15238=DIRECTION('',(-6.41527552355446E-17,-1.,6.85517916879725E-33));
#15239=DIRECTION('',(0.,0.,-1.));
#15240=DIRECTION('center_axis',(0.,0.,-1.));
#15241=DIRECTION('ref_axis',(1.,1.4210854715202E-14,0.));
#15242=DIRECTION('center_axis',(-5.55111512312578E-17,-3.88267476788466E-31,
1.));
#15243=DIRECTION('ref_axis',(1.,1.4210854715202E-14,5.55111512312578E-17));
#15244=DIRECTION('center_axis',(5.55111512312578E-17,3.88267476788466E-31,
-1.));
#15245=DIRECTION('ref_axis',(1.,1.4210854715202E-14,5.55111512312578E-17));
#15246=DIRECTION('',(0.,0.,-1.));
#15247=DIRECTION('center_axis',(0.,1.,0.));
#15248=DIRECTION('ref_axis',(1.,0.,1.8503717077086E-17));
#15249=DIRECTION('',(1.,0.,1.8503717077086E-17));
#15250=DIRECTION('',(1.,0.,1.8503717077086E-17));
#15251=DIRECTION('',(0.,0.,-1.));
#15252=DIRECTION('center_axis',(0.,0.,-1.));
#15253=DIRECTION('ref_axis',(0.,1.,0.));
#15254=DIRECTION('center_axis',(-2.77555756156289E-17,2.8027542331593E-17,
1.));
#15255=DIRECTION('ref_axis',(0.,1.,-2.8027542331593E-17));
#15256=DIRECTION('center_axis',(2.77555756156289E-17,-2.8027542331593E-17,
-1.));
#15257=DIRECTION('ref_axis',(0.,1.,-2.8027542331593E-17));
#15258=DIRECTION('',(0.,0.,-1.));
#15259=DIRECTION('center_axis',(-1.,-3.20763776177723E-16,0.));
#15260=DIRECTION('ref_axis',(-3.20763776177723E-16,1.,-1.30015623442515E-17));
#15261=DIRECTION('',(-3.20763776177723E-16,1.,-1.30015623442515E-17));
#15262=DIRECTION('',(-3.20763776177723E-16,1.,-1.30015623442515E-17));
#15263=DIRECTION('center_axis',(-1.8503717077086E-17,0.,1.));
#15264=DIRECTION('ref_axis',(1.,0.,1.8503717077086E-17));
#15265=DIRECTION('center_axis',(-1.8503717077086E-17,0.,1.));
#15266=DIRECTION('ref_axis',(1.,0.,1.8503717077086E-17));
#15267=DIRECTION('axis',(0.,0.,1.));
#15268=DIRECTION('refdir',(1.,0.,0.));
#15269=DIRECTION('center_axis',(2.75333173930341E-16,0.,1.));
#15270=DIRECTION('ref_axis',(-1.,0.,2.75333173930341E-16));
#15271=DIRECTION('center_axis',(2.75333173930341E-16,0.,1.));
#15272=DIRECTION('ref_axis',(-1.,0.,2.75333173930341E-16));
#15273=DIRECTION('',(-0.740512347492959,-9.06866076086345E-17,-0.672042754004882));
#15274=DIRECTION('center_axis',(-2.75333173930341E-16,0.,-1.));
#15275=DIRECTION('ref_axis',(-1.,0.,2.75333173930341E-16));
#15276=DIRECTION('center_axis',(-2.75333173930341E-16,0.,-1.));
#15277=DIRECTION('ref_axis',(-1.,0.,2.72638525605195E-16));
#15278=DIRECTION('center_axis',(2.75333173930341E-16,0.,1.));
#15279=DIRECTION('ref_axis',(-1.,0.,2.75333173930341E-16));
#15280=DIRECTION('center_axis',(1.22464679914735E-16,1.,-3.37185890152874E-32));
#15281=DIRECTION('ref_axis',(1.,-1.22464679914735E-16,-2.79941343255335E-16));
#15282=DIRECTION('center_axis',(-2.75333173930341E-16,0.,-1.));
#15283=DIRECTION('ref_axis',(-1.,0.,2.75333173930341E-16));
#15284=DIRECTION('center_axis',(-2.75333173930341E-16,0.,-1.));
#15285=DIRECTION('ref_axis',(-1.,0.,2.75333173930341E-16));
#15286=DIRECTION('center_axis',(-2.75333173930341E-16,0.,-1.));
#15287=DIRECTION('ref_axis',(1.,0.,-2.75333173930341E-16));
#15288=DIRECTION('center_axis',(-2.75333173930341E-16,0.,-1.));
#15289=DIRECTION('ref_axis',(-1.,0.,2.75333173930341E-16));
#15290=DIRECTION('',(2.75333173930341E-16,0.,1.));
#15291=DIRECTION('center_axis',(0.0435778713738291,-0.0754790873051733,
-0.996194698091746));
#15292=DIRECTION('ref_axis',(-0.866025403784439,-0.5,-3.35810244624808E-17));
#15293=DIRECTION('',(0.,0.997141949694316,-0.0755508581011305));
#15294=DIRECTION('',(-0.866025403784439,-0.5,0.));
#15295=DIRECTION('',(-0.863550259614423,0.498570974847158,-0.0755508581011305));
#15296=DIRECTION('center_axis',(0.0871557427476581,0.,-0.996194698091746));
#15297=DIRECTION('ref_axis',(0.,-1.,0.));
#15298=DIRECTION('',(0.,-1.,0.));
#15299=DIRECTION('',(-0.863550259614423,-0.498570974847158,-0.0755508581011305));
#15300=DIRECTION('center_axis',(0.0435778713738291,0.0754790873051733,-0.996194698091746));
#15301=DIRECTION('ref_axis',(0.866025403784439,-0.5,3.35810244624808E-17));
#15302=DIRECTION('',(0.866025403784439,-0.5,0.));
#15303=DIRECTION('',(-1.59381164582915E-16,-0.997141949694316,-0.0755508581011305));
#15304=DIRECTION('center_axis',(-0.0435778713738291,0.0754790873051733,
-0.996194698091746));
#15305=DIRECTION('ref_axis',(0.866025403784439,0.5,-3.35810244624808E-17));
#15306=DIRECTION('',(0.866025403784439,0.5,0.));
#15307=DIRECTION('',(0.863550259614423,-0.498570974847159,-0.0755508581011305));
#15308=DIRECTION('center_axis',(-0.0871557427476581,5.58657470692638E-17,
-0.996194698091746));
#15309=DIRECTION('ref_axis',(6.40987562127855E-16,1.,-3.92662944814522E-32));
#15310=DIRECTION('',(6.40987562127855E-16,1.,0.));
#15311=DIRECTION('',(0.863550259614423,0.498570974847158,-0.0755508581011305));
#15312=DIRECTION('center_axis',(-0.0435778713738291,-0.0754790873051733,
-0.996194698091746));
#15313=DIRECTION('ref_axis',(-0.866025403784439,0.5,3.35810244624808E-17));
#15314=DIRECTION('',(-0.866025403784439,0.5,0.));
#15315=DIRECTION('center_axis',(0.5,-0.866025403784439,0.));
#15316=DIRECTION('ref_axis',(-0.866025403784439,-0.5,0.));
#15317=DIRECTION('',(-0.866025403784439,-0.5,2.38445523128275E-16));
#15318=DIRECTION('',(0.,0.,-1.));
#15319=DIRECTION('',(0.,0.,-1.));
#15320=DIRECTION('center_axis',(1.,0.,0.));
#15321=DIRECTION('ref_axis',(0.,-1.,0.));
#15322=DIRECTION('',(0.,-1.,0.));
#15323=DIRECTION('',(0.,0.,-1.));
#15324=DIRECTION('center_axis',(0.5,0.866025403784439,0.));
#15325=DIRECTION('ref_axis',(0.866025403784439,-0.5,0.));
#15326=DIRECTION('',(0.866025403784439,-0.5,-2.38445523128275E-16));
#15327=DIRECTION('',(0.,0.,-1.));
#15328=DIRECTION('center_axis',(-0.5,0.866025403784439,0.));
#15329=DIRECTION('ref_axis',(0.866025403784439,0.5,0.));
#15330=DIRECTION('',(0.866025403784439,0.5,-2.38445523128275E-16));
#15331=DIRECTION('',(0.,0.,-1.));
#15332=DIRECTION('center_axis',(-1.,6.40987562127855E-16,0.));
#15333=DIRECTION('ref_axis',(6.40987562127855E-16,1.,0.));
#15334=DIRECTION('',(6.40987562127855E-16,1.,-1.76485139930534E-31));
#15335=DIRECTION('',(0.,0.,-1.));
#15336=DIRECTION('center_axis',(-0.5,-0.866025403784439,0.));
#15337=DIRECTION('ref_axis',(-0.866025403784439,0.5,0.));
#15338=DIRECTION('',(-0.866025403784439,0.5,2.38445523128275E-16));
#15339=DIRECTION('center_axis',(-2.75333173930341E-16,0.,-1.));
#15340=DIRECTION('ref_axis',(-1.,0.,2.75333173930341E-16));
#15341=DIRECTION('center_axis',(2.75333173930341E-16,0.,1.));
#15342=DIRECTION('ref_axis',(1.,0.,-2.75333173930341E-16));
#15343=DIRECTION('center_axis',(-2.75333173930341E-16,0.,-1.));
#15344=DIRECTION('ref_axis',(1.,0.,-2.75333173930341E-16));
#15345=DIRECTION('center_axis',(1.22464679914735E-16,0.,1.));
#15346=DIRECTION('ref_axis',(1.,0.,-8.59318587050222E-17));
#15347=DIRECTION('center_axis',(1.22464679914735E-16,-1.,-7.49879891330929E-33));
#15348=DIRECTION('ref_axis',(-1.,-1.22464679914735E-16,5.37074116906389E-17));
#15349=DIRECTION('',(5.06731490694329E-16,1.32513649906846E-15,1.));
#15350=DIRECTION('',(1.,-1.47104550762833E-14,-5.06731490694309E-16));
#15351=DIRECTION('',(-1.,1.22464679914735E-16,0.));
#15352=DIRECTION('',(0.,0.,1.));
#15353=DIRECTION('',(0.,0.,1.));
#15354=DIRECTION('',(1.,0.,0.));
#15355=DIRECTION('',(0.,0.,1.));
#15356=DIRECTION('',(1.,0.,0.));
#15357=DIRECTION('',(0.,0.,1.));
#15358=DIRECTION('',(1.,0.,0.));
#15359=DIRECTION('',(0.,0.,1.));
#15360=DIRECTION('',(1.,0.,0.));
#15361=DIRECTION('',(0.,0.,1.));
#15362=DIRECTION('',(1.,0.,0.));
#15363=DIRECTION('',(0.,0.,1.));
#15364=DIRECTION('',(1.,0.,0.));
#15365=DIRECTION('',(0.,0.,1.));
#15366=DIRECTION('',(1.,0.,0.));
#15367=DIRECTION('',(0.,0.,1.));
#15368=DIRECTION('',(1.,0.,0.));
#15369=DIRECTION('',(0.,0.,1.));
#15370=DIRECTION('',(1.,0.,0.));
#15371=DIRECTION('',(0.,0.,1.));
#15372=DIRECTION('',(1.,0.,0.));
#15373=DIRECTION('',(0.,0.,1.));
#15374=DIRECTION('',(1.,0.,0.));
#15375=DIRECTION('',(-1.,1.22464679914735E-16,0.));
#15376=DIRECTION('',(0.,0.,1.));
#15377=DIRECTION('',(-1.,1.22464679914735E-16,0.));
#15378=DIRECTION('',(0.,0.,1.));
#15379=DIRECTION('',(-1.,1.22464679914735E-16,0.));
#15380=DIRECTION('',(0.,0.,1.));
#15381=CARTESIAN_POINT('',(0.,0.,0.));
#15382=CARTESIAN_POINT('',(0.,0.,0.));
#15383=CARTESIAN_POINT('Origin',(15.5,15.5,-45.9992561210692));
#15384=CARTESIAN_POINT('',(12.325,15.5,-33.844));
#15385=CARTESIAN_POINT('Origin',(15.5,15.5,-33.844));
#15386=CARTESIAN_POINT('',(12.325,15.5,-34.479));
#15387=CARTESIAN_POINT('',(12.325,15.5,-45.9992561210692));
#15388=CARTESIAN_POINT('',(18.675,15.5,-34.479));
#15389=CARTESIAN_POINT('Origin',(15.5,15.5,-34.479));
#15390=CARTESIAN_POINT('Origin',(15.5,15.5,-34.479));
#15391=CARTESIAN_POINT('Origin',(15.5,15.5,-34.479));
#15392=CARTESIAN_POINT('',(17.913,15.1825,-35.6336740328739));
#15393=CARTESIAN_POINT('',(17.913,15.5,-35.6429742265188));
#15394=CARTESIAN_POINT('Ctrl Pts',(17.913,15.5,-35.6429742265188));
#15395=CARTESIAN_POINT('Ctrl Pts',(17.913,15.3977178848389,-35.6429742265188));
#15396=CARTESIAN_POINT('Ctrl Pts',(17.913,15.2910620631233,-35.6401598997242));
#15397=CARTESIAN_POINT('Ctrl Pts',(17.913,15.1824999999999,-35.6336740328742));
#15398=CARTESIAN_POINT('Origin',(17.405,15.5,-34.479));
#15399=CARTESIAN_POINT('',(17.913,15.8175,-35.6336740328742));
#15400=CARTESIAN_POINT('Ctrl Pts',(17.913,15.8175000000001,-35.6336740328742));
#15401=CARTESIAN_POINT('Ctrl Pts',(17.913,15.7089379368767,-35.6401598997242));
#15402=CARTESIAN_POINT('Ctrl Pts',(17.913,15.6022821151611,-35.6429742265188));
#15403=CARTESIAN_POINT('Ctrl Pts',(17.913,15.5,-35.6429742265188));
#15404=CARTESIAN_POINT('',(17.3783553311341,15.8175,-35.749));
#15405=CARTESIAN_POINT('Origin',(17.3559153980514,15.8175,-34.4373099752802));
#15406=CARTESIAN_POINT('',(15.8175,17.3783553311341,-35.749));
#15407=CARTESIAN_POINT('Origin',(15.5,15.5,-35.749));
#15408=CARTESIAN_POINT('',(15.8175,17.913,-35.6336740328739));
#15409=CARTESIAN_POINT('Origin',(15.8175000000003,17.3559153980479,-34.4373099752707));
#15410=CARTESIAN_POINT('',(15.1825,17.913,-35.633674032875));
#15411=CARTESIAN_POINT('Ctrl Pts',(15.8175,17.913,-35.6336740328742));
#15412=CARTESIAN_POINT('Ctrl Pts',(15.7089379368767,17.913,-35.6401598997242));
#15413=CARTESIAN_POINT('Ctrl Pts',(15.6022821151611,17.913,-35.6429742265188));
#15414=CARTESIAN_POINT('Ctrl Pts',(15.3977178848389,17.913,-35.6429742265188));
#15415=CARTESIAN_POINT('Ctrl Pts',(15.2910620631233,17.913,-35.6401598997242));
#15416=CARTESIAN_POINT('Ctrl Pts',(15.1825,17.913,-35.6336740328742));
#15417=CARTESIAN_POINT('',(15.1825,17.3783553311341,-35.749));
#15418=CARTESIAN_POINT('Origin',(15.1825000000009,17.3559153980454,-34.4373099752573));
#15419=CARTESIAN_POINT('',(13.6216446688659,15.8175,-35.749));
#15420=CARTESIAN_POINT('Origin',(15.5,15.5,-35.749));
#15421=CARTESIAN_POINT('',(13.087,15.8175,-35.6336740328739));
#15422=CARTESIAN_POINT('Origin',(13.6451071230427,15.8175000000003,-34.4325038145077));
#15423=CARTESIAN_POINT('',(13.087,15.1825,-35.6336740328739));
#15424=CARTESIAN_POINT('Ctrl Pts',(13.087,15.1825,-35.6336740328742));
#15425=CARTESIAN_POINT('Ctrl Pts',(13.087,15.2910620631233,-35.6401598997242));
#15426=CARTESIAN_POINT('Ctrl Pts',(13.087,15.3977178848389,-35.6429742265188));
#15427=CARTESIAN_POINT('Ctrl Pts',(13.087,15.6022821151611,-35.6429742265188));
#15428=CARTESIAN_POINT('Ctrl Pts',(13.087,15.7089379368767,-35.6401598997242));
#15429=CARTESIAN_POINT('Ctrl Pts',(13.087,15.8175,-35.6336740328742));
#15430=CARTESIAN_POINT('',(13.6216446688659,15.1825,-35.749));
#15431=CARTESIAN_POINT('Origin',(13.6451071230429,15.1824999999997,-34.4325038145053));
#15432=CARTESIAN_POINT('',(15.1825,13.6216446688659,-35.749));
#15433=CARTESIAN_POINT('Origin',(15.5,15.5,-35.749));
#15434=CARTESIAN_POINT('',(15.1825,13.087,-35.6336740328739));
#15435=CARTESIAN_POINT('Origin',(15.1824999999996,13.6451071230448,-34.4325038144978));
#15436=CARTESIAN_POINT('',(15.8175,13.087,-35.633674032875));
#15437=CARTESIAN_POINT('Ctrl Pts',(15.1825,13.087,-35.6336740328742));
#15438=CARTESIAN_POINT('Ctrl Pts',(15.2910620631233,13.087,-35.6401598997242));
#15439=CARTESIAN_POINT('Ctrl Pts',(15.3977178848389,13.087,-35.6429742265188));
#15440=CARTESIAN_POINT('Ctrl Pts',(15.6022821151611,13.087,-35.6429742265188));
#15441=CARTESIAN_POINT('Ctrl Pts',(15.7089379368767,13.087,-35.6401598997242));
#15442=CARTESIAN_POINT('Ctrl Pts',(15.8175,13.087,-35.6336740328742));
#15443=CARTESIAN_POINT('',(15.8175,13.6216446688659,-35.749));
#15444=CARTESIAN_POINT('Origin',(15.8174999999991,13.6451071230564,-34.4325038144518));
#15445=CARTESIAN_POINT('',(17.3783553311341,15.1825,-35.749));
#15446=CARTESIAN_POINT('Origin',(15.5,15.5,-35.749));
#15447=CARTESIAN_POINT('Origin',(17.3559153980526,15.1824999999996,-34.4373099752921));
#15448=CARTESIAN_POINT('Origin',(0.,0.,-35.749));
#15449=CARTESIAN_POINT('',(15.1825,15.8175,-35.749));
#15450=CARTESIAN_POINT('',(15.1825,17.913,-35.749));
#15451=CARTESIAN_POINT('',(17.913,15.8175,-35.749));
#15452=CARTESIAN_POINT('Origin',(0.,0.,-35.749));
#15453=CARTESIAN_POINT('',(15.1825,15.1825,-35.749));
#15454=CARTESIAN_POINT('',(17.913,15.1825,-35.749));
#15455=CARTESIAN_POINT('',(15.1825,17.913,-35.749));
#15456=CARTESIAN_POINT('Origin',(0.,0.,-35.749));
#15457=CARTESIAN_POINT('',(15.8175,15.1825,-35.749));
#15458=CARTESIAN_POINT('',(15.8175,17.913,-35.749));
#15459=CARTESIAN_POINT('',(17.913,15.1825,-35.749));
#15460=CARTESIAN_POINT('Origin',(15.5,15.5,-33.844));
#15461=CARTESIAN_POINT('Origin',(0.,0.,-35.749));
#15462=CARTESIAN_POINT('',(15.8175,15.8175,-35.749));
#15463=CARTESIAN_POINT('',(15.8175,17.913,-35.749));
#15464=CARTESIAN_POINT('',(17.913,15.8175,-35.749));
#15465=CARTESIAN_POINT('Origin',(15.8175,17.913,-34.987));
#15466=CARTESIAN_POINT('',(15.8175,15.8175,-34.987));
#15467=CARTESIAN_POINT('',(15.8175,15.8175,-34.987));
#15468=CARTESIAN_POINT('',(15.8175,17.913,-34.987));
#15469=CARTESIAN_POINT('',(15.8175,17.913,-34.987));
#15470=CARTESIAN_POINT('',(15.8175,17.913,-34.987));
#15471=CARTESIAN_POINT('Origin',(15.1825,17.913,-34.987));
#15472=CARTESIAN_POINT('',(15.1825,17.913,-34.987));
#15473=CARTESIAN_POINT('',(15.1825,17.913,-34.987));
#15474=CARTESIAN_POINT('',(15.1825,15.8175,-34.987));
#15475=CARTESIAN_POINT('',(15.1825,17.913,-34.987));
#15476=CARTESIAN_POINT('',(15.1825,15.8175,-34.987));
#15477=CARTESIAN_POINT('Origin',(15.8175,17.913,-34.987));
#15478=CARTESIAN_POINT('',(15.8175,13.087,-34.987));
#15479=CARTESIAN_POINT('',(15.8175,13.087,-34.987));
#15480=CARTESIAN_POINT('',(15.8175,15.1825,-34.987));
#15481=CARTESIAN_POINT('',(15.8175,17.913,-34.987));
#15482=CARTESIAN_POINT('',(15.8175,15.1825,-34.987));
#15483=CARTESIAN_POINT('Origin',(15.8175,17.913,-34.987));
#15484=CARTESIAN_POINT('',(15.8175,17.913,-34.987));
#15485=CARTESIAN_POINT('Origin',(15.1825,17.913,-34.987));
#15486=CARTESIAN_POINT('',(15.1825,15.1825,-34.987));
#15487=CARTESIAN_POINT('',(15.1825,15.1825,-34.987));
#15488=CARTESIAN_POINT('',(15.1825,13.087,-34.987));
#15489=CARTESIAN_POINT('',(15.1825,17.913,-34.987));
#15490=CARTESIAN_POINT('',(15.1825,13.087,-34.987));
#15491=CARTESIAN_POINT('Origin',(15.1825,13.087,-34.987));
#15492=CARTESIAN_POINT('',(15.1825,13.087,-34.987));
#15493=CARTESIAN_POINT('Origin',(0.,0.,-34.987));
#15494=CARTESIAN_POINT('',(13.087,15.1825,-34.987));
#15495=CARTESIAN_POINT('',(17.913,15.1825,-34.987));
#15496=CARTESIAN_POINT('',(13.087,15.8175,-34.987));
#15497=CARTESIAN_POINT('',(13.087,15.8175,-34.987));
#15498=CARTESIAN_POINT('',(17.913,15.8175,-34.987));
#15499=CARTESIAN_POINT('',(17.913,15.8175,-34.987));
#15500=CARTESIAN_POINT('',(17.913,15.8175,-34.987));
#15501=CARTESIAN_POINT('',(17.913,15.1825,-34.987));
#15502=CARTESIAN_POINT('',(17.913,15.1825,-34.987));
#15503=CARTESIAN_POINT('',(17.913,15.1825,-34.987));
#15504=CARTESIAN_POINT('Origin',(13.087,15.8175,-34.987));
#15505=CARTESIAN_POINT('',(13.087,15.8175,-34.987));
#15506=CARTESIAN_POINT('',(13.087,15.1825,-34.987));
#15507=CARTESIAN_POINT('Origin',(17.913,15.8175,-34.987));
#15508=CARTESIAN_POINT('Origin',(17.913,15.1825,-34.987));
#15509=CARTESIAN_POINT('Origin',(17.913,15.1825,-34.987));
#15510=CARTESIAN_POINT('',(17.913,15.1825,-34.987));
#15511=CARTESIAN_POINT('Origin',(17.913,15.1825,-34.987));
#15512=CARTESIAN_POINT('',(17.913,15.8175,-34.987));
#15513=CARTESIAN_POINT('Origin',(17.913,15.8175,-34.987));
#15514=CARTESIAN_POINT('Origin',(-15.5000000000001,15.5,-45.9992561210692));
#15515=CARTESIAN_POINT('',(-15.5,12.3249999999999,-33.844));
#15516=CARTESIAN_POINT('Origin',(-15.5000000000001,15.5,-33.844));
#15517=CARTESIAN_POINT('',(-15.5000000000001,12.325,-34.479));
#15518=CARTESIAN_POINT('',(-15.5000000000001,12.325,-45.9992561210692));
#15519=CARTESIAN_POINT('',(-15.5000000000001,18.675,-34.479));
#15520=CARTESIAN_POINT('Origin',(-15.5000000000001,15.5,-34.479));
#15521=CARTESIAN_POINT('Origin',(-15.5000000000001,15.5,-34.479));
#15522=CARTESIAN_POINT('Origin',(-15.5000000000001,15.5,-34.479));
#15523=CARTESIAN_POINT('',(-15.1825000000001,17.913,-35.6336740328739));
#15524=CARTESIAN_POINT('',(-15.5000000000001,17.913,-35.6429742265188));
#15525=CARTESIAN_POINT('Ctrl Pts',(-15.5000000000001,17.913,-35.6429742265188));
#15526=CARTESIAN_POINT('Ctrl Pts',(-15.397717884839,17.913,-35.6429742265188));
#15527=CARTESIAN_POINT('Ctrl Pts',(-15.2910620631234,17.913,-35.6401598997242));
#15528=CARTESIAN_POINT('Ctrl Pts',(-15.1825,17.913,-35.6336740328742));
#15529=CARTESIAN_POINT('Origin',(-15.5000000000001,17.405,-34.479));
#15530=CARTESIAN_POINT('',(-15.8175000000001,17.913,-35.6336740328742));
#15531=CARTESIAN_POINT('Ctrl Pts',(-15.8175000000002,17.913,-35.6336740328742));
#15532=CARTESIAN_POINT('Ctrl Pts',(-15.7089379368768,17.913,-35.6401598997242));
#15533=CARTESIAN_POINT('Ctrl Pts',(-15.6022821151612,17.913,-35.6429742265188));
#15534=CARTESIAN_POINT('Ctrl Pts',(-15.5000000000001,17.913,-35.6429742265188));
#15535=CARTESIAN_POINT('',(-15.8175000000001,17.3783553311341,-35.749));
#15536=CARTESIAN_POINT('Origin',(-15.8174999999999,17.3559153980509,-34.4373099752779));
#15537=CARTESIAN_POINT('',(-17.3783553311342,15.8174999999999,-35.749));
#15538=CARTESIAN_POINT('Origin',(-15.5000000000001,15.5,-35.749));
#15539=CARTESIAN_POINT('',(-17.9130000000001,15.8174999999999,-35.6336740328739));
#15540=CARTESIAN_POINT('Origin',(-17.3559153980642,15.8175000000004,-34.4373099753428));
#15541=CARTESIAN_POINT('',(-17.913,15.1824999999999,-35.633674032875));
#15542=CARTESIAN_POINT('Ctrl Pts',(-17.9130000000001,15.8174999999999,-35.6336740328742));
#15543=CARTESIAN_POINT('Ctrl Pts',(-17.9130000000001,15.7089379368766,-35.6401598997242));
#15544=CARTESIAN_POINT('Ctrl Pts',(-17.9130000000001,15.6022821151611,-35.6429742265188));
#15545=CARTESIAN_POINT('Ctrl Pts',(-17.9130000000001,15.3977178848389,-35.6429742265188));
#15546=CARTESIAN_POINT('Ctrl Pts',(-17.9130000000001,15.2910620631233,-35.6401598997242));
#15547=CARTESIAN_POINT('Ctrl Pts',(-17.9130000000001,15.1824999999999,-35.6336740328742));
#15548=CARTESIAN_POINT('',(-17.3783553311342,15.1824999999999,-35.749));
#15549=CARTESIAN_POINT('Origin',(-17.3559153980482,15.1825000000009,-34.4373099752696));
#15550=CARTESIAN_POINT('',(-15.8175,13.6216446688658,-35.749));
#15551=CARTESIAN_POINT('Origin',(-15.5000000000001,15.5,-35.749));
#15552=CARTESIAN_POINT('',(-15.8175,13.087,-35.6336740328739));
#15553=CARTESIAN_POINT('Origin',(-15.8175000000003,13.6451071230414,-34.4325038145137));
#15554=CARTESIAN_POINT('',(-15.1825,13.087,-35.6336740328739));
#15555=CARTESIAN_POINT('Ctrl Pts',(-15.1825,13.087,-35.6336740328742));
#15556=CARTESIAN_POINT('Ctrl Pts',(-15.2910620631233,13.087,-35.6401598997242));
#15557=CARTESIAN_POINT('Ctrl Pts',(-15.397717884839,13.087,-35.6429742265188));
#15558=CARTESIAN_POINT('Ctrl Pts',(-15.6022821151612,13.087,-35.6429742265188));
#15559=CARTESIAN_POINT('Ctrl Pts',(-15.7089379368768,13.087,-35.6401598997242));
#15560=CARTESIAN_POINT('Ctrl Pts',(-15.8175,13.087,-35.6336740328742));
#15561=CARTESIAN_POINT('',(-15.1825,13.6216446688658,-35.749));
#15562=CARTESIAN_POINT('Origin',(-15.1824999999997,13.6451071230399,-34.4325038145209));
#15563=CARTESIAN_POINT('',(-13.6216446688659,15.1825,-35.749));
#15564=CARTESIAN_POINT('Origin',(-15.5000000000001,15.5,-35.749));
#15565=CARTESIAN_POINT('',(-13.0870000000001,15.1825,-35.6336740328739));
#15566=CARTESIAN_POINT('Origin',(-13.6451071230419,15.1824999999996,-34.4325038145103));
#15567=CARTESIAN_POINT('',(-13.0870000000001,15.8175,-35.633674032875));
#15568=CARTESIAN_POINT('Ctrl Pts',(-13.0870000000001,15.1825,-35.6336740328742));
#15569=CARTESIAN_POINT('Ctrl Pts',(-13.0870000000001,15.2910620631233,-35.6401598997242));
#15570=CARTESIAN_POINT('Ctrl Pts',(-13.0870000000001,15.3977178848389,-35.6429742265188));
#15571=CARTESIAN_POINT('Ctrl Pts',(-13.0870000000001,15.6022821151611,-35.6429742265188));
#15572=CARTESIAN_POINT('Ctrl Pts',(-13.0870000000001,15.7089379368767,-35.6401598997242));
#15573=CARTESIAN_POINT('Ctrl Pts',(-13.0870000000001,15.8175,-35.6336740328742));
#15574=CARTESIAN_POINT('',(-13.6216446688659,15.8175,-35.749));
#15575=CARTESIAN_POINT('Origin',(-13.6451071230542,15.8174999999991,-34.4325038144614));
#15576=CARTESIAN_POINT('',(-15.1825000000001,17.378355331134,-35.749));
#15577=CARTESIAN_POINT('Origin',(-15.5000000000001,15.5,-35.749));
#15578=CARTESIAN_POINT('Origin',(-15.1824999999996,17.3559153980558,-34.4373099753074));
#15579=CARTESIAN_POINT('Origin',(-1.48788610350143E-30,-1.48788610350144E-30,
-35.749));
#15580=CARTESIAN_POINT('',(-15.8175000000001,15.1825,-35.749));
#15581=CARTESIAN_POINT('',(-17.913,15.1824999999999,-35.749));
#15582=CARTESIAN_POINT('',(-15.8175000000001,17.913,-35.749));
#15583=CARTESIAN_POINT('Origin',(-1.48788610350143E-30,-1.48788610350144E-30,
-35.749));
#15584=CARTESIAN_POINT('',(-15.1825000000001,15.1825,-35.749));
#15585=CARTESIAN_POINT('',(-15.1825000000001,17.913,-35.749));
#15586=CARTESIAN_POINT('',(-17.913,15.1824999999999,-35.749));
#15587=CARTESIAN_POINT('Origin',(-1.48788610350143E-30,-1.48788610350144E-30,
-35.749));
#15588=CARTESIAN_POINT('',(-15.1825000000001,15.8175,-35.749));
#15589=CARTESIAN_POINT('',(-17.9130000000001,15.8174999999999,-35.749));
#15590=CARTESIAN_POINT('',(-15.1825000000001,17.913,-35.749));
#15591=CARTESIAN_POINT('Origin',(-15.5000000000001,15.5,-33.844));
#15592=CARTESIAN_POINT('Origin',(-1.48788610350143E-30,-1.48788610350144E-30,
-35.749));
#15593=CARTESIAN_POINT('',(-15.8175000000001,15.8174999999999,-35.749));
#15594=CARTESIAN_POINT('',(-17.9130000000001,15.8174999999999,-35.749));
#15595=CARTESIAN_POINT('',(-15.8175000000001,17.913,-35.749));
#15596=CARTESIAN_POINT('Origin',(-17.9130000000001,15.8174999999999,-34.987));
#15597=CARTESIAN_POINT('',(-15.8175000000001,15.8174999999999,-34.987));
#15598=CARTESIAN_POINT('',(-15.8175000000001,15.8174999999999,-34.987));
#15599=CARTESIAN_POINT('',(-17.9130000000001,15.8174999999999,-34.987));
#15600=CARTESIAN_POINT('',(-17.9130000000001,15.8174999999999,-34.987));
#15601=CARTESIAN_POINT('',(-17.9130000000001,15.8174999999999,-34.987));
#15602=CARTESIAN_POINT('Origin',(-17.913,15.1824999999999,-34.987));
#15603=CARTESIAN_POINT('',(-17.913,15.1824999999999,-34.987));
#15604=CARTESIAN_POINT('',(-17.913,15.1824999999999,-34.987));
#15605=CARTESIAN_POINT('',(-15.8175000000001,15.1825,-34.987));
#15606=CARTESIAN_POINT('',(-17.913,15.1824999999999,-34.987));
#15607=CARTESIAN_POINT('',(-15.8175000000001,15.1825,-34.987));
#15608=CARTESIAN_POINT('Origin',(-17.9130000000001,15.8174999999999,-34.987));
#15609=CARTESIAN_POINT('',(-13.0870000000001,15.8175,-34.987));
#15610=CARTESIAN_POINT('',(-13.0870000000001,15.8175,-34.987));
#15611=CARTESIAN_POINT('',(-15.1825000000001,15.8175,-34.987));
#15612=CARTESIAN_POINT('',(-17.9130000000001,15.8174999999999,-34.987));
#15613=CARTESIAN_POINT('',(-15.1825000000001,15.8175,-34.987));
#15614=CARTESIAN_POINT('Origin',(-17.9130000000001,15.8174999999999,-34.987));
#15615=CARTESIAN_POINT('',(-17.9130000000001,15.8174999999999,-34.987));
#15616=CARTESIAN_POINT('Origin',(-17.913,15.1824999999999,-34.987));
#15617=CARTESIAN_POINT('',(-15.1825000000001,15.1825,-34.987));
#15618=CARTESIAN_POINT('',(-15.1825000000001,15.1825,-34.987));
#15619=CARTESIAN_POINT('',(-13.0870000000001,15.1825,-34.987));
#15620=CARTESIAN_POINT('',(-17.913,15.1824999999999,-34.987));
#15621=CARTESIAN_POINT('',(-13.0870000000001,15.1825,-34.987));
#15622=CARTESIAN_POINT('Origin',(-13.0870000000001,15.1825,-34.987));
#15623=CARTESIAN_POINT('',(-13.0870000000001,15.1825,-34.987));
#15624=CARTESIAN_POINT('Origin',(-1.45617139229641E-30,-1.45617139229642E-30,
-34.987));
#15625=CARTESIAN_POINT('',(-15.1825,13.087,-34.987));
#15626=CARTESIAN_POINT('',(-15.1825000000001,17.913,-34.987));
#15627=CARTESIAN_POINT('',(-15.8175,13.087,-34.987));
#15628=CARTESIAN_POINT('',(-15.8175,13.087,-34.987));
#15629=CARTESIAN_POINT('',(-15.8175000000001,17.913,-34.987));
#15630=CARTESIAN_POINT('',(-15.8175000000001,17.913,-34.987));
#15631=CARTESIAN_POINT('',(-15.8175000000001,17.913,-34.987));
#15632=CARTESIAN_POINT('',(-15.1825000000001,17.913,-34.987));
#15633=CARTESIAN_POINT('',(-15.1825000000001,17.913,-34.987));
#15634=CARTESIAN_POINT('',(-15.1825000000001,17.913,-34.987));
#15635=CARTESIAN_POINT('Origin',(-15.8175,13.087,-34.987));
#15636=CARTESIAN_POINT('',(-15.8175,13.087,-34.987));
#15637=CARTESIAN_POINT('',(-15.1825,13.087,-34.987));
#15638=CARTESIAN_POINT('Origin',(-15.8175000000001,17.913,-34.987));
#15639=CARTESIAN_POINT('Origin',(-15.1825000000001,17.913,-34.987));
#15640=CARTESIAN_POINT('Origin',(-15.1825000000001,17.913,-34.987));
#15641=CARTESIAN_POINT('',(-15.1825000000001,17.913,-34.987));
#15642=CARTESIAN_POINT('Origin',(-15.1825000000001,17.913,-34.987));
#15643=CARTESIAN_POINT('',(-15.8175000000001,17.913,-34.987));
#15644=CARTESIAN_POINT('Origin',(-15.8175000000001,17.913,-34.987));
#15645=CARTESIAN_POINT('Origin',(-15.5,-15.5,-45.9992561210692));
#15646=CARTESIAN_POINT('',(-12.325,-15.5,-33.844));
#15647=CARTESIAN_POINT('Origin',(-15.5,-15.5,-33.844));
#15648=CARTESIAN_POINT('',(-12.325,-15.5,-34.479));
#15649=CARTESIAN_POINT('',(-12.325,-15.5,-45.9992561210692));
#15650=CARTESIAN_POINT('',(-18.675,-15.5,-34.479));
#15651=CARTESIAN_POINT('Origin',(-15.5,-15.5,-34.479));
#15652=CARTESIAN_POINT('Origin',(-15.5,-15.5,-34.479));
#15653=CARTESIAN_POINT('Origin',(-15.5,-15.5,-34.479));
#15654=CARTESIAN_POINT('',(-17.913,-15.1825,-35.6336740328739));
#15655=CARTESIAN_POINT('',(-17.913,-15.5,-35.6429742265188));
#15656=CARTESIAN_POINT('Ctrl Pts',(-17.913,-15.5,-35.6429742265188));
#15657=CARTESIAN_POINT('Ctrl Pts',(-17.913,-15.3977178848389,-35.6429742265188));
#15658=CARTESIAN_POINT('Ctrl Pts',(-17.913,-15.2910620631233,-35.6401598997242));
#15659=CARTESIAN_POINT('Ctrl Pts',(-17.913,-15.1824999999999,-35.6336740328742));
#15660=CARTESIAN_POINT('Origin',(-17.405,-15.5,-34.479));
#15661=CARTESIAN_POINT('',(-17.913,-15.8175,-35.6336740328742));
#15662=CARTESIAN_POINT('Ctrl Pts',(-17.913,-15.8175000000001,-35.6336740328742));
#15663=CARTESIAN_POINT('Ctrl Pts',(-17.913,-15.7089379368767,-35.6401598997242));
#15664=CARTESIAN_POINT('Ctrl Pts',(-17.913,-15.6022821151611,-35.6429742265188));
#15665=CARTESIAN_POINT('Ctrl Pts',(-17.913,-15.5,-35.6429742265188));
#15666=CARTESIAN_POINT('',(-17.3783553311341,-15.8175,-35.749));
#15667=CARTESIAN_POINT('Origin',(-17.3559153980514,-15.8175,-34.4373099752802));
#15668=CARTESIAN_POINT('',(-15.8175,-17.3783553311341,-35.749));
#15669=CARTESIAN_POINT('Origin',(-15.5,-15.5,-35.749));
#15670=CARTESIAN_POINT('',(-15.8175,-17.913,-35.6336740328739));
#15671=CARTESIAN_POINT('Origin',(-15.8175000000003,-17.3559153980479,-34.4373099752707));
#15672=CARTESIAN_POINT('',(-15.1825,-17.913,-35.633674032875));
#15673=CARTESIAN_POINT('Ctrl Pts',(-15.8175,-17.913,-35.6336740328742));
#15674=CARTESIAN_POINT('Ctrl Pts',(-15.7089379368767,-17.913,-35.6401598997242));
#15675=CARTESIAN_POINT('Ctrl Pts',(-15.6022821151611,-17.913,-35.6429742265188));
#15676=CARTESIAN_POINT('Ctrl Pts',(-15.3977178848389,-17.913,-35.6429742265188));
#15677=CARTESIAN_POINT('Ctrl Pts',(-15.2910620631233,-17.913,-35.6401598997242));
#15678=CARTESIAN_POINT('Ctrl Pts',(-15.1825,-17.913,-35.6336740328742));
#15679=CARTESIAN_POINT('',(-15.1825,-17.3783553311341,-35.749));
#15680=CARTESIAN_POINT('Origin',(-15.1825000000009,-17.3559153980454,-34.4373099752573));
#15681=CARTESIAN_POINT('',(-13.6216446688659,-15.8175,-35.749));
#15682=CARTESIAN_POINT('Origin',(-15.5,-15.5,-35.749));
#15683=CARTESIAN_POINT('',(-13.087,-15.8175,-35.6336740328739));
#15684=CARTESIAN_POINT('Origin',(-13.6451071230427,-15.8175000000003,-34.4325038145077));
#15685=CARTESIAN_POINT('',(-13.087,-15.1825,-35.6336740328739));
#15686=CARTESIAN_POINT('Ctrl Pts',(-13.087,-15.1825,-35.6336740328742));
#15687=CARTESIAN_POINT('Ctrl Pts',(-13.087,-15.2910620631233,-35.6401598997242));
#15688=CARTESIAN_POINT('Ctrl Pts',(-13.087,-15.3977178848389,-35.6429742265188));
#15689=CARTESIAN_POINT('Ctrl Pts',(-13.087,-15.6022821151611,-35.6429742265188));
#15690=CARTESIAN_POINT('Ctrl Pts',(-13.087,-15.7089379368767,-35.6401598997242));
#15691=CARTESIAN_POINT('Ctrl Pts',(-13.087,-15.8175,-35.6336740328742));
#15692=CARTESIAN_POINT('',(-13.6216446688659,-15.1825,-35.749));
#15693=CARTESIAN_POINT('Origin',(-13.6451071230429,-15.1824999999997,-34.4325038145053));
#15694=CARTESIAN_POINT('',(-15.1825,-13.6216446688659,-35.749));
#15695=CARTESIAN_POINT('Origin',(-15.5,-15.5,-35.749));
#15696=CARTESIAN_POINT('',(-15.1825,-13.087,-35.6336740328739));
#15697=CARTESIAN_POINT('Origin',(-15.1824999999996,-13.6451071230448,-34.4325038144978));
#15698=CARTESIAN_POINT('',(-15.8175,-13.087,-35.633674032875));
#15699=CARTESIAN_POINT('Ctrl Pts',(-15.1825,-13.087,-35.6336740328742));
#15700=CARTESIAN_POINT('Ctrl Pts',(-15.2910620631233,-13.087,-35.6401598997242));
#15701=CARTESIAN_POINT('Ctrl Pts',(-15.3977178848389,-13.087,-35.6429742265188));
#15702=CARTESIAN_POINT('Ctrl Pts',(-15.6022821151611,-13.087,-35.6429742265188));
#15703=CARTESIAN_POINT('Ctrl Pts',(-15.7089379368767,-13.087,-35.6401598997242));
#15704=CARTESIAN_POINT('Ctrl Pts',(-15.8175,-13.087,-35.6336740328742));
#15705=CARTESIAN_POINT('',(-15.8175,-13.6216446688659,-35.749));
#15706=CARTESIAN_POINT('Origin',(-15.8174999999991,-13.6451071230564,-34.4325038144518));
#15707=CARTESIAN_POINT('',(-17.3783553311341,-15.1825,-35.749));
#15708=CARTESIAN_POINT('Origin',(-15.5,-15.5,-35.749));
#15709=CARTESIAN_POINT('Origin',(-17.3559153980526,-15.1824999999996,-34.4373099752921));
#15710=CARTESIAN_POINT('Origin',(0.,-2.97577220700286E-30,-35.749));
#15711=CARTESIAN_POINT('',(-15.1825,-15.8175,-35.749));
#15712=CARTESIAN_POINT('',(-15.1825,-17.913,-35.749));
#15713=CARTESIAN_POINT('',(-17.913,-15.8175,-35.749));
#15714=CARTESIAN_POINT('Origin',(0.,-2.97577220700286E-30,-35.749));
#15715=CARTESIAN_POINT('',(-15.1825,-15.1825,-35.749));
#15716=CARTESIAN_POINT('',(-17.913,-15.1825,-35.749));
#15717=CARTESIAN_POINT('',(-15.1825,-17.913,-35.749));
#15718=CARTESIAN_POINT('Origin',(0.,-2.97577220700286E-30,-35.749));
#15719=CARTESIAN_POINT('',(-15.8175,-15.1825,-35.749));
#15720=CARTESIAN_POINT('',(-15.8175,-17.913,-35.749));
#15721=CARTESIAN_POINT('',(-17.913,-15.1825,-35.749));
#15722=CARTESIAN_POINT('Origin',(-15.5,-15.5,-33.844));
#15723=CARTESIAN_POINT('Origin',(0.,-2.97577220700286E-30,-35.749));
#15724=CARTESIAN_POINT('',(-15.8175,-15.8175,-35.749));
#15725=CARTESIAN_POINT('',(-15.8175,-17.913,-35.749));
#15726=CARTESIAN_POINT('',(-17.913,-15.8175,-35.749));
#15727=CARTESIAN_POINT('Origin',(-15.8175,-17.913,-34.987));
#15728=CARTESIAN_POINT('',(-15.8175,-15.8175,-34.987));
#15729=CARTESIAN_POINT('',(-15.8175,-15.8175,-34.987));
#15730=CARTESIAN_POINT('',(-15.8175,-17.913,-34.987));
#15731=CARTESIAN_POINT('',(-15.8175,-17.913,-34.987));
#15732=CARTESIAN_POINT('',(-15.8175,-17.913,-34.987));
#15733=CARTESIAN_POINT('Origin',(-15.1825,-17.913,-34.987));
#15734=CARTESIAN_POINT('',(-15.1825,-17.913,-34.987));
#15735=CARTESIAN_POINT('',(-15.1825,-17.913,-34.987));
#15736=CARTESIAN_POINT('',(-15.1825,-15.8175,-34.987));
#15737=CARTESIAN_POINT('',(-15.1825,-17.913,-34.987));
#15738=CARTESIAN_POINT('',(-15.1825,-15.8175,-34.987));
#15739=CARTESIAN_POINT('Origin',(-15.8175,-17.913,-34.987));
#15740=CARTESIAN_POINT('',(-15.8175,-13.087,-34.987));
#15741=CARTESIAN_POINT('',(-15.8175,-13.087,-34.987));
#15742=CARTESIAN_POINT('',(-15.8175,-15.1825,-34.987));
#15743=CARTESIAN_POINT('',(-15.8175,-17.913,-34.987));
#15744=CARTESIAN_POINT('',(-15.8175,-15.1825,-34.987));
#15745=CARTESIAN_POINT('Origin',(-15.8175,-17.913,-34.987));
#15746=CARTESIAN_POINT('',(-15.8175,-17.913,-34.987));
#15747=CARTESIAN_POINT('Origin',(-15.1825,-17.913,-34.987));
#15748=CARTESIAN_POINT('',(-15.1825,-15.1825,-34.987));
#15749=CARTESIAN_POINT('',(-15.1825,-15.1825,-34.987));
#15750=CARTESIAN_POINT('',(-15.1825,-13.087,-34.987));
#15751=CARTESIAN_POINT('',(-15.1825,-17.913,-34.987));
#15752=CARTESIAN_POINT('',(-15.1825,-13.087,-34.987));
#15753=CARTESIAN_POINT('Origin',(-15.1825,-13.087,-34.987));
#15754=CARTESIAN_POINT('',(-15.1825,-13.087,-34.987));
#15755=CARTESIAN_POINT('Origin',(0.,-2.91234278459283E-30,-34.987));
#15756=CARTESIAN_POINT('',(-13.087,-15.1825,-34.987));
#15757=CARTESIAN_POINT('',(-17.913,-15.1825,-34.987));
#15758=CARTESIAN_POINT('',(-13.087,-15.8175,-34.987));
#15759=CARTESIAN_POINT('',(-13.087,-15.8175,-34.987));
#15760=CARTESIAN_POINT('',(-17.913,-15.8175,-34.987));
#15761=CARTESIAN_POINT('',(-17.913,-15.8175,-34.987));
#15762=CARTESIAN_POINT('',(-17.913,-15.8175,-34.987));
#15763=CARTESIAN_POINT('',(-17.913,-15.1825,-34.987));
#15764=CARTESIAN_POINT('',(-17.913,-15.1825,-34.987));
#15765=CARTESIAN_POINT('',(-17.913,-15.1825,-34.987));
#15766=CARTESIAN_POINT('Origin',(-13.087,-15.8175,-34.987));
#15767=CARTESIAN_POINT('',(-13.087,-15.8175,-34.987));
#15768=CARTESIAN_POINT('',(-13.087,-15.1825,-34.987));
#15769=CARTESIAN_POINT('Origin',(-17.913,-15.8175,-34.987));
#15770=CARTESIAN_POINT('Origin',(-17.913,-15.1825,-34.987));
#15771=CARTESIAN_POINT('Origin',(-17.913,-15.1825,-34.987));
#15772=CARTESIAN_POINT('',(-17.913,-15.1825,-34.987));
#15773=CARTESIAN_POINT('Origin',(-17.913,-15.1825,-34.987));
#15774=CARTESIAN_POINT('',(-17.913,-15.8175,-34.987));
#15775=CARTESIAN_POINT('Origin',(-17.913,-15.8175,-34.987));
#15776=CARTESIAN_POINT('Origin',(15.5000000000002,-15.4999999999998,-45.9992561210692));
#15777=CARTESIAN_POINT('',(15.5000000000001,-12.3249999999998,-33.844));
#15778=CARTESIAN_POINT('Origin',(15.5000000000002,-15.4999999999998,-33.844));
#15779=CARTESIAN_POINT('',(15.5000000000002,-12.3249999999998,-34.479));
#15780=CARTESIAN_POINT('',(15.5000000000002,-12.3249999999998,-45.9992561210692));
#15781=CARTESIAN_POINT('',(15.5000000000002,-18.6749999999998,-34.479));
#15782=CARTESIAN_POINT('Origin',(15.5000000000002,-15.4999999999998,-34.479));
#15783=CARTESIAN_POINT('Origin',(15.5000000000002,-15.4999999999998,-34.479));
#15784=CARTESIAN_POINT('Origin',(15.5000000000002,-15.4999999999998,-34.479));
#15785=CARTESIAN_POINT('',(15.1825000000002,-17.9129999999998,-35.6336740328739));
#15786=CARTESIAN_POINT('',(15.5000000000002,-17.9129999999998,-35.6429742265188));
#15787=CARTESIAN_POINT('Ctrl Pts',(15.5000000000002,-17.9129999999998,-35.6429742265188));
#15788=CARTESIAN_POINT('Ctrl Pts',(15.3977178848391,-17.9129999999998,-35.6429742265188));
#15789=CARTESIAN_POINT('Ctrl Pts',(15.2910620631235,-17.9129999999998,-35.6401598997242));
#15790=CARTESIAN_POINT('Ctrl Pts',(15.1825000000001,-17.9129999999998,-35.6336740328742));
#15791=CARTESIAN_POINT('Origin',(15.5000000000002,-17.4049999999998,-34.479));
#15792=CARTESIAN_POINT('',(15.8175000000002,-17.9129999999998,-35.6336740328742));
#15793=CARTESIAN_POINT('Ctrl Pts',(15.8175000000002,-17.9129999999998,-35.6336740328742));
#15794=CARTESIAN_POINT('Ctrl Pts',(15.7089379368769,-17.9129999999998,-35.6401598997242));
#15795=CARTESIAN_POINT('Ctrl Pts',(15.6022821151613,-17.9129999999998,-35.6429742265188));
#15796=CARTESIAN_POINT('Ctrl Pts',(15.5000000000002,-17.9129999999998,-35.6429742265188));
#15797=CARTESIAN_POINT('',(15.8175000000002,-17.378355331134,-35.749));
#15798=CARTESIAN_POINT('Origin',(15.8175000000001,-17.3559153980596,-34.4373099753218));
#15799=CARTESIAN_POINT('',(17.3783553311343,-15.8174999999998,-35.749));
#15800=CARTESIAN_POINT('Origin',(15.5000000000002,-15.4999999999998,-35.749));
#15801=CARTESIAN_POINT('',(17.9130000000002,-15.8174999999998,-35.6336740328739));
#15802=CARTESIAN_POINT('Origin',(17.3559153980476,-15.8175000000002,-34.4373099752683));
#15803=CARTESIAN_POINT('',(17.9130000000002,-15.1824999999998,-35.633674032875));
#15804=CARTESIAN_POINT('Ctrl Pts',(17.9130000000002,-15.8174999999998,-35.6336740328742));
#15805=CARTESIAN_POINT('Ctrl Pts',(17.9130000000002,-15.7089379368765,-35.6401598997242));
#15806=CARTESIAN_POINT('Ctrl Pts',(17.9130000000002,-15.6022821151609,-35.6429742265188));
#15807=CARTESIAN_POINT('Ctrl Pts',(17.9130000000002,-15.3977178848387,-35.6429742265188));
#15808=CARTESIAN_POINT('Ctrl Pts',(17.9130000000002,-15.2910620631231,-35.6401598997242));
#15809=CARTESIAN_POINT('Ctrl Pts',(17.9130000000002,-15.1824999999999,-35.6336740328742));
#15810=CARTESIAN_POINT('',(17.3783553311343,-15.1824999999998,-35.749));
#15811=CARTESIAN_POINT('Origin',(17.3559153980464,-15.1825000000005,-34.4373099752598));
#15812=CARTESIAN_POINT('',(15.8175000000001,-13.6216446688657,-35.749));
#15813=CARTESIAN_POINT('Origin',(15.5000000000002,-15.4999999999998,-35.749));
#15814=CARTESIAN_POINT('',(15.8175000000001,-13.0869999999998,-35.6336740328739));
#15815=CARTESIAN_POINT('Origin',(15.8175000000005,-13.6451071230423,-34.4325038145089));
#15816=CARTESIAN_POINT('',(15.1825000000001,-13.0869999999998,-35.6336740328739));
#15817=CARTESIAN_POINT('Ctrl Pts',(15.1825000000001,-13.0869999999998,-35.6336740328742));
#15818=CARTESIAN_POINT('Ctrl Pts',(15.2910620631234,-13.0869999999998,-35.6401598997242));
#15819=CARTESIAN_POINT('Ctrl Pts',(15.3977178848391,-13.0869999999998,-35.6429742265188));
#15820=CARTESIAN_POINT('Ctrl Pts',(15.6022821151612,-13.0869999999998,-35.6429742265188));
#15821=CARTESIAN_POINT('Ctrl Pts',(15.7089379368768,-13.0869999999998,-35.6401598997242));
#15822=CARTESIAN_POINT('Ctrl Pts',(15.8175000000001,-13.0869999999998,-35.6336740328742));
#15823=CARTESIAN_POINT('',(15.1825000000001,-13.6216446688657,-35.749));
#15824=CARTESIAN_POINT('Origin',(15.1824999999998,-13.6451071230404,-34.4325038145186));
#15825=CARTESIAN_POINT('',(13.621644668866,-15.1824999999999,-35.749));
#15826=CARTESIAN_POINT('Origin',(15.5000000000002,-15.4999999999998,-35.749));
#15827=CARTESIAN_POINT('',(13.0870000000002,-15.1824999999999,-35.6336740328739));
#15828=CARTESIAN_POINT('Origin',(13.6451071230549,-15.1824999999995,-34.4325038144557));
#15829=CARTESIAN_POINT('',(13.0870000000002,-15.8174999999999,-35.633674032875));
#15830=CARTESIAN_POINT('Ctrl Pts',(13.0870000000002,-15.1824999999999,-35.6336740328742));
#15831=CARTESIAN_POINT('Ctrl Pts',(13.0870000000002,-15.2910620631232,-35.6401598997242));
#15832=CARTESIAN_POINT('Ctrl Pts',(13.0870000000002,-15.3977178848388,-35.6429742265188));
#15833=CARTESIAN_POINT('Ctrl Pts',(13.0870000000002,-15.6022821151609,-35.6429742265188));
#15834=CARTESIAN_POINT('Ctrl Pts',(13.0870000000002,-15.7089379368765,-35.6401598997242));
#15835=CARTESIAN_POINT('Ctrl Pts',(13.0870000000002,-15.8174999999999,-35.6336740328742));
#15836=CARTESIAN_POINT('',(13.621644668866,-15.8174999999999,-35.749));
#15837=CARTESIAN_POINT('Origin',(13.6451071230544,-15.817499999999,-34.4325038144617));
#15838=CARTESIAN_POINT('',(15.1825000000002,-17.3783553311339,-35.749));
#15839=CARTESIAN_POINT('Origin',(15.5000000000002,-15.4999999999998,-35.749));
#15840=CARTESIAN_POINT('Origin',(15.1824999999999,-17.3559153980519,-34.4373099752894));
#15841=CARTESIAN_POINT('Origin',(1.48788610350143E-30,-1.48788610350141E-30,
-35.749));
#15842=CARTESIAN_POINT('',(15.8175000000002,-15.1824999999998,-35.749));
#15843=CARTESIAN_POINT('',(17.9130000000002,-15.1824999999998,-35.749));
#15844=CARTESIAN_POINT('',(15.8175000000002,-17.9129999999998,-35.749));
#15845=CARTESIAN_POINT('Origin',(1.48788610350143E-30,-1.48788610350141E-30,
-35.749));
#15846=CARTESIAN_POINT('',(15.1825000000002,-15.1824999999998,-35.749));
#15847=CARTESIAN_POINT('',(15.1825000000002,-17.9129999999998,-35.749));
#15848=CARTESIAN_POINT('',(17.9130000000002,-15.1824999999998,-35.749));
#15849=CARTESIAN_POINT('Origin',(1.48788610350143E-30,-1.48788610350141E-30,
-35.749));
#15850=CARTESIAN_POINT('',(15.1825000000002,-15.8174999999998,-35.749));
#15851=CARTESIAN_POINT('',(17.9130000000002,-15.8174999999998,-35.749));
#15852=CARTESIAN_POINT('',(15.1825000000002,-17.9129999999998,-35.749));
#15853=CARTESIAN_POINT('Origin',(15.5000000000002,-15.4999999999998,-33.844));
#15854=CARTESIAN_POINT('Origin',(1.48788610350143E-30,-1.48788610350141E-30,
-35.749));
#15855=CARTESIAN_POINT('',(15.8175000000002,-15.8174999999998,-35.749));
#15856=CARTESIAN_POINT('',(17.9130000000002,-15.8174999999998,-35.749));
#15857=CARTESIAN_POINT('',(15.8175000000002,-17.9129999999998,-35.749));
#15858=CARTESIAN_POINT('Origin',(17.9130000000002,-15.8174999999998,-34.987));
#15859=CARTESIAN_POINT('',(15.8175000000002,-15.8174999999998,-34.987));
#15860=CARTESIAN_POINT('',(15.8175000000002,-15.8174999999998,-34.987));
#15861=CARTESIAN_POINT('',(17.9130000000002,-15.8174999999998,-34.987));
#15862=CARTESIAN_POINT('',(17.9130000000002,-15.8174999999998,-34.987));
#15863=CARTESIAN_POINT('',(17.9130000000002,-15.8174999999998,-34.987));
#15864=CARTESIAN_POINT('Origin',(17.9130000000002,-15.1824999999998,-34.987));
#15865=CARTESIAN_POINT('',(17.9130000000002,-15.1824999999998,-34.987));
#15866=CARTESIAN_POINT('',(17.9130000000002,-15.1824999999998,-34.987));
#15867=CARTESIAN_POINT('',(15.8175000000002,-15.1824999999998,-34.987));
#15868=CARTESIAN_POINT('',(17.9130000000002,-15.1824999999998,-34.987));
#15869=CARTESIAN_POINT('',(15.8175000000002,-15.1824999999998,-34.987));
#15870=CARTESIAN_POINT('Origin',(17.9130000000002,-15.8174999999998,-34.987));
#15871=CARTESIAN_POINT('',(13.0870000000002,-15.8174999999999,-34.987));
#15872=CARTESIAN_POINT('',(13.0870000000002,-15.8174999999999,-34.987));
#15873=CARTESIAN_POINT('',(15.1825000000002,-15.8174999999998,-34.987));
#15874=CARTESIAN_POINT('',(17.9130000000002,-15.8174999999998,-34.987));
#15875=CARTESIAN_POINT('',(15.1825000000002,-15.8174999999998,-34.987));
#15876=CARTESIAN_POINT('Origin',(17.9130000000002,-15.8174999999998,-34.987));
#15877=CARTESIAN_POINT('',(17.9130000000002,-15.8174999999998,-34.987));
#15878=CARTESIAN_POINT('Origin',(17.9130000000002,-15.1824999999998,-34.987));
#15879=CARTESIAN_POINT('',(15.1825000000002,-15.1824999999998,-34.987));
#15880=CARTESIAN_POINT('',(15.1825000000002,-15.1824999999998,-34.987));
#15881=CARTESIAN_POINT('',(13.0870000000002,-15.1824999999999,-34.987));
#15882=CARTESIAN_POINT('',(17.9130000000002,-15.1824999999998,-34.987));
#15883=CARTESIAN_POINT('',(13.0870000000002,-15.1824999999999,-34.987));
#15884=CARTESIAN_POINT('Origin',(13.0870000000002,-15.1824999999999,-34.987));
#15885=CARTESIAN_POINT('',(13.0870000000002,-15.1824999999999,-34.987));
#15886=CARTESIAN_POINT('Origin',(1.45617139229641E-30,-1.4561713922964E-30,
-34.987));
#15887=CARTESIAN_POINT('',(15.1825000000001,-13.0869999999998,-34.987));
#15888=CARTESIAN_POINT('',(15.1825000000002,-17.9129999999998,-34.987));
#15889=CARTESIAN_POINT('',(15.8175000000001,-13.0869999999998,-34.987));
#15890=CARTESIAN_POINT('',(15.8175000000001,-13.0869999999998,-34.987));
#15891=CARTESIAN_POINT('',(15.8175000000002,-17.9129999999998,-34.987));
#15892=CARTESIAN_POINT('',(15.8175000000002,-17.9129999999998,-34.987));
#15893=CARTESIAN_POINT('',(15.8175000000002,-17.9129999999998,-34.987));
#15894=CARTESIAN_POINT('',(15.1825000000002,-17.9129999999998,-34.987));
#15895=CARTESIAN_POINT('',(15.1825000000002,-17.9129999999998,-34.987));
#15896=CARTESIAN_POINT('',(15.1825000000002,-17.9129999999998,-34.987));
#15897=CARTESIAN_POINT('Origin',(15.8175000000001,-13.0869999999998,-34.987));
#15898=CARTESIAN_POINT('',(15.8175000000001,-13.0869999999998,-34.987));
#15899=CARTESIAN_POINT('',(15.1825000000001,-13.0869999999998,-34.987));
#15900=CARTESIAN_POINT('Origin',(15.8175000000002,-17.9129999999998,-34.987));
#15901=CARTESIAN_POINT('Origin',(15.1825000000002,-17.9129999999998,-34.987));
#15902=CARTESIAN_POINT('Origin',(15.1825000000002,-17.9129999999998,-34.987));
#15903=CARTESIAN_POINT('',(15.1825000000002,-17.9129999999998,-34.987));
#15904=CARTESIAN_POINT('Origin',(15.1825000000002,-17.9129999999998,-34.987));
#15905=CARTESIAN_POINT('',(15.8175000000002,-17.9129999999998,-34.987));
#15906=CARTESIAN_POINT('Origin',(15.8175000000002,-17.9129999999998,-34.987));
#15907=CARTESIAN_POINT('Origin',(-15.5,-15.5,-1.713));
#15908=CARTESIAN_POINT('',(-17.405,-15.5,10.4245));
#15909=CARTESIAN_POINT('',(-17.405,-15.5,10.487));
#15910=CARTESIAN_POINT('',(-17.405,-15.5,-1.713));
#15911=CARTESIAN_POINT('',(-14.1407339385556,-16.8346987578456,10.7369999999971));
#15912=CARTESIAN_POINT('Ctrl Pts',(-17.405,-15.5,10.4245));
#15913=CARTESIAN_POINT('Ctrl Pts',(-17.405,-15.2720840652369,10.4331343389953));
#15914=CARTESIAN_POINT('Ctrl Pts',(-17.3641001824124,-15.0457843881672,
10.4426020195728));
#15915=CARTESIAN_POINT('Ctrl Pts',(-17.1966348744043,-14.5985988585374,
10.4632059864524));
#15916=CARTESIAN_POINT('Ctrl Pts',(-17.0643347591089,-14.3846734577823,
10.4742040131023));
#15917=CARTESIAN_POINT('Ctrl Pts',(-16.730376764707,-14.0257798182943,10.4951047132884));
#15918=CARTESIAN_POINT('Ctrl Pts',(-16.5341453810794,-13.8820757914142,
10.5042617943533));
#15919=CARTESIAN_POINT('Ctrl Pts',(-16.0882488808044,-13.6705967759069,
10.5237673280487));
#15920=CARTESIAN_POINT('Ctrl Pts',(-15.8409345899176,-13.6088375595572,
10.534585975944));
#15921=CARTESIAN_POINT('Ctrl Pts',(-15.3427841976526,-13.5855895851824,
10.5563773316861));
#15922=CARTESIAN_POINT('Ctrl Pts',(-15.0968410526987,-13.6219267784699,
10.5671359994444));
#15923=CARTESIAN_POINT('Ctrl Pts',(-14.6347738095753,-13.785399372733,10.5873489147167));
#15924=CARTESIAN_POINT('Ctrl Pts',(-14.4226768590876,-13.9100795241097,
10.5961644815545));
#15925=CARTESIAN_POINT('Ctrl Pts',(-14.050029015234,-14.2387855609376,10.6167677930241));
#15926=CARTESIAN_POINT('Ctrl Pts',(-13.895491040028,-14.4423528711417,10.6278598074432));
#15927=CARTESIAN_POINT('Ctrl Pts',(-13.6791847013386,-14.8893109807355,
10.6495234227835));
#15928=CARTESIAN_POINT('Ctrl Pts',(-13.6161046016384,-15.1268137316682,
10.659900652251));
#15929=CARTESIAN_POINT('Ctrl Pts',(-13.5822720286564,-15.6205573481791,
10.6793455691953));
#15930=CARTESIAN_POINT('Ctrl Pts',(-13.6148906767425,-15.8722903791592,
10.6890388567062));
#15931=CARTESIAN_POINT('Ctrl Pts',(-13.7413712296963,-16.2461760980631,
10.7059695131874));
#15932=CARTESIAN_POINT('Ctrl Pts',(-13.802449717033,-16.3762850572176,10.7122344697735));
#15933=CARTESIAN_POINT('Ctrl Pts',(-13.9523779911651,-16.6199506503624,
10.7247447379606));
#15934=CARTESIAN_POINT('Ctrl Pts',(-14.040662315962,-16.7327851541203,10.7309503245344));
#15935=CARTESIAN_POINT('Ctrl Pts',(-14.1407339385535,-16.8346987578475,
10.7369999999987));
#15936=CARTESIAN_POINT('',(-13.5949999999999,-15.5,10.737));
#15937=CARTESIAN_POINT('Origin',(-15.5,-15.5,10.737));
#15938=CARTESIAN_POINT('Ctrl Pts',(-13.595,-15.5000000000012,10.7370000000001));
#15939=CARTESIAN_POINT('Ctrl Pts',(-13.5949999999998,-15.2559720572982,
10.727755275695));
#15940=CARTESIAN_POINT('Ctrl Pts',(-13.6418882041557,-15.0141454724656,
10.7175683960863));
#15941=CARTESIAN_POINT('Ctrl Pts',(-13.8269533696929,-14.5550979526125,
10.6961301022759));
#15942=CARTESIAN_POINT('Ctrl Pts',(-13.9657493860806,-14.3432783686507,
10.6850697720519));
#15943=CARTESIAN_POINT('Ctrl Pts',(-14.3151146891572,-13.9879371350501,
10.6639666580166));
#15944=CARTESIAN_POINT('Ctrl Pts',(-14.5213561808095,-13.8469618146069,
10.6548103158002));
#15945=CARTESIAN_POINT('Ctrl Pts',(-14.9736930923868,-13.6528623367304,
10.635023049327));
#15946=CARTESIAN_POINT('Ctrl Pts',(-15.2150758005425,-13.6006007016105,
10.6244638757419));
#15947=CARTESIAN_POINT('Ctrl Pts',(-15.7140940963548,-13.5900452778231,
10.6026345539653));
#15948=CARTESIAN_POINT('Ctrl Pts',(-15.9670093270509,-13.6356819789821,
10.5915708955796));
#15949=CARTESIAN_POINT('Ctrl Pts',(-16.4284043448797,-13.8190288012306,
10.5713873864882));
#15950=CARTESIAN_POINT('Ctrl Pts',(-16.6342169389518,-13.9504340066446,
10.5625623379533));
#15951=CARTESIAN_POINT('Ctrl Pts',(-16.9896936418914,-14.2870989847445,
10.5420330827009));
#15952=CARTESIAN_POINT('Ctrl Pts',(-17.1345401136243,-14.4907494677001,
10.5311498925172));
#15953=CARTESIAN_POINT('Ctrl Pts',(-17.3401653577434,-14.9463862640391,
10.5093911146263));
#15954=CARTESIAN_POINT('Ctrl Pts',(-17.3972469301894,-15.1947525769663,
10.4987335327075));
#15955=CARTESIAN_POINT('Ctrl Pts',(-17.4047548059783,-15.464697685363,10.4883427514567));
#15956=CARTESIAN_POINT('Ctrl Pts',(-17.405,-15.4823535402015,10.4876685162936));
#15957=CARTESIAN_POINT('Ctrl Pts',(-17.405,-15.5,10.487));
#15958=CARTESIAN_POINT('Origin',(-15.5,-15.5,-1.713));
#15959=CARTESIAN_POINT('',(-17.405,-15.5,9.92450000000002));
#15960=CARTESIAN_POINT('',(-17.405,-15.5,9.98699999999996));
#15961=CARTESIAN_POINT('',(-17.405,-15.5,-1.713));
#15962=CARTESIAN_POINT('Ctrl Pts',(-17.405,-15.5,9.92450000000002));
#15963=CARTESIAN_POINT('Ctrl Pts',(-17.405,-15.4858928849603,9.92503443219593));
#15964=CARTESIAN_POINT('Ctrl Pts',(-17.4048432990239,-15.4717795650996,
9.9255725268598));
#15965=CARTESIAN_POINT('Ctrl Pts',(-17.3989206140259,-15.2053500729653,
9.93579545122571));
#15966=CARTESIAN_POINT('Ctrl Pts',(-17.3432288158043,-14.9566768843941,
9.9464342612718));
#15967=CARTESIAN_POINT('Ctrl Pts',(-17.1401035489678,-14.4997826626639,
9.96818599514227));
#15968=CARTESIAN_POINT('Ctrl Pts',(-16.9962976665314,-14.2952281465799,
9.97908067355896));
#15969=CARTESIAN_POINT('Ctrl Pts',(-16.6426392387018,-13.9566550887119,
9.99964244447171));
#15970=CARTESIAN_POINT('Ctrl Pts',(-16.4376668624969,-13.8241974768803,
10.0084822019904));
#15971=CARTESIAN_POINT('Ctrl Pts',(-15.97729573678,-13.6382690782196,10.0286209214006));
#15972=CARTESIAN_POINT('Ctrl Pts',(-15.7244880114004,-13.5912198115294,
10.0396798770165));
#15973=CARTESIAN_POINT('Ctrl Pts',(-15.2251502351818,-13.5991005423923,
10.0615231743139));
#15974=CARTESIAN_POINT('Ctrl Pts',(-14.9833692139113,-13.6501161077889,
10.0720997719197));
#15975=CARTESIAN_POINT('Ctrl Pts',(-14.5302405900597,-13.8417861959255,
10.0919216714758));
#15976=CARTESIAN_POINT('Ctrl Pts',(-14.3235335496068,-13.9814347470377,
10.1010361828006));
#15977=CARTESIAN_POINT('Ctrl Pts',(-13.9719423166695,-14.3349729707548,
10.1221196779632));
#15978=CARTESIAN_POINT('Ctrl Pts',(-13.8316815321583,-14.546608011966,10.1332050547907));
#15979=CARTESIAN_POINT('Ctrl Pts',(-13.6450105327502,-15.0033955585007,
10.1545928552778));
#15980=CARTESIAN_POINT('Ctrl Pts',(-13.5969735500697,-15.2428689153515,
10.164715711879));
#15981=CARTESIAN_POINT('Ctrl Pts',(-13.5930648657893,-15.7372102120197,
10.1835287680117));
#15982=CARTESIAN_POINT('Ctrl Pts',(-13.6412030815586,-15.9874435647518,
10.1939768176186));
#15983=CARTESIAN_POINT('Ctrl Pts',(-13.8307623126648,-16.4509887967258,
10.2156837975944));
#15984=CARTESIAN_POINT('Ctrl Pts',(-13.9688638816563,-16.6603281599289,
10.2266349783049));
#15985=CARTESIAN_POINT('Ctrl Pts',(-14.3126694773338,-17.0091454193476,
10.2473693355128));
#15986=CARTESIAN_POINT('Ctrl Pts',(-14.5131893701912,-17.1472610561492,
10.2563324308918));
#15987=CARTESIAN_POINT('Ctrl Pts',(-14.9653264274279,-17.3457762984031,
10.2761109548304));
#15988=CARTESIAN_POINT('Ctrl Pts',(-15.2143646253066,-17.4003051378336,
10.2870050142302));
#15989=CARTESIAN_POINT('Ctrl Pts',(-15.7123217853693,-17.4089955584802,
10.3087879171201));
#15990=CARTESIAN_POINT('Ctrl Pts',(-15.9564269263558,-17.3657527498055,
10.3194661822552));
#15991=CARTESIAN_POINT('Ctrl Pts',(-16.4143747649841,-17.1891034921468,
10.3394988961059));
#15992=CARTESIAN_POINT('Ctrl Pts',(-16.6239526754419,-17.0575253746799,
10.3484116271306));
#15993=CARTESIAN_POINT('Ctrl Pts',(-16.9869359893406,-16.7172558558466,
10.3692416229483));
#15994=CARTESIAN_POINT('Ctrl Pts',(-17.1349074509725,-16.5098314274038,
10.3803361354248));
#15995=CARTESIAN_POINT('Ctrl Pts',(-17.3375323162512,-16.0580819096674,
10.4018820230515));
#15996=CARTESIAN_POINT('Ctrl Pts',(-17.3936448790322,-15.8195492548674,
10.4121458734487));
#15997=CARTESIAN_POINT('Ctrl Pts',(-17.4044832913812,-15.5512533747567,
10.4225470219212));
#15998=CARTESIAN_POINT('Ctrl Pts',(-17.405,-15.5256168999003,10.4235295325425));
#15999=CARTESIAN_POINT('Ctrl Pts',(-17.405,-15.5,10.4245));
#16000=CARTESIAN_POINT('Ctrl Pts',(-17.405,-15.5,10.487));
#16001=CARTESIAN_POINT('Ctrl Pts',(-17.405,-15.7233674488027,10.4785379752825));
#16002=CARTESIAN_POINT('Ctrl Pts',(-17.3657160047092,-15.9451655039957,
10.4692761752847));
#16003=CARTESIAN_POINT('Ctrl Pts',(-17.2026181913531,-16.3904274326593,
10.44884060887));
#16004=CARTESIAN_POINT('Ctrl Pts',(-17.0709111954349,-16.6063497886673,
10.4377799026799));
#16005=CARTESIAN_POINT('Ctrl Pts',(-16.7320504038859,-16.974252258311,10.4164306778067));
#16006=CARTESIAN_POINT('Ctrl Pts',(-16.5284556753648,-17.1228467103087,
10.4069893121333));
#16007=CARTESIAN_POINT('Ctrl Pts',(-16.0806603218491,-17.3306844436351,
10.3874007139918));
#16008=CARTESIAN_POINT('Ctrl Pts',(-15.8416446290644,-17.3899290558279,
10.3769450843861));
#16009=CARTESIAN_POINT('Ctrl Pts',(-15.3446905793098,-17.4155239047065,
10.3552060620872));
#16010=CARTESIAN_POINT('Ctrl Pts',(-15.0913104239464,-17.3778548751218,
10.3441220657895));
#16011=CARTESIAN_POINT('Ctrl Pts',(-14.6242327547708,-17.2091194672544,
10.3236899717749));
#16012=CARTESIAN_POINT('Ctrl Pts',(-14.4136338488466,-17.0836247288672,
10.3148992200213));
#16013=CARTESIAN_POINT('Ctrl Pts',(-14.0480376738827,-16.7576783955241,
10.2945546927935));
#16014=CARTESIAN_POINT('Ctrl Pts',(-13.8974752650319,-16.5591758882452,
10.2837415073847));
#16015=CARTESIAN_POINT('Ctrl Pts',(-13.6780183424,-16.1108202101679,10.2619560363234));
#16016=CARTESIAN_POINT('Ctrl Pts',(-13.6131998190904,-15.8643163431901,
10.2511997864289));
#16017=CARTESIAN_POINT('Ctrl Pts',(-13.5841010569675,-15.3717108225541,
10.2319015241377));
#16018=CARTESIAN_POINT('Ctrl Pts',(-13.6156809758626,-15.1305503131339,
10.2225514740956));
#16019=CARTESIAN_POINT('Ctrl Pts',(-13.7698309070763,-14.6646055022332,
10.2015280703944));
#16020=CARTESIAN_POINT('Ctrl Pts',(-13.8941011075487,-14.4452691828191,
10.1905006896061));
#16021=CARTESIAN_POINT('Ctrl Pts',(-14.2217833654884,-14.0651557923405,
10.1689333675832));
#16022=CARTESIAN_POINT('Ctrl Pts',(-14.4227033327979,-13.9087673550772,
10.1591258384604));
#16023=CARTESIAN_POINT('Ctrl Pts',(-14.865863187593,-13.6872389907069,10.1397400180406));
#16024=CARTESIAN_POINT('Ctrl Pts',(-15.1023316570555,-13.6211517131275,
10.1293958155269));
#16025=CARTESIAN_POINT('Ctrl Pts',(-15.5968004017892,-13.5807343117028,
10.1077655117328));
#16026=CARTESIAN_POINT('Ctrl Pts',(-15.8504040187405,-13.6105083795636,
10.0966717402126));
#16027=CARTESIAN_POINT('Ctrl Pts',(-16.3229596847464,-13.7646616321221,
10.0760000137906));
#16028=CARTESIAN_POINT('Ctrl Pts',(-16.5383839359081,-13.8843207578509,
10.0671630489989));
#16029=CARTESIAN_POINT('Ctrl Pts',(-16.9138012019442,-14.1997074181159,
10.0470037535998));
#16030=CARTESIAN_POINT('Ctrl Pts',(-17.0697776365901,-14.3930311503321,
10.0362683432509));
#16031=CARTESIAN_POINT('Ctrl Pts',(-17.3024997474288,-14.8338683737813,
10.0144775606673));
#16032=CARTESIAN_POINT('Ctrl Pts',(-17.3748167573771,-15.0783138076581,
10.0036352833029));
#16033=CARTESIAN_POINT('Ctrl Pts',(-17.4024647865506,-15.3864522508245,
9.99135707970488));
#16034=CARTESIAN_POINT('Ctrl Pts',(-17.405,-15.4432562982936,9.98914967135526));
#16035=CARTESIAN_POINT('Ctrl Pts',(-17.405,-15.4999999999999,9.98699999999995));
#16036=CARTESIAN_POINT('Origin',(-15.5,-15.5,-1.713));
#16037=CARTESIAN_POINT('',(-17.405,-15.4999999999999,9.42450000000002));
#16038=CARTESIAN_POINT('',(-17.405,-15.5,9.48699999999995));
#16039=CARTESIAN_POINT('',(-17.405,-15.5,-1.713));
#16040=CARTESIAN_POINT('Ctrl Pts',(-17.405,-15.4999999999999,9.42450000000001));
#16041=CARTESIAN_POINT('Ctrl Pts',(-17.405,-15.4466613264519,9.42652067569103));
#16042=CARTESIAN_POINT('Ctrl Pts',(-17.4027599096894,-15.3932664486905,
9.42859247646646));
#16043=CARTESIAN_POINT('Ctrl Pts',(-17.3770562589371,-15.088400244482,9.44070418700785));
#16044=CARTESIAN_POINT('Ctrl Pts',(-17.3060564179067,-14.8435749018795,
9.45153204731841));
#16045=CARTESIAN_POINT('Ctrl Pts',(-17.075654363384,-14.4013836246713,9.47332338181777));
#16046=CARTESIAN_POINT('Ctrl Pts',(-16.9206199127688,-14.2071364928725,
9.48407317079667));
#16047=CARTESIAN_POINT('Ctrl Pts',(-16.546929902058,-13.8898817511187,9.5042654573752));
#16048=CARTESIAN_POINT('Ctrl Pts',(-16.3323671058024,-13.7691883827222,
9.51308849055973));
#16049=CARTESIAN_POINT('Ctrl Pts',(-15.8607715005188,-13.6124415613253,
9.53371821957476));
#16050=CARTESIAN_POINT('Ctrl Pts',(-15.607190250997,-13.5812680673282,9.54481101264221));
#16051=CARTESIAN_POINT('Ctrl Pts',(-15.1122489846817,-13.6190638884743,
9.56646198667174));
#16052=CARTESIAN_POINT('Ctrl Pts',(-14.8753143328217,-13.6839438427397,
9.57682658211618));
#16053=CARTESIAN_POINT('Ctrl Pts',(-14.4313224334131,-13.9030386696172,
9.59624879993806));
#16054=CARTESIAN_POINT('Ctrl Pts',(-14.2299234575674,-14.0580267748202,
9.60598525050875));
#16055=CARTESIAN_POINT('Ctrl Pts',(-13.9002267209048,-14.4359673346765,
9.62751431850032));
#16056=CARTESIAN_POINT('Ctrl Pts',(-13.7746222022327,-14.6547120499756,
9.63854847159431));
#16057=CARTESIAN_POINT('Ctrl Pts',(-13.6177893545292,-15.1199384076246,
9.65960333896465));
#16058=CARTESIAN_POINT('Ctrl Pts',(-13.5848498401192,-15.3609429627073,
9.66900997345517));
#16059=CARTESIAN_POINT('Ctrl Pts',(-13.6111852189762,-15.8537185271427,
9.6882542362108));
#16060=CARTESIAN_POINT('Ctrl Pts',(-13.6746168216891,-16.1005756101188,
9.69899353220021));
#16061=CARTESIAN_POINT('Ctrl Pts',(-13.8916050354316,-16.5502717829196,
9.72077579013989));
#16062=CARTESIAN_POINT('Ctrl Pts',(-14.0411524564435,-16.7497115841666,
9.73160228379306));
#16063=CARTESIAN_POINT('Ctrl Pts',(-14.4049344021493,-17.0775919354096,
9.75198039781016));
#16064=CARTESIAN_POINT('Ctrl Pts',(-14.6146612252727,-17.2041533666905,
9.76077126969677));
#16065=CARTESIAN_POINT('Ctrl Pts',(-15.0807225085978,-17.3755390853041,
9.78115890238817));
#16066=CARTESIAN_POINT('Ctrl Pts',(-15.3340363632444,-17.414649518979,9.79223999839198));
#16067=CARTESIAN_POINT('Ctrl Pts',(-15.8313968608293,-17.3917694317577,
9.81399680056106));
#16068=CARTESIAN_POINT('Ctrl Pts',(-16.0708559082174,-17.333782344077,9.8244718245063));
#16069=CARTESIAN_POINT('Ctrl Pts',(-16.5194826772159,-17.1284350223924,
9.84409679252898));
#16070=CARTESIAN_POINT('Ctrl Pts',(-16.7235594195928,-16.9812365666504,
9.85348036806906));
#16071=CARTESIAN_POINT('Ctrl Pts',(-17.0644138088265,-16.6155512875477,
9.87478920166968));
#16072=CARTESIAN_POINT('Ctrl Pts',(-17.1974549309092,-16.4002718265706,
9.88585473286657));
#16073=CARTESIAN_POINT('Ctrl Pts',(-17.3644129937763,-15.9524068452289,
9.90647334540993));
#16074=CARTESIAN_POINT('Ctrl Pts',(-17.405,-15.7270401289098,9.91589883992502));
#16075=CARTESIAN_POINT('Ctrl Pts',(-17.405,-15.5,9.92450000000002));
#16076=CARTESIAN_POINT('Ctrl Pts',(-17.405,-15.4999999999999,9.98699999999996));
#16077=CARTESIAN_POINT('Ctrl Pts',(-17.405,-15.683604244378,9.98004435958553));
#16078=CARTESIAN_POINT('Ctrl Pts',(-17.3784600973982,-15.8665326447994,
9.97253383495133));
#16079=CARTESIAN_POINT('Ctrl Pts',(-17.2549772020074,-16.2816926262105,
9.95410511499368));
#16080=CARTESIAN_POINT('Ctrl Pts',(-17.1379301675275,-16.5040765573527,
9.94312026586847));
#16081=CARTESIAN_POINT('Ctrl Pts',(-16.8227314123397,-16.8939633578098,
9.92145573168694));
#16082=CARTESIAN_POINT('Ctrl Pts',(-16.6266061190295,-17.056749276571,9.91128285735042));
#16083=CARTESIAN_POINT('Ctrl Pts',(-16.1910184997219,-17.2917483583643,
9.89222828082777));
#16084=CARTESIAN_POINT('Ctrl Pts',(-15.9575035818148,-17.3650834538561,
9.88201328004444));
#16085=CARTESIAN_POINT('Ctrl Pts',(-15.4661861766118,-17.4212969458065,
9.86052083012306));
#16086=CARTESIAN_POINT('Ctrl Pts',(-15.2126060379952,-17.3999835540545,
9.84942808565165));
#16087=CARTESIAN_POINT('Ctrl Pts',(-14.7343503144704,-17.2616058287939,
9.82850701288154));
#16088=CARTESIAN_POINT('Ctrl Pts',(-14.5136523266074,-17.148207639327,9.81953350173553));
#16089=CARTESIAN_POINT('Ctrl Pts',(-14.1279075199582,-16.8440925289149,
9.79957532961759));
#16090=CARTESIAN_POINT('Ctrl Pts',(-13.9663939196341,-16.6563994788957,
9.78893212097399));
#16091=CARTESIAN_POINT('Ctrl Pts',(-13.7199253192794,-16.2239384011735,
9.76715799238112));
#16092=CARTESIAN_POINT('Ctrl Pts',(-13.6397527520202,-15.9819239268847,
9.7562359903493));
#16093=CARTESIAN_POINT('Ctrl Pts',(-13.5797699101727,-15.4915856352516,
9.73634811467448));
#16094=CARTESIAN_POINT('Ctrl Pts',(-13.5962938465972,-15.2484754744938,
9.72744297672526));
#16095=CARTESIAN_POINT('Ctrl Pts',(-13.7209832734784,-14.7749510096144,
9.70677679433944));
#16096=CARTESIAN_POINT('Ctrl Pts',(-13.8304461678666,-14.5496419268634,
9.6958470114628));
#16097=CARTESIAN_POINT('Ctrl Pts',(-14.1320990097588,-14.1503612026893,
9.67412287885901));
#16098=CARTESIAN_POINT('Ctrl Pts',(-14.3226854240572,-13.9812388909141,
9.66354731343935));
#16099=CARTESIAN_POINT('Ctrl Pts',(-14.7495292931239,-13.7324475034692,
9.64478608875415));
#16100=CARTESIAN_POINT('Ctrl Pts',(-14.9796780285392,-13.6515497085524,
9.63476124109627));
#16101=CARTESIAN_POINT('Ctrl Pts',(-15.4672143701705,-13.5788006729456,
9.61343419203103));
#16102=CARTESIAN_POINT('Ctrl Pts',(-15.7204741931685,-13.5912105377042,
9.60235545961642));
#16103=CARTESIAN_POINT('Ctrl Pts',(-16.204531811323,-13.7127816421253,9.58118058568141));
#16104=CARTESIAN_POINT('Ctrl Pts',(-16.4309078311172,-13.8195490204609,
9.57196759941106));
#16105=CARTESIAN_POINT('Ctrl Pts',(-16.827331201323,-14.1118245911351,9.55222439056537));
#16106=CARTESIAN_POINT('Ctrl Pts',(-16.9943879667994,-14.2935066477241,
9.5416876600686));
#16107=CARTESIAN_POINT('Ctrl Pts',(-17.2557532352398,-14.7183342332122,
9.51987689386206));
#16108=CARTESIAN_POINT('Ctrl Pts',(-17.3442983332949,-14.9593985818345,
9.50880776005274));
#16109=CARTESIAN_POINT('Ctrl Pts',(-17.3976475212624,-15.3066648662753,
9.49448509958961));
#16110=CARTESIAN_POINT('Ctrl Pts',(-17.405,-15.4033638686422,9.49066095121076));
#16111=CARTESIAN_POINT('Ctrl Pts',(-17.405,-15.5,9.48699999999995));
#16112=CARTESIAN_POINT('Origin',(-15.5,-15.5,-1.713));
#16113=CARTESIAN_POINT('',(-17.405,-15.5,8.92450000000001));
#16114=CARTESIAN_POINT('',(-17.405,-15.5,8.98699999999994));
#16115=CARTESIAN_POINT('',(-17.405,-15.5,-1.713));
#16116=CARTESIAN_POINT('Ctrl Pts',(-17.405,-15.5,8.92450000000001));
#16117=CARTESIAN_POINT('Ctrl Pts',(-17.405,-15.409275326029,8.92793700229262));
#16118=CARTESIAN_POINT('Ctrl Pts',(-17.398519492809,-15.3184805274955,8.93151840455227));
#16119=CARTESIAN_POINT('Ctrl Pts',(-17.3492242597744,-14.9763792634779,
8.945556724842));
#16120=CARTESIAN_POINT('Ctrl Pts',(-17.2628017286436,-14.7342827990601,
8.95661853384977));
#16121=CARTESIAN_POINT('Ctrl Pts',(-17.0050165166439,-14.306748335673,8.97845354313614));
#16122=CARTESIAN_POINT('Ctrl Pts',(-16.8394181021722,-14.1234462369798,
8.98901974966593));
#16123=CARTESIAN_POINT('Ctrl Pts',(-16.4458406175058,-13.8279968550024,
9.00882094881983));
#16124=CARTESIAN_POINT('Ctrl Pts',(-16.2210003870653,-13.7194452026138,
9.01796017554389));
#16125=CARTESIAN_POINT('Ctrl Pts',(-15.7384782505255,-13.5933449252129,
9.03906788055439));
#16126=CARTESIAN_POINT('Ctrl Pts',(-15.4851026556293,-13.5785478536479,
9.0501516773565));
#16127=CARTESIAN_POINT('Ctrl Pts',(-14.9965585940993,-13.6468643236345,
9.07152280865702));
#16128=CARTESIAN_POINT('Ctrl Pts',(-14.7654772361706,-13.7257210633924,
9.08163135449816));
#16129=CARTESIAN_POINT('Ctrl Pts',(-14.3362611084979,-13.9708249691623,
9.1004072131015));
#16130=CARTESIAN_POINT('Ctrl Pts',(-14.1441559139415,-14.1382325258434,
9.110899685755));
#16131=CARTESIAN_POINT('Ctrl Pts',(-13.838794743977,-14.5350681676457,9.13261229869945));
#16132=CARTESIAN_POINT('Ctrl Pts',(-13.7272817555302,-14.7596137954321,
9.14355799914543));
#16133=CARTESIAN_POINT('Ctrl Pts',(-13.5985427525879,-15.2321288692101,
9.16427451528865));
#16134=CARTESIAN_POINT('Ctrl Pts',(-13.5799328172441,-15.4749447987811,
9.17322125843685));
#16135=CARTESIAN_POINT('Ctrl Pts',(-13.635611148507,-15.9656408622825,9.19302853849637));
#16136=CARTESIAN_POINT('Ctrl Pts',(-13.71366210364,-16.2083400222125,9.20393007460936));
#16137=CARTESIAN_POINT('Ctrl Pts',(-13.9564334096459,-16.6431144964178,
9.2257109754222));
#16138=CARTESIAN_POINT('Ctrl Pts',(-14.1164652592955,-16.8323493150796,
9.23638018299291));
#16139=CARTESIAN_POINT('Ctrl Pts',(-14.4994156161444,-17.1395315764847,
9.25639342972927));
#16140=CARTESIAN_POINT('Ctrl Pts',(-14.7186656759076,-17.2546375642761,
9.26532089570884));
#16141=CARTESIAN_POINT('Ctrl Pts',(-15.1953865887207,-17.3973296525557,
9.28617482890278));
#16142=CARTESIAN_POINT('Ctrl Pts',(-15.4490001598685,-17.4209476505201,
9.29726903586463));
#16143=CARTESIAN_POINT('Ctrl Pts',(-15.9412261503245,-17.3690277360049,
9.31880123142265));
#16144=CARTESIAN_POINT('Ctrl Pts',(-16.175568605205,-17.2976581050846,9.32905243242355));
#16145=CARTESIAN_POINT('Ctrl Pts',(-16.61501213862,-17.0653840664801,9.348275684104));
#16146=CARTESIAN_POINT('Ctrl Pts',(-16.8137940051543,-16.9027340340602,
9.35842798312882));
#16147=CARTESIAN_POINT('Ctrl Pts',(-17.1324353710775,-16.5130185407986,
9.38016132522746));
#16148=CARTESIAN_POINT('Ctrl Pts',(-17.2507523336409,-16.2911516811955,
9.39115436188346));
#16149=CARTESIAN_POINT('Ctrl Pts',(-17.3774665425925,-15.8732814570085,
9.40975643249182));
#16150=CARTESIAN_POINT('Ctrl Pts',(-17.405,-15.6870089843509,9.41741537483886));
#16151=CARTESIAN_POINT('Ctrl Pts',(-17.405,-15.4999999999999,9.42450000000001));
#16152=CARTESIAN_POINT('Ctrl Pts',(-17.405,-15.5,9.48699999999995));
#16153=CARTESIAN_POINT('Ctrl Pts',(-17.405,-15.644525241093,9.48152482369748));
#16154=CARTESIAN_POINT('Ctrl Pts',(-17.3885555369914,-15.7888822922063,
9.47569634141479));
#16155=CARTESIAN_POINT('Ctrl Pts',(-17.2998877500828,-16.1712951301782,
9.45926969548867));
#16156=CARTESIAN_POINT('Ctrl Pts',(-17.1975903445424,-16.3991170818372,
9.44840144087596));
#16157=CARTESIAN_POINT('Ctrl Pts',(-16.9087708563741,-16.8069302128147,
9.42663476215735));
#16158=CARTESIAN_POINT('Ctrl Pts',(-16.723440169658,-16.9818639361858,9.41595399261335));
#16159=CARTESIAN_POINT('Ctrl Pts',(-16.3048257342699,-17.2434054274864,
9.39688974093776));
#16160=CARTESIAN_POINT('Ctrl Pts',(-16.077809888832,-17.331223199864,9.38727602313356));
#16161=CARTESIAN_POINT('Ctrl Pts',(-15.594132191259,-17.4190668232392,9.36611776864656));
#16162=CARTESIAN_POINT('Ctrl Pts',(-15.3414349406903,-17.4148203408526,
9.35506364569956));
#16163=CARTESIAN_POINT('Ctrl Pts',(-14.8522409502503,-17.3088796253594,
9.33366408356309));
#16164=CARTESIAN_POINT('Ctrl Pts',(-14.6205362430131,-17.2082632388532,
9.32414643406416));
#16165=CARTESIAN_POINT('Ctrl Pts',(-14.2144656677214,-16.9268481307298,
9.30460365539883));
#16166=CARTESIAN_POINT('Ctrl Pts',(-14.0425721856135,-16.7507512830307,
9.29417272431012));
#16167=CARTESIAN_POINT('Ctrl Pts',(-13.7692533807776,-16.3353303098051,
9.27245686610818));
#16168=CARTESIAN_POINT('Ctrl Pts',(-13.6735865683392,-16.0979023164427,
9.26136972349921));
#16169=CARTESIAN_POINT('Ctrl Pts',(-13.5826657913141,-15.6095993801634,
9.24088227222742));
#16170=CARTESIAN_POINT('Ctrl Pts',(-13.5843440818462,-15.3641860826945,
9.23208791148313));
#16171=CARTESIAN_POINT('Ctrl Pts',(-13.68059784426,-14.8838478203405,9.21178554845534));
#16172=CARTESIAN_POINT('Ctrl Pts',(-13.7755756290199,-14.6537037713375,
9.20098942048743));
#16173=CARTESIAN_POINT('Ctrl Pts',(-14.0511332418958,-14.2376577107011,
9.17920091374667));
#16174=CARTESIAN_POINT('Ctrl Pts',(-14.2309465084974,-14.0570001865435,
9.168423982924));
#16175=CARTESIAN_POINT('Ctrl Pts',(-14.6410908924904,-13.7826192882917,
9.1490585839653));
#16176=CARTESIAN_POINT('Ctrl Pts',(-14.8650573151847,-13.6878215260928,
9.13977527055186));
#16177=CARTESIAN_POINT('Ctrl Pts',(-15.3447514535787,-13.5850121306314,
9.11879127499656));
#16178=CARTESIAN_POINT('Ctrl Pts',(-15.596633383431,-13.5811614681987,9.10777281787266));
#16179=CARTESIAN_POINT('Ctrl Pts',(-16.0907406760179,-13.6713557098377,
9.08615832563351));
#16180=CARTESIAN_POINT('Ctrl Pts',(-16.3278520255412,-13.7657721397032,
9.07625894007863));
#16181=CARTESIAN_POINT('Ctrl Pts',(-16.7433789328809,-14.0363858974374,
9.05691852702171));
#16182=CARTESIAN_POINT('Ctrl Pts',(-16.9198464447732,-14.2068750648706,
9.04659999220047));
#16183=CARTESIAN_POINT('Ctrl Pts',(-17.2045925732363,-14.6127415422356,
9.02499615387264));
#16184=CARTESIAN_POINT('Ctrl Pts',(-17.3071205372726,-14.8464033193435,
9.01390162120042));
#16185=CARTESIAN_POINT('Ctrl Pts',(-17.3903396172592,-15.227177625558,8.99765622477507));
#16186=CARTESIAN_POINT('Ctrl Pts',(-17.405,-15.363540262961,8.99216962374751));
#16187=CARTESIAN_POINT('Ctrl Pts',(-17.405,-15.5,8.98699999999994));
#16188=CARTESIAN_POINT('Origin',(-15.5,-15.5,-1.713));
#16189=CARTESIAN_POINT('',(-17.405,-15.5,8.4245));
#16190=CARTESIAN_POINT('',(-17.405,-15.5000000000001,8.48699999999992));
#16191=CARTESIAN_POINT('',(-17.405,-15.5,-1.713));
#16192=CARTESIAN_POINT('Ctrl Pts',(-17.405,-15.5,8.4245));
#16193=CARTESIAN_POINT('Ctrl Pts',(-17.405,-15.3693362200014,8.42945005043016));
#16194=CARTESIAN_POINT('Ctrl Pts',(-17.3915584459371,-15.2387320065154,
8.43469184149533));
#16195=CARTESIAN_POINT('Ctrl Pts',(-17.3129587506065,-14.8626848265213,
8.45065711964764));
#16196=CARTESIAN_POINT('Ctrl Pts',(-17.2124302981695,-14.6278980119052,
8.46175053925174));
#16197=CARTESIAN_POINT('Ctrl Pts',(-16.9310050713234,-14.2191957001966,
8.48338917433258));
#16198=CARTESIAN_POINT('Ctrl Pts',(-16.7558615754538,-14.0470486187207,
8.49374155813311));
#16199=CARTESIAN_POINT('Ctrl Pts',(-16.3431083496375,-13.7732503683779,
8.51314194541293));
#16200=CARTESIAN_POINT('Ctrl Pts',(-16.10760158395,-13.6769965436411,8.52292075310797));
#16201=CARTESIAN_POINT('Ctrl Pts',(-15.614921506734,-13.58213919731,8.54447281247875));
#16202=CARTESIAN_POINT('Ctrl Pts',(-15.3627726883948,-13.5836059425745,
8.55550294451459));
#16203=CARTESIAN_POINT('Ctrl Pts',(-14.8818895105323,-13.6820079646112,
8.57653895404487));
#16204=CARTESIAN_POINT('Ctrl Pts',(-14.6570308346313,-13.7747367447764,
8.58591132001061));
#16205=CARTESIAN_POINT('Ctrl Pts',(-14.2443587524093,-14.0453161543274,
8.60518799033095));
#16206=CARTESIAN_POINT('Ctrl Pts',(-14.0628886413264,-14.22429314795,8.61593749508648));
#16207=CARTESIAN_POINT('Ctrl Pts',(-13.7833699390011,-14.6379403929234,
8.63772176339421));
#16208=CARTESIAN_POINT('Ctrl Pts',(-13.6862146574259,-14.8674191403123,
8.6485403139478));
#16209=CARTESIAN_POINT('Ctrl Pts',(-13.5857011635114,-15.3467664469454,
8.66889830571233));
#16210=CARTESIAN_POINT('Ctrl Pts',(-13.5817741305567,-15.5918085739254,
8.67768878488976));
#16211=CARTESIAN_POINT('Ctrl Pts',(-13.6680606652279,-16.0808563942445,
8.69810309387477));
#16212=CARTESIAN_POINT('Ctrl Pts',(-13.7616155090868,-16.3193911022531,
8.70918596958557));
#16213=CARTESIAN_POINT('Ctrl Pts',(-14.0313990140255,-16.7376546749684,
8.73093219145427));
#16214=CARTESIAN_POINT('Ctrl Pts',(-14.2018673807692,-16.9154322879258,
8.74139562594321));
#16215=CARTESIAN_POINT('Ctrl Pts',(-14.6050603235757,-17.2001034951633,
8.76099881792033));
#16216=CARTESIAN_POINT('Ctrl Pts',(-14.8351557382453,-17.3025719947771,
8.77041669896072));
#16217=CARTESIAN_POINT('Ctrl Pts',(-15.3228295720101,-17.4132202940157,
8.79174976255499));
#16218=CARTESIAN_POINT('Ctrl Pts',(-15.5757225522784,-17.4199127641496,
8.80281244760611));
#16219=CARTESIAN_POINT('Ctrl Pts',(-16.0605729834542,-17.336589793723,8.82402200277566));
#16220=CARTESIAN_POINT('Ctrl Pts',(-16.288521032735,-17.2508562853564,8.83375085279399));
#16221=CARTESIAN_POINT('Ctrl Pts',(-16.7096322391058,-16.9931544551816,
8.85272425326287));
#16222=CARTESIAN_POINT('Ctrl Pts',(-16.8965692920554,-16.8199580436126,
8.86337434157162));
#16223=CARTESIAN_POINT('Ctrl Pts',(-17.1892894534501,-16.4146779656935,
8.88513037498472));
#16224=CARTESIAN_POINT('Ctrl Pts',(-17.2937559827386,-16.1875913998802,
8.89601821398283));
#16225=CARTESIAN_POINT('Ctrl Pts',(-17.3872334019742,-15.800224289686,8.91273774450063));
#16226=CARTESIAN_POINT('Ctrl Pts',(-17.405,-15.6502231589476,8.91880896448446));
#16227=CARTESIAN_POINT('Ctrl Pts',(-17.405,-15.5,8.92450000000001));
#16228=CARTESIAN_POINT('Ctrl Pts',(-17.405,-15.5,8.98699999999994));
#16229=CARTESIAN_POINT('Ctrl Pts',(-17.405,-15.6069532063804,8.98294819799899));
#16230=CARTESIAN_POINT('Ctrl Pts',(-17.3959938933646,-15.7139509549833,
8.97869772460645));
#16231=CARTESIAN_POINT('Ctrl Pts',(-17.3366571088536,-16.0623240399535,
8.96420217194528));
#16232=CARTESIAN_POINT('Ctrl Pts',(-17.2487949895943,-16.2944938491879,
8.95348493605647));
#16233=CARTESIAN_POINT('Ctrl Pts',(-16.9862734772024,-16.7180851373411,
8.93169571590957));
#16234=CARTESIAN_POINT('Ctrl Pts',(-16.8119645569091,-16.9041043960273,
8.92083605432768));
#16235=CARTESIAN_POINT('Ctrl Pts',(-16.4101359120342,-17.1908103010399,
8.90118562039972));
#16236=CARTESIAN_POINT('Ctrl Pts',(-16.1890042445451,-17.2923371627356,
8.89214016817789));
#16237=CARTESIAN_POINT('Ctrl Pts',(-15.7132171293496,-17.4093048847077,
8.87132708352367));
#16238=CARTESIAN_POINT('Ctrl Pts',(-15.4623440480321,-17.4208031583863,
8.86035275800674));
#16239=CARTESIAN_POINT('Ctrl Pts',(-14.9667524644239,-17.3461827321486,
8.83867333615161));
#16240=CARTESIAN_POINT('Ctrl Pts',(-14.7271333943903,-17.2593674662084,
8.82841398151906));
#16241=CARTESIAN_POINT('Ctrl Pts',(-14.3042167827687,-17.0026282822229,
8.80943756151516));
#16242=CARTESIAN_POINT('Ctrl Pts',(-14.1229232827256,-16.8384414931528,
8.79925222991752));
#16243=CARTESIAN_POINT('Ctrl Pts',(-13.8259745669977,-16.443435989778,8.77779294914667));
#16244=CARTESIAN_POINT('Ctrl Pts',(-13.7160577376719,-16.214135444877,8.76670202562747));
#16245=CARTESIAN_POINT('Ctrl Pts',(-13.5931416459568,-15.7314445909808,
8.74572737175581));
#16246=CARTESIAN_POINT('Ctrl Pts',(-13.5792212868598,-15.4832891137937,
8.73671204307076));
#16247=CARTESIAN_POINT('Ctrl Pts',(-13.646465330172,-14.9964612904171,8.71679833861015));
#16248=CARTESIAN_POINT('Ctrl Pts',(-13.7265888079429,-14.7623421438691,
8.70617651589325));
#16249=CARTESIAN_POINT('Ctrl Pts',(-13.9760322448844,-14.3288654728532,
8.684298846273));
#16250=CARTESIAN_POINT('Ctrl Pts',(-14.1462917827891,-14.1356225733931,
8.67325409434886));
#16251=CARTESIAN_POINT('Ctrl Pts',(-14.5420854715896,-13.8357340475546,
8.65323624981342));
#16252=CARTESIAN_POINT('Ctrl Pts',(-14.7606109991447,-13.7278002038347,
8.64434422575922));
#16253=CARTESIAN_POINT('Ctrl Pts',(-15.2326334687793,-13.5976133907746,
8.62369582376294));
#16254=CARTESIAN_POINT('Ctrl Pts',(-15.4823561387463,-13.5789997324337,
8.61277182245205));
#16255=CARTESIAN_POINT('Ctrl Pts',(-15.9790897547409,-13.6390449845805,
8.59104244292473));
#16256=CARTESIAN_POINT('Ctrl Pts',(-16.2211008083728,-13.7187866834218,
8.58045578266087));
#16257=CARTESIAN_POINT('Ctrl Pts',(-16.6506886170301,-13.962686677952,8.56166366504681));
#16258=CARTESIAN_POINT('Ctrl Pts',(-16.8362688360923,-14.1209223401415,
8.55168424624599));
#16259=CARTESIAN_POINT('Ctrl Pts',(-17.1441810272607,-14.505661419594,8.53037410135452));
#16260=CARTESIAN_POINT('Ctrl Pts',(-17.2607621679606,-14.730739908857,8.51929736207643));
#16261=CARTESIAN_POINT('Ctrl Pts',(-17.3799675670468,-15.1439263203452,
8.50103696713371));
#16262=CARTESIAN_POINT('Ctrl Pts',(-17.405,-15.3216860808434,8.49375522239003));
#16263=CARTESIAN_POINT('Ctrl Pts',(-17.405,-15.5000000000001,8.48699999999992));
#16264=CARTESIAN_POINT('Origin',(-15.5,-15.5,-1.713));
#16265=CARTESIAN_POINT('',(-17.405,-15.5000000000001,7.92449999999999));
#16266=CARTESIAN_POINT('',(-17.405,-15.5,7.98699999999992));
#16267=CARTESIAN_POINT('',(-17.405,-15.5,-1.713));
#16268=CARTESIAN_POINT('Ctrl Pts',(-17.405,-15.5000000000001,7.92449999999999));
#16269=CARTESIAN_POINT('Ctrl Pts',(-17.405,-15.3278413248805,7.93102203788868));
#16270=CARTESIAN_POINT('Ctrl Pts',(-17.3816660200934,-15.1561469939484,
7.93803685163428));
#16271=CARTESIAN_POINT('Ctrl Pts',(-17.2680352205322,-14.7475265742745,
7.95600233998613));
#16272=CARTESIAN_POINT('Ctrl Pts',(-17.1534769956326,-14.521136506178,7.96708452120161));
#16273=CARTESIAN_POINT('Ctrl Pts',(-16.848921312095,-14.133273473672,7.98843959911533));
#16274=CARTESIAN_POINT('Ctrl Pts',(-16.6646523308701,-13.9731930129781,
7.99853444759402));
#16275=CARTESIAN_POINT('Ctrl Pts',(-16.2371009035877,-13.7253616488697,
8.01727477877572));
#16276=CARTESIAN_POINT('Ctrl Pts',(-15.9958294371788,-13.6434241389121,
8.02781017335167));
#16277=CARTESIAN_POINT('Ctrl Pts',(-15.4993610024274,-13.5788909397874,
8.04952795264963));
#16278=CARTESIAN_POINT('Ctrl Pts',(-15.2492635663799,-13.5953222638203,
8.06046834792729));
#16279=CARTESIAN_POINT('Ctrl Pts',(-14.7760729185293,-13.7214484695683,
8.08116785133282));
#16280=CARTESIAN_POINT('Ctrl Pts',(-14.5567507407337,-13.8274006779497,
8.09009978680586));
#16281=CARTESIAN_POINT('Ctrl Pts',(-14.1604663446654,-14.1221691213376,
8.10993439565284));
#16282=CARTESIAN_POINT('Ctrl Pts',(-13.989866276221,-14.3116203521669,8.12084295264752));
#16283=CARTESIAN_POINT('Ctrl Pts',(-13.7360278325154,-14.7399496784566,
8.14262174965563));
#16284=CARTESIAN_POINT('Ctrl Pts',(-13.6528638148051,-14.9733341365597,
8.15328224302487));
#16285=CARTESIAN_POINT('Ctrl Pts',(-13.5796822980195,-15.4588708210738,
8.17327690013998));
#16286=CARTESIAN_POINT('Ctrl Pts',(-13.5903664666448,-15.7064344398994,
8.18221919083499));
#16287=CARTESIAN_POINT('Ctrl Pts',(-13.7066735949874,-16.1903551164184,
8.20309588214965));
#16288=CARTESIAN_POINT('Ctrl Pts',(-13.8136966525045,-16.4214026244029,
8.21418969405491));
#16289=CARTESIAN_POINT('Ctrl Pts',(-14.1058795957532,-16.8207346051826,
8.23570864031575));
#16290=CARTESIAN_POINT('Ctrl Pts',(-14.285295796027,-16.9874232356291,8.24594769056184));
#16291=CARTESIAN_POINT('Ctrl Pts',(-14.7071162134803,-17.2507600222599,
8.2651500770754));
#16292=CARTESIAN_POINT('Ctrl Pts',(-14.9479255966595,-17.3409451581515,
8.27534976363324));
#16293=CARTESIAN_POINT('Ctrl Pts',(-15.4452236897676,-17.4204195301753,
8.29710383594769));
#16294=CARTESIAN_POINT('Ctrl Pts',(-15.6964128671484,-17.4111349486261,
8.30809198893899));
#16295=CARTESIAN_POINT('Ctrl Pts',(-16.1733455540415,-17.2982695729136,
8.32895518609092));
#16296=CARTESIAN_POINT('Ctrl Pts',(-16.3952937613701,-17.1987059718314,
8.33806187032001));
#16297=CARTESIAN_POINT('Ctrl Pts',(-16.7995631993888,-16.9155887815292,
8.35762973550196));
#16298=CARTESIAN_POINT('Ctrl Pts',(-16.9754956046028,-16.7311166563296,
8.36846629496478));
#16299=CARTESIAN_POINT('Ctrl Pts',(-17.2418429542412,-16.3096851418179,
8.39025737424484));
#16300=CARTESIAN_POINT('Ctrl Pts',(-17.3317854922963,-16.07808427619,8.40099855981789));
#16301=CARTESIAN_POINT('Ctrl Pts',(-17.395064708575,-15.7246982043178,8.4157702537691));
#16302=CARTESIAN_POINT('Ctrl Pts',(-17.405,-15.6123354215797,8.42024429882621));
#16303=CARTESIAN_POINT('Ctrl Pts',(-17.405,-15.5,8.4245));
#16304=CARTESIAN_POINT('Ctrl Pts',(-17.405,-15.5000000000001,8.48699999999993));
#16305=CARTESIAN_POINT('Ctrl Pts',(-17.405,-15.5689194556288,8.48438906389365));
#16306=CARTESIAN_POINT('Ctrl Pts',(-17.4012601389503,-15.6379154614805,
8.48169342853276));
#16307=CARTESIAN_POINT('Ctrl Pts',(-17.3672272759638,-15.9497398290679,
8.46913593704795));
#16308=CARTESIAN_POINT('Ctrl Pts',(-17.2941571210807,-16.1854094743916,
8.45860964758196));
#16309=CARTESIAN_POINT('Ctrl Pts',(-17.0583701713612,-16.6247714749451,
8.43680771718842));
#16310=CARTESIAN_POINT('Ctrl Pts',(-16.8945577340746,-16.8224418097889,
8.42573624955095));
#16311=CARTESIAN_POINT('Ctrl Pts',(-16.5082695847493,-17.1343575800066,
8.40547067406924));
#16312=CARTESIAN_POINT('Ctrl Pts',(-16.2924627289198,-17.2492106825419,
8.39666591115141));
#16313=CARTESIAN_POINT('Ctrl Pts',(-15.8245395354151,-17.3933751001279,
8.37619683007072));
#16314=CARTESIAN_POINT('Ctrl Pts',(-15.5762512021136,-17.4194718333346,
8.3653355731459));
#16315=CARTESIAN_POINT('Ctrl Pts',(-15.0785906620799,-17.3748649011662,
8.34356564576035));
#16316=CARTESIAN_POINT('Ctrl Pts',(-14.8341899508767,-17.302616329701,8.33287445104456));
#16317=CARTESIAN_POINT('Ctrl Pts',(-14.3976635436967,-17.0722738647,8.31377880768586));
#16318=CARTESIAN_POINT('Ctrl Pts',(-14.2076380393395,-16.9202201791062,
8.30420322719795));
#16319=CARTESIAN_POINT('Ctrl Pts',(-13.8885764919547,-16.5463990738807,
8.283062835803));
#16320=CARTESIAN_POINT('Ctrl Pts',(-13.7652102985012,-16.3259192551278,
8.27201190750953));
#16321=CARTESIAN_POINT('Ctrl Pts',(-13.6106874984648,-15.849658596069,8.25058954401056));
#16322=CARTESIAN_POINT('Ctrl Pts',(-13.5811365169908,-15.5985255332951,
8.24103575486708));
#16323=CARTESIAN_POINT('Ctrl Pts',(-13.6203436374559,-15.1058544769991,
8.22151391712892));
#16324=CARTESIAN_POINT('Ctrl Pts',(-13.6861534992362,-14.8688107237936,
8.21109437019214));
#16325=CARTESIAN_POINT('Ctrl Pts',(-13.9077988343148,-14.4238428734001,
8.18938937763538));
#16326=CARTESIAN_POINT('Ctrl Pts',(-14.0648875575496,-14.2218437822689,
8.17830098279379));
#16327=CARTESIAN_POINT('Ctrl Pts',(-14.4412856912249,-13.8976998272933,
8.15778847333054));
#16328=CARTESIAN_POINT('Ctrl Pts',(-14.6543836160393,-13.7757102786005,
8.14899109291169));
#16329=CARTESIAN_POINT('Ctrl Pts',(-15.1180563845774,-13.6174618962045,
8.12870794468166));
#16330=CARTESIAN_POINT('Ctrl Pts',(-15.3646752632665,-13.5838824110931,
8.11791971726744));
#16331=CARTESIAN_POINT('Ctrl Pts',(-15.8627838435254,-13.6129089088121,
8.09613019057195));
#16332=CARTESIAN_POINT('Ctrl Pts',(-16.1093548999957,-13.6775199454088,
8.08534405511831));
#16333=CARTESIAN_POINT('Ctrl Pts',(-16.5527418706616,-13.8941183052364,
8.06594829962111));
#16334=CARTESIAN_POINT('Ctrl Pts',(-16.7472855708635,-14.0400614101336,
8.05669383732974));
#16335=CARTESIAN_POINT('Ctrl Pts',(-17.0772690199196,-14.4029753150022,
8.03572776622165));
#16336=CARTESIAN_POINT('Ctrl Pts',(-17.207202564757,-14.6186949936846,8.02471352762786));
#16337=CARTESIAN_POINT('Ctrl Pts',(-17.3668134813419,-15.0609521367506,
8.00446806047157));
#16338=CARTESIAN_POINT('Ctrl Pts',(-17.405,-15.2797715610955,7.99534310685587));
#16339=CARTESIAN_POINT('Ctrl Pts',(-17.405,-15.5,7.98699999999992));
#16340=CARTESIAN_POINT('Origin',(-15.5,-15.5,-1.713));
#16341=CARTESIAN_POINT('',(-17.405,-15.5,7.42449999999999));
#16342=CARTESIAN_POINT('',(-17.405,-15.5,7.48699999999992));
#16343=CARTESIAN_POINT('',(-17.405,-15.5,-1.713));
#16344=CARTESIAN_POINT('Ctrl Pts',(-17.405,-15.5000000000001,7.42449999999999));
#16345=CARTESIAN_POINT('Ctrl Pts',(-17.405,-15.2859601869197,7.43260865772304));
#16346=CARTESIAN_POINT('Ctrl Pts',(-17.3689300191348,-15.0731745590006,
7.44145873426585));
#16347=CARTESIAN_POINT('Ctrl Pts',(-17.2155449818739,-14.6349786335938,
7.46141417266776));
#16348=CARTESIAN_POINT('Ctrl Pts',(-17.0875354560809,-14.4178315681802,
7.4724404035471));
#16349=CARTESIAN_POINT('Ctrl Pts',(-16.7607672669738,-14.0516852550486,
7.49345860578802));
#16350=CARTESIAN_POINT('Ctrl Pts',(-16.5675714828386,-13.9039370875409,
7.50279958517755));
#16351=CARTESIAN_POINT('Ctrl Pts',(-16.1262099173826,-13.6832438287778,
7.52210674027187));
#16352=CARTESIAN_POINT('Ctrl Pts',(-15.8802588412845,-13.6163539874434,
7.53286575497432));
#16353=CARTESIAN_POINT('Ctrl Pts',(-15.3822323784215,-13.5826948657237,
7.55465168948277));
#16354=CARTESIAN_POINT('Ctrl Pts',(-15.1350938622725,-13.6140566743586,
7.56546264819445));
#16355=CARTESIAN_POINT('Ctrl Pts',(-14.6701450480656,-13.7681179537064,
7.58580161644495));
#16356=CARTESIAN_POINT('Ctrl Pts',(-14.4562443785121,-13.8879677841051,
7.59459260542679));
#16357=CARTESIAN_POINT('Ctrl Pts',(-14.076872315963,-14.2084654789811,7.61503202698809));
#16358=CARTESIAN_POINT('Ctrl Pts',(-13.917761136657,-14.4091925780489,7.62611646953724));
#16359=CARTESIAN_POINT('Ctrl Pts',(-13.6918725906919,-14.8525296745866,
7.64785249145431));
#16360=CARTESIAN_POINT('Ctrl Pts',(-13.6238888493654,-15.089185426922,7.65830488708587));
#16361=CARTESIAN_POINT('Ctrl Pts',(-13.5804095704248,-15.5809930040761,
7.67788745467378));
#16362=CARTESIAN_POINT('Ctrl Pts',(-13.6075392032479,-15.8316550604089,
7.68733863994873));
#16363=CARTESIAN_POINT('Ctrl Pts',(-13.7572048353041,-16.3089652109285,
7.70869452498207));
#16364=CARTESIAN_POINT('Ctrl Pts',(-13.8785477285808,-16.5308492590566,
7.71975439676735));
#16365=CARTESIAN_POINT('Ctrl Pts',(-14.1942719736145,-16.9079615850459,
7.74094647799673));
#16366=CARTESIAN_POINT('Ctrl Pts',(-14.3829499933764,-17.0618712024457,
7.75063517031373));
#16367=CARTESIAN_POINT('Ctrl Pts',(-14.8173920364941,-17.2963209333944,
7.76963963414216));
#16368=CARTESIAN_POINT('Ctrl Pts',(-15.0610947982815,-17.3708446298938,
7.78030029738747));
#16369=CARTESIAN_POINT('Ctrl Pts',(-15.5585256515928,-17.4201228531586,
7.80206017723487));
#16370=CARTESIAN_POINT('Ctrl Pts',(-15.8072711156938,-17.39628309016,7.81294143113256));
#16371=CARTESIAN_POINT('Ctrl Pts',(-16.2764462266497,-17.2563443110142,
7.83346527675619));
#16372=CARTESIAN_POINT('Ctrl Pts',(-16.493071388795,-17.1435995165235,7.84228813470852));
#16373=CARTESIAN_POINT('Ctrl Pts',(-16.8822650416203,-16.8353316053453,
7.86247906509631));
#16374=CARTESIAN_POINT('Ctrl Pts',(-17.0480504967237,-16.6389867478324,
7.87354347288548));
#16375=CARTESIAN_POINT('Ctrl Pts',(-17.2880064817722,-16.2013715692635,
7.89537041314125));
#16376=CARTESIAN_POINT('Ctrl Pts',(-17.3632254230871,-15.9661516439027,
7.90592666430032));
#16377=CARTESIAN_POINT('Ctrl Pts',(-17.4006389639305,-15.6489266856316,
7.9187626941778));
#16378=CARTESIAN_POINT('Ctrl Pts',(-17.405,-15.574423595628,7.92168054573687));
#16379=CARTESIAN_POINT('Ctrl Pts',(-17.405,-15.5000000000001,7.92449999999999));
#16380=CARTESIAN_POINT('Ctrl Pts',(-17.405,-15.5,7.98699999999992));
#16381=CARTESIAN_POINT('Ctrl Pts',(-17.405,-15.532209736732,7.98577977032979));
#16382=CARTESIAN_POINT('Ctrl Pts',(-17.4041831077522,-15.5644482771286,
7.9845405821808));
#16383=CARTESIAN_POINT('Ctrl Pts',(-17.3902066369061,-15.839474090864,7.97381584128779));
#16384=CARTESIAN_POINT('Ctrl Pts',(-17.3315088500334,-16.0776482928075,
7.96350902576525));
#16385=CARTESIAN_POINT('Ctrl Pts',(-17.1237985933374,-16.5276682568169,
7.94191743130374));
#16386=CARTESIAN_POINT('Ctrl Pts',(-16.9733813555449,-16.7336858868427,
7.93082271913725));
#16387=CARTESIAN_POINT('Ctrl Pts',(-16.6067956491012,-17.0696781001648,
7.91007597174301));
#16388=CARTESIAN_POINT('Ctrl Pts',(-16.3962887405343,-17.1986907762383,
7.901207731432));
#16389=CARTESIAN_POINT('Ctrl Pts',(-15.9368085129371,-17.3704762421015,
7.88110798394306));
#16390=CARTESIAN_POINT('Ctrl Pts',(-15.6920027968328,-17.411178820638,7.87039907247744));
#16391=CARTESIAN_POINT('Ctrl Pts',(-15.1939245631539,-17.3971187727929,
7.8486108732789));
#16392=CARTESIAN_POINT('Ctrl Pts',(-14.9454974477225,-17.3399153220138,
7.83774354539477));
#16393=CARTESIAN_POINT('Ctrl Pts',(-14.4956487774217,-17.1366061828828,
7.81806512587155));
#16394=CARTESIAN_POINT('Ctrl Pts',(-14.2967173925019,-16.9964370779171,
7.80903898604087));
#16395=CARTESIAN_POINT('Ctrl Pts',(-13.9565177536094,-16.6439111116339,
7.78824299908806));
#16396=CARTESIAN_POINT('Ctrl Pts',(-13.8205296831303,-16.4328694086849,
7.77727355415141));
#16397=CARTESIAN_POINT('Ctrl Pts',(-13.635959276609,-15.9670032617552,7.7555877658196));
#16398=CARTESIAN_POINT('Ctrl Pts',(-13.5905662864574,-15.7162261608564,
7.74528846041283));
#16399=CARTESIAN_POINT('Ctrl Pts',(-13.599927086301,-15.2216539588205,7.72634740656811));
#16400=CARTESIAN_POINT('Ctrl Pts',(-13.6507049183005,-14.9824695442845,
7.71617554763647));
#16401=CARTESIAN_POINT('Ctrl Pts',(-13.8428022508102,-14.5273301187568,
7.69473149816027));
#16402=CARTESIAN_POINT('Ctrl Pts',(-13.9856920186994,-14.317093015566,7.68364157881967));
#16403=CARTESIAN_POINT('Ctrl Pts',(-14.3411746028942,-13.9680431210495,
7.66264300629398));
#16404=CARTESIAN_POINT('Ctrl Pts',(-14.5488518054332,-13.8311442236975,
7.65360753257075));
#16405=CARTESIAN_POINT('Ctrl Pts',(-15.0036218345933,-13.6445446066163,
7.63371383050773));
#16406=CARTESIAN_POINT('Ctrl Pts',(-15.2462142286056,-13.5961399934897,
7.62310173978103));
#16407=CARTESIAN_POINT('Ctrl Pts',(-15.7461742493181,-13.5938550022295,
7.60123122268949));
#16408=CARTESIAN_POINT('Ctrl Pts',(-15.9987330092648,-13.6438552027474,
7.59018315794992));
#16409=CARTESIAN_POINT('Ctrl Pts',(-16.4569491101971,-13.8351696420944,
7.57013870909023));
#16410=CARTESIAN_POINT('Ctrl Pts',(-16.66017366989,-13.9698316825174,7.56125974628438));
#16411=CARTESIAN_POINT('Ctrl Pts',(-17.0100084290185,-14.3123994329133,
7.54063027323432));
#16412=CARTESIAN_POINT('Ctrl Pts',(-17.1516134171614,-14.5188338184068,
7.52971251662349));
#16413=CARTESIAN_POINT('Ctrl Pts',(-17.3494687636066,-14.9783214237974,
7.50797780042861));
#16414=CARTESIAN_POINT('Ctrl Pts',(-17.4022393975719,-15.227612456327,7.49737947654021));
#16415=CARTESIAN_POINT('Ctrl Pts',(-17.4049648675835,-15.4866391454631,
7.48750692938117));
#16416=CARTESIAN_POINT('Ctrl Pts',(-17.405,-15.4933203150895,7.48725305235433));
#16417=CARTESIAN_POINT('Ctrl Pts',(-17.405,-15.5,7.48699999999992));
#16418=CARTESIAN_POINT('Origin',(-15.5,-15.5,-1.713));
#16419=CARTESIAN_POINT('',(-17.405,-15.5000000009028,6.92449999993158));
#16420=CARTESIAN_POINT('',(-17.405,-15.5,6.98699999999991));
#16421=CARTESIAN_POINT('',(-17.405,-15.5,-1.713));
#16422=CARTESIAN_POINT('Ctrl Pts',(-17.405,-15.5000000018056,6.92449999993158));
#16423=CARTESIAN_POINT('Ctrl Pts',(-17.4050000000007,-15.4993165450942,
6.92452589192082));
#16424=CARTESIAN_POINT('Ctrl Pts',(-17.4049996321956,-15.4986330720564,
6.92455179257323));
#16425=CARTESIAN_POINT('Ctrl Pts',(-17.4047272898079,-15.245605544446,6.93414341278151));
#16426=CARTESIAN_POINT('Ctrl Pts',(-17.3543192201274,-14.9958416071321,
6.9447079775017));
#16427=CARTESIAN_POINT('Ctrl Pts',(-17.1607411027068,-14.5343054481261,
6.96642674815675));
#16428=CARTESIAN_POINT('Ctrl Pts',(-17.0209296753586,-14.326370698519,6.97736211513677));
#16429=CARTESIAN_POINT('Ctrl Pts',(-16.6741899445924,-13.980587243007,6.99804571627696));
#16430=CARTESIAN_POINT('Ctrl Pts',(-16.4723615303824,-13.8441490441949,
7.00696449998315));
#16431=CARTESIAN_POINT('Ctrl Pts',(-16.0183602662677,-13.6495751788062,
7.02682457277907));
#16432=CARTESIAN_POINT('Ctrl Pts',(-15.7688428179189,-13.5972454552154,
7.03773959676634));
#16433=CARTESIAN_POINT('Ctrl Pts',(-15.2710283860677,-13.5929566539516,
7.05951625607742));
#16434=CARTESIAN_POINT('Ctrl Pts',(-15.0275172627361,-13.638275717184,7.07016853618816));
#16435=CARTESIAN_POINT('Ctrl Pts',(-14.5708371583004,-13.8189161112692,
7.09014579360003));
#16436=CARTESIAN_POINT('Ctrl Pts',(-14.3620213984788,-13.9526166083722,
7.09910262354388));
#16437=CARTESIAN_POINT('Ctrl Pts',(-14.0020253277836,-14.296403346199,7.12000052747168));
#16438=CARTESIAN_POINT('Ctrl Pts',(-13.8560796735194,-14.5049667163631,
7.1310938784775));
#16439=CARTESIAN_POINT('Ctrl Pts',(-13.6576577760441,-14.9581002563818,
7.15260026980298));
#16440=CARTESIAN_POINT('Ctrl Pts',(-13.603677776513,-15.1969076419803,7.16282788407705));
#16441=CARTESIAN_POINT('Ctrl Pts',(-13.587861043887,-15.6941342999381,7.18201070487947));
#16442=CARTESIAN_POINT('Ctrl Pts',(-13.6309452992921,-15.9479281211301,
7.19225545851312));
#16443=CARTESIAN_POINT('Ctrl Pts',(-13.8123031142063,-16.4179614599662,
7.21402884956801));
#16444=CARTESIAN_POINT('Ctrl Pts',(-13.9465467660043,-16.6303806971777,
7.22501232645237));
#16445=CARTESIAN_POINT('Ctrl Pts',(-14.2837864249233,-16.9859346325971,
7.24585828314302));
#16446=CARTESIAN_POINT('Ctrl Pts',(-14.4814296775109,-17.1277830688267,
7.25494311800115));
#16447=CARTESIAN_POINT('Ctrl Pts',(-14.9294025575922,-17.3349866726149,
7.27453948195923));
#16448=CARTESIAN_POINT('Ctrl Pts',(-15.1773104399173,-17.3943623235028,
7.28538409623418));
#16449=CARTESIAN_POINT('Ctrl Pts',(-15.675444267082,-17.4127966111112,7.30717472734376));
#16450=CARTESIAN_POINT('Ctrl Pts',(-15.9208011461287,-17.3741693632993,
7.31790774917433));
#16451=CARTESIAN_POINT('Ctrl Pts',(-16.3815184534768,-17.2063427592322,
7.33806161213794));
#16452=CARTESIAN_POINT('Ctrl Pts',(-16.5927821005162,-17.0794014782496,
7.346901104432));
#16453=CARTESIAN_POINT('Ctrl Pts',(-16.962269571994,-16.7468831279773,7.36757971660608));
#16454=CARTESIAN_POINT('Ctrl Pts',(-17.1146586683044,-16.5420253559275,
7.37867361787087));
#16455=CARTESIAN_POINT('Ctrl Pts',(-17.3264778968817,-16.093447168092,7.40030046478855));
#16456=CARTESIAN_POINT('Ctrl Pts',(-17.3872685002348,-15.8555835898382,
7.41064128732047));
#16457=CARTESIAN_POINT('Ctrl Pts',(-17.4038899094754,-15.5751324644401,
7.42162941084344));
#16458=CARTESIAN_POINT('Ctrl Pts',(-17.405,-15.5375478446883,7.42307754211034));
#16459=CARTESIAN_POINT('Ctrl Pts',(-17.405,-15.5000000000001,7.42449999999999));
#16460=CARTESIAN_POINT('Ctrl Pts',(-17.405,-15.5,7.48699999999992));
#16461=CARTESIAN_POINT('Ctrl Pts',(-17.405,-15.7347872455801,7.47810534911817));
#16462=CARTESIAN_POINT('Ctrl Pts',(-17.3615945711204,-15.9676689740826,
7.4683335115242));
#16463=CARTESIAN_POINT('Ctrl Pts',(-17.186386324715,-16.4209223251271,7.44733031644295));
#16464=CARTESIAN_POINT('Ctrl Pts',(-17.0505427522955,-16.6348205435384,
7.43625581612895));
#16465=CARTESIAN_POINT('Ctrl Pts',(-16.7055108783205,-16.9958209729757,
7.4150330917345));
#16466=CARTESIAN_POINT('Ctrl Pts',(-16.5004180729049,-17.1400882671737,
7.40576282033707));
#16467=CARTESIAN_POINT('Ctrl Pts',(-16.0500445276086,-17.3401676914711,
7.38606144040285));
#16468=CARTESIAN_POINT('Ctrl Pts',(-15.8096683757708,-17.395482444622,7.37554629815274));
#16469=CARTESIAN_POINT('Ctrl Pts',(-15.3114950305751,-17.412602840006,7.35375393834541));
#16470=CARTESIAN_POINT('Ctrl Pts',(-15.0583476117071,-17.3704389219874,
7.34268012299687));
#16471=CARTESIAN_POINT('Ctrl Pts',(-14.5944564284417,-17.193449456036,7.32238742031684));
#16472=CARTESIAN_POINT('Ctrl Pts',(-14.3865677951402,-17.0646250499273,
7.31358744261619));
#16473=CARTESIAN_POINT('Ctrl Pts',(-14.0266526607683,-16.7326405909047,
7.29313842501508));
#16474=CARTESIAN_POINT('Ctrl Pts',(-13.8792830440329,-16.5312238716456,
7.28228467155956));
#16475=CARTESIAN_POINT('Ctrl Pts',(-13.6675732369669,-16.0787216942403,
7.26051156200427));
#16476=CARTESIAN_POINT('Ctrl Pts',(-13.607098221749,-15.8311399539857,7.24980948045646));
#16477=CARTESIAN_POINT('Ctrl Pts',(-13.58664223745,-15.3380197430459,7.23068075683691));
#16478=CARTESIAN_POINT('Ctrl Pts',(-13.6224829650516,-15.0973368538402,
7.22114444460773));
#16479=CARTESIAN_POINT('Ctrl Pts',(-13.7850502774532,-14.6336626550652,
7.20002295329454));
#16480=CARTESIAN_POINT('Ctrl Pts',(-13.9134974868911,-14.4162086949334,
7.18897552292067));
#16481=CARTESIAN_POINT('Ctrl Pts',(-14.2474727228465,-14.0429233005055,
7.16752923016414));
#16482=CARTESIAN_POINT('Ctrl Pts',(-14.4498931260941,-13.8909154772963,
7.15793643367915));
#16483=CARTESIAN_POINT('Ctrl Pts',(-14.8956570181038,-13.6770378253324,
7.13843670087031));
#16484=CARTESIAN_POINT('Ctrl Pts',(-15.1335716879282,-13.6147594565805,
7.12802923499873));
#16485=CARTESIAN_POINT('Ctrl Pts',(-15.6294813482876,-13.5826035126581,
7.10633589902499));
#16486=CARTESIAN_POINT('Ctrl Pts',(-15.8829894175019,-13.6167831150686,
7.09524630719585));
#16487=CARTESIAN_POINT('Ctrl Pts',(-16.3525063151051,-13.7790877500325,
7.07470751027532));
#16488=CARTESIAN_POINT('Ctrl Pts',(-16.5652284844368,-13.9020030374803,
7.065906024606));
#16489=CARTESIAN_POINT('Ctrl Pts',(-16.9351884517455,-14.2232753518093,
7.04564312130783));
#16490=CARTESIAN_POINT('Ctrl Pts',(-17.0881738164499,-14.4194981933583,
7.03486330293791));
#16491=CARTESIAN_POINT('Ctrl Pts',(-17.3135468307644,-14.8645672137614,
7.01307294487737));
#16492=CARTESIAN_POINT('Ctrl Pts',(-17.3816998785812,-15.1101868669613,
7.00227725882102));
#16493=CARTESIAN_POINT('Ctrl Pts',(-17.403334109118,-15.4079593231243,6.99052329439176));
#16494=CARTESIAN_POINT('Ctrl Pts',(-17.405,-15.4540028611883,6.98874254989983));
#16495=CARTESIAN_POINT('Ctrl Pts',(-17.405,-15.4999999999999,6.98699999999991));
#16496=CARTESIAN_POINT('Origin',(-15.5,-15.5,-1.713));
#16497=CARTESIAN_POINT('',(-17.405,-15.5,6.42449999999997));
#16498=CARTESIAN_POINT('',(-17.405,-15.5,6.48699999999991));
#16499=CARTESIAN_POINT('',(-17.405,-15.5,-1.713));
#16500=CARTESIAN_POINT('Ctrl Pts',(-17.405,-15.4999999999999,6.42449999999997));
#16501=CARTESIAN_POINT('Ctrl Pts',(-17.405,-15.4601322430178,6.42601034515914));
#16502=CARTESIAN_POINT('Ctrl Pts',(-17.4037484985812,-15.420226760854,6.42754949266624));
#16503=CARTESIAN_POINT('Ctrl Pts',(-17.3853827382776,-15.1284149916749,
6.4390061543191));
#16504=CARTESIAN_POINT('Ctrl Pts',(-17.3196132846632,-14.8821582325296,
6.44977384181169));
#16505=CARTESIAN_POINT('Ctrl Pts',(-17.0984664394437,-14.4347306341274,
6.47156111605405));
#16506=CARTESIAN_POINT('Ctrl Pts',(-16.9472105586335,-14.2368744594976,
6.48236498368003));
#16507=CARTESIAN_POINT('Ctrl Pts',(-16.5803702499558,-13.912257525636,6.5026863601263));
#16508=CARTESIAN_POINT('Ctrl Pts',(-16.3691697008814,-13.7874961889225,
6.51147857826408));
#16509=CARTESIAN_POINT('Ctrl Pts',(-15.9013957690298,-13.6205861373532,
6.53194112996362));
#16510=CARTESIAN_POINT('Ctrl Pts',(-15.6479745696036,-13.5839087567736,
6.54302692171455));
#16511=CARTESIAN_POINT('Ctrl Pts',(-15.1513086183574,-13.6113697582875,
6.56475334127912));
#16512=CARTESIAN_POINT('Ctrl Pts',(-14.912601829198,-13.671478039929,6.57519545804024));
#16513=CARTESIAN_POINT('Ctrl Pts',(-14.4653810695128,-13.8810306020189,
6.5947589208436));
#16514=CARTESIAN_POINT('Ctrl Pts',(-14.2621189473946,-14.0305901642359,
6.60424165704099));
#16515=CARTESIAN_POINT('Ctrl Pts',(-13.924637934564,-14.4000201554789,6.62561857146581));
#16516=CARTESIAN_POINT('Ctrl Pts',(-13.79385298758,-14.6163813593607,6.63667573561485));
#16517=CARTESIAN_POINT('Ctrl Pts',(-13.6265497449183,-15.0787563566687,
6.65785159366709));
#16518=CARTESIAN_POINT('Ctrl Pts',(-13.5883173202284,-15.3191853793069,
6.66750387599365));
#16519=CARTESIAN_POINT('Ctrl Pts',(-13.6039452571242,-15.8125714288761,
6.68653707027394));
#16520=CARTESIAN_POINT('Ctrl Pts',(-13.6619870155715,-16.0607208315224,
6.6972074362341));
#16521=CARTESIAN_POINT('Ctrl Pts',(-13.8693367441029,-16.5154799558981,
6.71897068289104));
#16522=CARTESIAN_POINT('Ctrl Pts',(-14.0148996961614,-16.7185021911561,
6.72984574366513));
#16523=CARTESIAN_POINT('Ctrl Pts',(-14.3716324066437,-17.0538459441022,
6.75035241751871));
#16524=CARTESIAN_POINT('Ctrl Pts',(-14.5780288600434,-17.1845225613327,
6.75916880402621));
#16525=CARTESIAN_POINT('Ctrl Pts',(-15.0401307441502,-17.3660783945052,
6.77938323465207));
#16526=CARTESIAN_POINT('Ctrl Pts',(-15.2931160658331,-17.4107358839109,
6.79044995913515));
#16527=CARTESIAN_POINT('Ctrl Pts',(-15.7919046780419,-17.3983278051984,
6.81226923350999));
#16528=CARTESIAN_POINT('Ctrl Pts',(-16.0330075000311,-17.3452038021689,
6.82281616360576));
#16529=CARTESIAN_POINT('Ctrl Pts',(-16.4847932651915,-17.1494192766576,
6.84257932043693));
#16530=CARTESIAN_POINT('Ctrl Pts',(-16.690711503981,-17.0075201088409,6.85176618727098));
#16531=CARTESIAN_POINT('Ctrl Pts',(-17.0391100613201,-16.650333546496,6.87291806459168));
#16532=CARTESIAN_POINT('Ctrl Pts',(-17.1772184238653,-16.4375824178345,
6.88399864479192));
#16533=CARTESIAN_POINT('Ctrl Pts',(-17.3592350532944,-15.9800551998517,
6.90531266528233));
#16534=CARTESIAN_POINT('Ctrl Pts',(-17.4049999997715,-15.7410811218703,
6.91536691268471));
#16535=CARTESIAN_POINT('Ctrl Pts',(-17.405,-15.5000000018056,6.92449999993158));
#16536=CARTESIAN_POINT('Ctrl Pts',(-17.405,-15.4999999999999,6.98699999999991));
#16537=CARTESIAN_POINT('Ctrl Pts',(-17.405,-15.6943874704945,6.97963584918515));
#16538=CARTESIAN_POINT('Ctrl Pts',(-17.3752506427565,-15.8878971634581,
6.97165426613153));
#16539=CARTESIAN_POINT('Ctrl Pts',(-17.2414283784515,-16.3115578174224,
6.95267736232273));
#16540=CARTESIAN_POINT('Ctrl Pts',(-17.120368366469,-16.5322806509859,6.94166766910084));
#16541=CARTESIAN_POINT('Ctrl Pts',(-16.7975501002715,-16.9175902999785,
6.92000987918617));
#16542=CARTESIAN_POINT('Ctrl Pts',(-16.5977824941516,-17.0773521697487,
6.91002198137144));
#16543=CARTESIAN_POINT('Ctrl Pts',(-16.156625631238,-17.3046970326897,6.89072378089403));
#16544=CARTESIAN_POINT('Ctrl Pts',(-15.9212944056835,-17.3736536130528,
6.88042932658281));
#16545=CARTESIAN_POINT('Ctrl Pts',(-15.4280081963133,-17.4203124218493,
6.85885075224467));
#16546=CARTESIAN_POINT('Ctrl Pts',(-15.174381278281,-17.3938754826517,6.84775596142961));
#16547=CARTESIAN_POINT('Ctrl Pts',(-14.69955590838,-17.2459242149106,6.82698494787315));
#16548=CARTESIAN_POINT('Ctrl Pts',(-14.4820651847725,-17.1287321615361,
6.81810481278379));
#16549=CARTESIAN_POINT('Ctrl Pts',(-14.102551540606,-16.8177953917989,6.79802449941344));
#16550=CARTESIAN_POINT('Ctrl Pts',(-13.9443589834925,-16.6266828292324,
6.78732438512114));
#16551=CARTESIAN_POINT('Ctrl Pts',(-13.7061578526639,-16.1891108490807,
6.76553746402708));
#16552=CARTESIAN_POINT('Ctrl Pts',(-13.6307204217205,-15.9455969914062,
6.75466222770199));
#16553=CARTESIAN_POINT('Ctrl Pts',(-13.5803266843897,-15.4544806575515,
6.73495461221655));
#16554=CARTESIAN_POINT('Ctrl Pts',(-13.6015021726823,-15.2120161132821,
6.72594783691514));
#16555=CARTESIAN_POINT('Ctrl Pts',(-13.735237407317,-14.7407603202715,6.70516974829986));
#16556=CARTESIAN_POINT('Ctrl Pts',(-13.8492739824694,-14.5171820856897,
6.6942054998984));
#16557=CARTESIAN_POINT('Ctrl Pts',(-14.1591310117816,-14.1234803305985,
6.67251327609788));
#16558=CARTESIAN_POINT('Ctrl Pts',(-14.3530787555558,-13.9581645755139,
6.66217153300273));
#16559=CARTESIAN_POINT('Ctrl Pts',(-14.7852233534807,-13.717638997849,6.64326756983889));
#16560=CARTESIAN_POINT('Ctrl Pts',(-15.0174283305894,-13.6412861257118,
6.63310987180263));
#16561=CARTESIAN_POINT('Ctrl Pts',(-15.507270799116,-13.5784654785805,6.61168194229578));
#16562=CARTESIAN_POINT('Ctrl Pts',(-15.7607595796635,-13.5962252141327,
6.60059319424033));
#16563=CARTESIAN_POINT('Ctrl Pts',(-16.2413554964388,-13.7279224646686,
6.57956975081185));
#16564=CARTESIAN_POINT('Ctrl Pts',(-16.4643034860068,-13.8386814298334,
6.57051235094214));
#16565=CARTESIAN_POINT('Ctrl Pts',(-16.8543319185472,-14.1380699108652,
6.55063954926042));
#16566=CARTESIAN_POINT('Ctrl Pts',(-17.0180921883204,-14.3233740897399,
6.54003770056315));
#16567=CARTESIAN_POINT('Ctrl Pts',(-17.2713800244962,-14.7542397872394,
6.51817485901714));
#16568=CARTESIAN_POINT('Ctrl Pts',(-17.3551426119534,-14.9975970924926,
6.50712346346707));
#16569=CARTESIAN_POINT('Ctrl Pts',(-17.3995286879098,-15.3332027678794,
6.49343859564043));
#16570=CARTESIAN_POINT('Ctrl Pts',(-17.405,-15.416638718226,6.49015804845609));
#16571=CARTESIAN_POINT('Ctrl Pts',(-17.405,-15.4999999999999,6.48699999999991));
#16572=CARTESIAN_POINT('Origin',(-15.5,-15.5,-1.713));
#16573=CARTESIAN_POINT('',(-17.405,-15.5,5.92449999999997));
#16574=CARTESIAN_POINT('',(-17.405,-15.5000000034284,5.98699999974014));
#16575=CARTESIAN_POINT('',(-17.405,-15.5,-1.713));
#16576=CARTESIAN_POINT('Ctrl Pts',(-17.405,-15.5,5.92449999999997));
#16577=CARTESIAN_POINT('Ctrl Pts',(-17.405,-15.4144176700989,5.92774219036784));
#16578=CARTESIAN_POINT('Ctrl Pts',(-17.3992332699381,-15.3287564795742,
5.93111349973546));
#16579=CARTESIAN_POINT('Ctrl Pts',(-17.3546716311612,-15.0006921244555,
5.94451651307743));
#16580=CARTESIAN_POINT('Ctrl Pts',(-17.2751038305769,-14.7664430467097,
5.95513110417249));
#16581=CARTESIAN_POINT('Ctrl Pts',(-17.0267333284629,-14.3324868603746,
5.97700347217566));
#16582=CARTESIAN_POINT('Ctrl Pts',(-16.8569786447406,-14.1388871358369,
5.98805069971181));
#16583=CARTESIAN_POINT('Ctrl Pts',(-16.4619306836403,-13.8380453788742,
6.00808834558228));
#16584=CARTESIAN_POINT('Ctrl Pts',(-16.2436228778207,-13.7295663669768,
6.01697056527465));
#16585=CARTESIAN_POINT('Ctrl Pts',(-15.7719223056613,-13.5982668894319,
6.03760488601653));
#16586=CARTESIAN_POINT('Ctrl Pts',(-15.5223056300077,-13.5790558352873,
6.04852425061521));
#16587=CARTESIAN_POINT('Ctrl Pts',(-15.0352776596755,-13.6367139569718,
6.06982906121628));
#16588=CARTESIAN_POINT('Ctrl Pts',(-14.8021355362915,-13.7109192081023,
6.0800277543179));
#16589=CARTESIAN_POINT('Ctrl Pts',(-14.3675310337485,-13.9475127920323,
6.09903932485781));
#16590=CARTESIAN_POINT('Ctrl Pts',(-14.1720287921778,-14.1110291910389,
6.10925947498833));
#16591=CARTESIAN_POINT('Ctrl Pts',(-13.8583617609821,-14.5020202981999,
6.13093234231348));
#16592=CARTESIAN_POINT('Ctrl Pts',(-13.7421793491084,-14.7247517553509,
6.1419114458153));
#16593=CARTESIAN_POINT('Ctrl Pts',(-13.6041850136687,-15.1949217251059,
6.16274155542265));
#16594=CARTESIAN_POINT('Ctrl Pts',(-13.5808290435917,-15.4370968267385,
6.17180703306081));
#16595=CARTESIAN_POINT('Ctrl Pts',(-13.6267406199668,-15.9285535022321,
6.19142950699013));
#16596=CARTESIAN_POINT('Ctrl Pts',(-13.6999541275731,-16.1727358500583,
6.20228142607045));
#16597=CARTESIAN_POINT('Ctrl Pts',(-13.9342528540802,-16.612643260009,6.22407146787201));
#16598=CARTESIAN_POINT('Ctrl Pts',(-14.0908682124153,-16.8053351301606,
6.23479691554574));
#16599=CARTESIAN_POINT('Ctrl Pts',(-14.4674616885799,-17.119446886757,6.25493363903315));
#16600=CARTESIAN_POINT('Ctrl Pts',(-14.6834759111022,-17.2383997168824,
6.26378153591858));
#16601=CARTESIAN_POINT('Ctrl Pts',(-15.1566843563942,-17.3907795398349,
6.28448181786488));
#16602=CARTESIAN_POINT('Ctrl Pts',(-15.4102989723853,-17.419598005697,6.29557607053292));
#16603=CARTESIAN_POINT('Ctrl Pts',(-15.9044371223974,-17.3773918906524,
6.3171919126157));
#16604=CARTESIAN_POINT('Ctrl Pts',(-16.1405836197149,-17.3104815732564,
6.3275220306086));
#16605=CARTESIAN_POINT('Ctrl Pts',(-16.5831726506165,-17.0872896027469,
6.34688288060429));
#16606=CARTESIAN_POINT('Ctrl Pts',(-16.7837641373552,-16.9299401273163,
6.35674048961191));
#16607=CARTESIAN_POINT('Ctrl Pts',(-17.1100623193184,-16.5483409084119,
6.37833382769666));
#16608=CARTESIAN_POINT('Ctrl Pts',(-17.2334173550748,-16.3286040401448,
6.38935636610198));
#16609=CARTESIAN_POINT('Ctrl Pts',(-17.3733223438246,-15.9001673121539,
6.40864724907353));
#16610=CARTESIAN_POINT('Ctrl Pts',(-17.405,-15.700587196877,6.41690097952011));
#16611=CARTESIAN_POINT('Ctrl Pts',(-17.405,-15.4999999999999,6.42449999999997));
#16612=CARTESIAN_POINT('Ctrl Pts',(-17.405,-15.4999999999999,6.48699999999991));
#16613=CARTESIAN_POINT('Ctrl Pts',(-17.405,-15.6573653676441,6.48103838993624));
#16614=CARTESIAN_POINT('Ctrl Pts',(-17.3855039144757,-15.8144320154612,
6.47466167296953));
#16615=CARTESIAN_POINT('Ctrl Pts',(-17.2858671110078,-16.2079255525943,
6.45757532996358));
#16616=CARTESIAN_POINT('Ctrl Pts',(-17.1786901034823,-16.434062405774,6.44666418546016));
#16617=CARTESIAN_POINT('Ctrl Pts',(-16.8811149668584,-16.8361165529484,
6.42492417349771));
#16618=CARTESIAN_POINT('Ctrl Pts',(-16.6921893369319,-17.0071153860193,
6.41431384329561));
#16619=CARTESIAN_POINT('Ctrl Pts',(-16.2679653059451,-17.2599951864708,
6.3954550354746));
#16620=CARTESIAN_POINT('Ctrl Pts',(-16.0388328778226,-17.3431118415628,
6.38557099203068));
#16621=CARTESIAN_POINT('Ctrl Pts',(-15.5525225818871,-17.4207271638321,
6.36429757576055));
#16622=CARTESIAN_POINT('Ctrl Pts',(-15.2994157965646,-17.410947629751,6.35322553790743));
#16623=CARTESIAN_POINT('Ctrl Pts',(-14.813683679078,-17.2943880200312,6.33197741378292));
#16624=CARTESIAN_POINT('Ctrl Pts',(-14.5856038048897,-17.1895935173748,
6.32267510107439));
#16625=CARTESIAN_POINT('Ctrl Pts',(-14.186058208372,-16.9008155654491,6.30299610541913));
#16626=CARTESIAN_POINT('Ctrl Pts',(-14.0174177953425,-16.7209255269853,
6.2924926255542));
#16627=CARTESIAN_POINT('Ctrl Pts',(-13.7521525220174,-16.2991036698075,
6.27071042604193));
#16628=CARTESIAN_POINT('Ctrl Pts',(-13.6612898194952,-16.0591930631974,
6.25963430919053));
#16629=CARTESIAN_POINT('Ctrl Pts',(-13.5808752867126,-15.5692252954415,
6.23931358301802));
#16630=CARTESIAN_POINT('Ctrl Pts',(-13.5876496855473,-15.3246422120223,
6.23051753534931));
#16631=CARTESIAN_POINT('Ctrl Pts',(-13.69358258658,-14.8465705637078,6.21008933575238));
#16632=CARTESIAN_POINT('Ctrl Pts',(-13.7935051225893,-14.6179683833791,
6.19924346683156));
#16633=CARTESIAN_POINT('Ctrl Pts',(-14.0780384376739,-14.2074310799854,
6.17746733422077));
#16634=CARTESIAN_POINT('Ctrl Pts',(-14.2615952673923,-14.0306168913634,
6.16675412363653));
#16635=CARTESIAN_POINT('Ctrl Pts',(-14.6774696299874,-13.7648903345165,
6.1475912570579));
#16636=CARTESIAN_POINT('Ctrl Pts',(-14.9034802016442,-13.6747996097228,
6.13809447936804));
#16637=CARTESIAN_POINT('Ctrl Pts',(-15.3858696864533,-13.5820526462828,
6.11699257714542));
#16638=CARTESIAN_POINT('Ctrl Pts',(-15.638328177964,-13.583645740638,6.10594889860164));
#16639=CARTESIAN_POINT('Ctrl Pts',(-16.1291525866983,-13.6844547122694,
6.08447801458002));
#16640=CARTESIAN_POINT('Ctrl Pts',(-16.3626155095225,-13.7830517490666,
6.07484396541252));
#16641=CARTESIAN_POINT('Ctrl Pts',(-16.7790766551765,-14.06587592793,6.0550205403597));
#16642=CARTESIAN_POINT('Ctrl Pts',(-16.9576323622296,-14.2477879182273,
6.0442235911034));
#16643=CARTESIAN_POINT('Ctrl Pts',(-17.2301952244117,-14.665614301179,6.02243314083661));
#16644=CARTESIAN_POINT('Ctrl Pts',(-17.3235315529603,-14.8962457352792,
6.01165445119898));
#16645=CARTESIAN_POINT('Ctrl Pts',(-17.3934468662726,-15.2577349531895,
5.99643063218933));
#16646=CARTESIAN_POINT('Ctrl Pts',(-17.405000000436,-15.3788627644953,5.99158914799085));
#16647=CARTESIAN_POINT('Ctrl Pts',(-17.405,-15.5000000068569,5.98699999974014));
#16648=CARTESIAN_POINT('Origin',(-15.5,-15.5,-1.713));
#16649=CARTESIAN_POINT('',(-17.405,-15.5,5.42449999999996));
#16650=CARTESIAN_POINT('',(-17.405,-15.5,5.48699999999989));
#16651=CARTESIAN_POINT('',(-17.405,-15.5,-1.713));
#16652=CARTESIAN_POINT('Ctrl Pts',(-17.405,-15.5,5.42449999999996));
#16653=CARTESIAN_POINT('Ctrl Pts',(-17.405,-15.3760434359275,5.42919595509413));
#16654=CARTESIAN_POINT('Ctrl Pts',(-17.3929028862534,-15.2521105344024,
5.43415560504857));
#16655=CARTESIAN_POINT('Ctrl Pts',(-17.3208126200574,-14.8880510179744,
5.44952436807631));
#16656=CARTESIAN_POINT('Ctrl Pts',(-17.226391501484,-14.6577403242684,5.46031463364058));
#16657=CARTESIAN_POINT('Ctrl Pts',(-16.9518486544494,-14.2410878161607,
5.48210391973371));
#16658=CARTESIAN_POINT('Ctrl Pts',(-16.7724610386279,-14.0600036767685,
5.49288770244791));
#16659=CARTESIAN_POINT('Ctrl Pts',(-16.3629640389708,-13.7846532854336,
5.5122756697999));
#16660=CARTESIAN_POINT('Ctrl Pts',(-16.1392237783365,-13.6893274580866,
5.52153745501584));
#16661=CARTESIAN_POINT('Ctrl Pts',(-15.659834124758,-13.5853971651835,5.5425081310254));
#16662=CARTESIAN_POINT('Ctrl Pts',(-15.408023639897,-13.5809403932743,5.55352346282159));
#16663=CARTESIAN_POINT('Ctrl Pts',(-14.913556107456,-13.6699452666455,5.57515371358453));
#16664=CARTESIAN_POINT('Ctrl Pts',(-14.6760350732985,-13.7638927857631,
5.58508484305015));
#16665=CARTESIAN_POINT('Ctrl Pts',(-14.2598042431201,-14.033696179453,5.6044099527637));
#16666=CARTESIAN_POINT('Ctrl Pts',(-14.0830030766772,-14.203762905526,5.61471978164992));
#16667=CARTESIAN_POINT('Ctrl Pts',(-13.79741831993,-14.6089053564775,5.63631453375179));
#16668=CARTESIAN_POINT('Ctrl Pts',(-13.6943846727369,-14.8422789569263,
5.64740920961171));
#16669=CARTESIAN_POINT('Ctrl Pts',(-13.5870911327856,-15.3278163767363,
5.66815000182601));
#16670=CARTESIAN_POINT('Ctrl Pts',(-13.5808071130259,-15.5745934078983,
5.67701545681125));
#16671=CARTESIAN_POINT('Ctrl Pts',(-13.6621313310384,-16.0583284637951,
5.69711996057826));
#16672=CARTESIAN_POINT('Ctrl Pts',(-13.7494664034097,-16.2906393684339,
5.70783101399816));
#16673=CARTESIAN_POINT('Ctrl Pts',(-14.0110168099278,-16.7147717784116,
5.72961949365117));
#16674=CARTESIAN_POINT('Ctrl Pts',(-14.1849125956826,-16.9011803082986,
5.74048486614643));
#16675=CARTESIAN_POINT('Ctrl Pts',(-14.586121554684,-17.1887935215797,5.76015611849404));
#16676=CARTESIAN_POINT('Ctrl Pts',(-14.8070478925458,-17.2908173313166,
5.76918713440696));
#16677=CARTESIAN_POINT('Ctrl Pts',(-15.2825443775373,-17.408819662251,5.78998750557895));
#16678=CARTESIAN_POINT('Ctrl Pts',(-15.5333346762825,-17.4208758725757,
5.80095820981103));
#16679=CARTESIAN_POINT('Ctrl Pts',(-16.0290349471213,-17.3473935266342,
5.8226423861382));
#16680=CARTESIAN_POINT('Ctrl Pts',(-16.2688452203251,-17.2611273017974,
5.83293139227933));
#16681=CARTESIAN_POINT('Ctrl Pts',(-16.6922941478763,-17.0053894491118,
5.8518815209281));
#16682=CARTESIAN_POINT('Ctrl Pts',(-16.8739280570934,-16.8416634991693,
5.8620568396734));
#16683=CARTESIAN_POINT('Ctrl Pts',(-17.1717436625757,-16.4474570381807,
5.88350481046489));
#16684=CARTESIAN_POINT('Ctrl Pts',(-17.2821880097861,-16.2184804825159,
5.89459499802755));
#16685=CARTESIAN_POINT('Ctrl Pts',(-17.3849003572026,-15.8192563713138,
5.9119657065058));
#16686=CARTESIAN_POINT('Ctrl Pts',(-17.405,-15.6597824535574,5.91844682135343));
#16687=CARTESIAN_POINT('Ctrl Pts',(-17.405,-15.5,5.92449999999997));
#16688=CARTESIAN_POINT('Ctrl Pts',(-17.405,-15.5000000068569,5.98699999974013));
#16689=CARTESIAN_POINT('Ctrl Pts',(-17.4049999995636,-15.6212520006587,
5.98240650424101));
#16690=CARTESIAN_POINT('Ctrl Pts',(-17.3934249672455,-15.7424940251675,
5.97756021424145));
#16691=CARTESIAN_POINT('Ctrl Pts',(-17.3221315854689,-16.1107514310504,
5.9620498485584));
#16692=CARTESIAN_POINT('Ctrl Pts',(-17.2248764986786,-16.3473310510096,
5.95096010646316));
#16693=CARTESIAN_POINT('Ctrl Pts',(-16.9489044613018,-16.7605841853532,
5.92926834219268));
#16694=CARTESIAN_POINT('Ctrl Pts',(-16.7759444872425,-16.935403161333,5.91886249524204));
#16695=CARTESIAN_POINT('Ctrl Pts',(-16.3676999304369,-17.2143489102531,
5.89936571557253));
#16696=CARTESIAN_POINT('Ctrl Pts',(-16.1347682830141,-17.313555727457,5.88976764142664));
#16697=CARTESIAN_POINT('Ctrl Pts',(-15.6444331987704,-17.4159141380227,
5.86831816267583));
#16698=CARTESIAN_POINT('Ctrl Pts',(-15.3918998457965,-17.4183069254304,
5.8572712093524));
#16699=CARTESIAN_POINT('Ctrl Pts',(-14.9091203529905,-17.3270377526458,
5.83615224641251));
#16700=CARTESIAN_POINT('Ctrl Pts',(-14.6828074455978,-17.2376334387652,
5.82662110337859));
#16701=CARTESIAN_POINT('Ctrl Pts',(-14.2661037299997,-16.9731704217253,
5.80748796475579));
#16702=CARTESIAN_POINT('Ctrl Pts',(-14.0820088260293,-16.7969225078747,
5.7967844379516));
#16703=CARTESIAN_POINT('Ctrl Pts',(-13.7961776710268,-16.3872035965591,
5.77501092250489));
#16704=CARTESIAN_POINT('Ctrl Pts',(-13.6955369747897,-16.1588346230077,
5.76415818056918));
#16705=CARTESIAN_POINT('Ctrl Pts',(-13.5881963560233,-15.6810970911766,
5.74371184862297));
#16706=CARTESIAN_POINT('Ctrl Pts',(-13.5806847269442,-15.4366308122503,
5.73491243701307));
#16707=CARTESIAN_POINT('Ctrl Pts',(-13.6595783657715,-14.9464290612334,
5.71461611204482));
#16708=CARTESIAN_POINT('Ctrl Pts',(-13.7497409224647,-14.7061669365763,
5.70354199210313));
#16709=CARTESIAN_POINT('Ctrl Pts',(-14.0138290100348,-14.2834314875499,
5.68175092991055));
#16710=CARTESIAN_POINT('Ctrl Pts',(-14.1819919720835,-14.1029975163744,
5.67123728670109));
#16711=CARTESIAN_POINT('Ctrl Pts',(-14.5805926662016,-13.8131593223387,
5.65153879212186));
#16712=CARTESIAN_POINT('Ctrl Pts',(-14.8081547979217,-13.7077660171985,
5.64226444453527));
#16713=CARTESIAN_POINT('Ctrl Pts',(-15.2933813077319,-13.5896850205772,
5.62103843798188));
#16714=CARTESIAN_POINT('Ctrl Pts',(-15.5465373051868,-13.5791082285566,
5.60996424736706));
#16715=CARTESIAN_POINT('Ctrl Pts',(-16.0332209521069,-13.6552489250426,
5.58867449903284));
#16716=CARTESIAN_POINT('Ctrl Pts',(-16.262660718492,-13.7376920430767,5.57874860458176));
#16717=CARTESIAN_POINT('Ctrl Pts',(-16.6876819207768,-13.9893307180406,
5.55991937946208));
#16718=CARTESIAN_POINT('Ctrl Pts',(-16.8771141741595,-14.1597611584412,
5.54931950117439));
#16719=CARTESIAN_POINT('Ctrl Pts',(-17.1759309590692,-14.560977049772,5.52758408793076));
#16720=CARTESIAN_POINT('Ctrl Pts',(-17.283803098501,-14.7868647889453,5.5166671767215));
#16721=CARTESIAN_POINT('Ctrl Pts',(-17.3850463837683,-15.181917730531,5.49948662003355));
#16722=CARTESIAN_POINT('Ctrl Pts',(-17.405,-15.3407987939666,5.49303115873733));
#16723=CARTESIAN_POINT('Ctrl Pts',(-17.405,-15.5,5.48699999999989));
#16724=CARTESIAN_POINT('Origin',(-15.5,-15.5,-1.713));
#16725=CARTESIAN_POINT('',(-17.405,-15.5,4.92449999999995));
#16726=CARTESIAN_POINT('',(-17.405,-15.5,4.98699999999988));
#16727=CARTESIAN_POINT('',(-17.405,-15.5,-1.713));
#16728=CARTESIAN_POINT('Ctrl Pts',(-17.405,-15.5000000000001,4.92449999999995));
#16729=CARTESIAN_POINT('Ctrl Pts',(-17.405,-15.3380084622269,4.93063686731884));
#16730=CARTESIAN_POINT('Ctrl Pts',(-17.3843408041619,-15.1763710006228,
4.93721218428607));
#16731=CARTESIAN_POINT('Ctrl Pts',(-17.2806376985815,-14.7789600840496,
4.95453587205002));
#16732=CARTESIAN_POINT('Ctrl Pts',(-17.1717102736454,-14.5534548816947,
4.96546137276711));
#16733=CARTESIAN_POINT('Ctrl Pts',(-16.8710112518389,-14.1535201252274,
4.98718942044254));
#16734=CARTESIAN_POINT('Ctrl Pts',(-16.6808125325853,-13.983956326939,4.99777323131334));
#16735=CARTESIAN_POINT('Ctrl Pts',(-16.2545819583126,-13.7342053939596,
5.01655739315566));
#16736=CARTESIAN_POINT('Ctrl Pts',(-16.0246727565372,-13.6527867878846,
5.02654843584694));
#16737=CARTESIAN_POINT('Ctrl Pts',(-15.5374231761305,-13.5788933923025,
5.04786294067662));
#16738=CARTESIAN_POINT('Ctrl Pts',(-15.2841969270122,-13.5906848771702,
5.05894020441759));
#16739=CARTESIAN_POINT('Ctrl Pts',(-14.7997439961544,-13.7110798223801,
5.08013237112176));
#16740=CARTESIAN_POINT('Ctrl Pts',(-14.5729685123419,-13.8173840698908,
5.08936559945493));
#16741=CARTESIAN_POINT('Ctrl Pts',(-14.1758098743663,-14.1088374455546,
5.10909374233906));
#16742=CARTESIAN_POINT('Ctrl Pts',(-14.0083786203189,-14.2900988616466,
5.11962272825705));
#16743=CARTESIAN_POINT('Ctrl Pts',(-13.7460922865542,-14.7142219875609,
5.14142695259023));
#16744=CARTESIAN_POINT('Ctrl Pts',(-13.6570003466679,-14.9550166456319,
5.15249783014614));
#16745=CARTESIAN_POINT('Ctrl Pts',(-13.5804275330516,-15.4455720839554,
5.17275679245414));
#16746=CARTESIAN_POINT('Ctrl Pts',(-13.5890640079251,-15.6898618051801,
5.18156286747393));
#16747=CARTESIAN_POINT('Ctrl Pts',(-13.6985559912454,-16.1670865051149,
5.2020368265779));
#16748=CARTESIAN_POINT('Ctrl Pts',(-13.8002936525146,-16.3950946904093,
5.21289989356697));
#16749=CARTESIAN_POINT('Ctrl Pts',(-14.088104367486,-16.8035545086014,5.23466900714812));
#16750=CARTESIAN_POINT('Ctrl Pts',(-14.2730183848475,-16.9789334799628,
5.24535753090881));
#16751=CARTESIAN_POINT('Ctrl Pts',(-14.6909876344324,-17.2414631089392,
5.26444510539403));
#16752=CARTESIAN_POINT('Ctrl Pts',(-14.9177651172584,-17.3298174134956,
5.27403040757896));
#16753=CARTESIAN_POINT('Ctrl Pts',(-15.4011395799388,-17.4188210052778,
5.29517539719754));
#16754=CARTESIAN_POINT('Ctrl Pts',(-15.6537828372131,-17.4152022158959,
5.30622715823318));
#16755=CARTESIAN_POINT('Ctrl Pts',(-16.1433642866381,-17.3104730906201,
5.32764366958161));
#16756=CARTESIAN_POINT('Ctrl Pts',(-16.375483745341,-17.2103334121474,5.33718808787432));
#16757=CARTESIAN_POINT('Ctrl Pts',(-16.7822911123883,-16.9297542878312,
5.35671531153807));
#16758=CARTESIAN_POINT('Ctrl Pts',(-16.9545470277676,-16.7540897545839,
5.36713779211663));
#16759=CARTESIAN_POINT('Ctrl Pts',(-17.2287667612673,-16.3394015430889,
5.38884559581544));
#16760=CARTESIAN_POINT('Ctrl Pts',(-17.3249725708871,-16.1022598955999,
5.39993367962256));
#16761=CARTESIAN_POINT('Ctrl Pts',(-17.3939902026772,-15.7365117366992,
5.4152992094953));
#16762=CARTESIAN_POINT('Ctrl Pts',(-17.405,-15.6182543353654,5.42002006743066));
#16763=CARTESIAN_POINT('Ctrl Pts',(-17.405,-15.5,5.42449999999996));
#16764=CARTESIAN_POINT('Ctrl Pts',(-17.405,-15.5,5.48699999999989));
#16765=CARTESIAN_POINT('Ctrl Pts',(-17.405,-15.5814768755342,5.4839133401559));
#16766=CARTESIAN_POINT('Ctrl Pts',(-17.3997732389571,-15.6630288598788,
5.4807095137914));
#16767=CARTESIAN_POINT('Ctrl Pts',(-17.3566182979129,-15.9969615452074,
5.46711495302279));
#16768=CARTESIAN_POINT('Ctrl Pts',(-17.2735392416782,-16.2406370700203,
5.45606645245911));
#16769=CARTESIAN_POINT('Ctrl Pts',(-17.021409045366,-16.6723479860623,5.4341969109657));
#16770=CARTESIAN_POINT('Ctrl Pts',(-16.8581230029901,-16.8581616545989,
5.42358613325307));
#16771=CARTESIAN_POINT('Ctrl Pts',(-16.4690036002391,-17.1585557089554,
5.40369511909761));
#16772=CARTESIAN_POINT('Ctrl Pts',(-16.2465361768677,-17.2698769738081,
5.39465687562847));
#16773=CARTESIAN_POINT('Ctrl Pts',(-15.7664355311582,-17.4029987099506,
5.37365509760093));
#16774=CARTESIAN_POINT('Ctrl Pts',(-15.5129232590213,-17.4215146350884,
5.36256532191691));
#16775=CARTESIAN_POINT('Ctrl Pts',(-15.0227594117968,-17.3600985674522,
5.34112333384936));
#16776=CARTESIAN_POINT('Ctrl Pts',(-14.7902722396957,-17.2843865373322,
5.33095329132526));
#16777=CARTESIAN_POINT('Ctrl Pts',(-14.3573886143867,-17.0450337541717,
5.31201699975444));
#16778=CARTESIAN_POINT('Ctrl Pts',(-14.162974515436,-16.8802544045959,5.30171227628098));
#16779=CARTESIAN_POINT('Ctrl Pts',(-13.8519761651499,-16.4873592914475,
5.28002564792785));
#16780=CARTESIAN_POINT('Ctrl Pts',(-13.7372974953326,-16.2640320949588,
5.26905686575707));
#16781=CARTESIAN_POINT('Ctrl Pts',(-13.6022888935652,-15.7930997383418,
5.2482631787414));
#16782=CARTESIAN_POINT('Ctrl Pts',(-13.5804608845042,-15.5507227020883,
5.23923957595381));
#16783=CARTESIAN_POINT('Ctrl Pts',(-13.6295123736636,-15.0595029086655,
5.21955739902793));
#16784=CARTESIAN_POINT('Ctrl Pts',(-13.7042844979505,-14.8157866894146,
5.20868904822613));
#16785=CARTESIAN_POINT('Ctrl Pts',(-13.941319488103,-14.3775117194336,5.18690100129162));
#16786=CARTESIAN_POINT('Ctrl Pts',(-14.0990413745835,-14.1859249151819,
5.17619321551943));
#16787=CARTESIAN_POINT('Ctrl Pts',(-14.4776810473978,-13.8740364453775,
5.15609596379566));
#16788=CARTESIAN_POINT('Ctrl Pts',(-14.6947281052106,-13.7563163073901,
5.1472262421167));
#16789=CARTESIAN_POINT('Ctrl Pts',(-15.1690701263999,-13.6070357747158,
5.12647637242337));
#16790=CARTESIAN_POINT('Ctrl Pts',(-15.4226956206289,-13.5798847323188,
5.11538164389191));
#16791=CARTESIAN_POINT('Ctrl Pts',(-15.9162414890316,-13.6252091599672,
5.09379171089091));
#16792=CARTESIAN_POINT('Ctrl Pts',(-16.1518191026795,-13.6935529003981,
5.08348647844787));
#16793=CARTESIAN_POINT('Ctrl Pts',(-16.5934068526385,-13.9196514534064,
5.06416942901834));
#16794=CARTESIAN_POINT('Ctrl Pts',(-16.7934223159308,-14.078687343901,5.05422142208812));
#16795=CARTESIAN_POINT('Ctrl Pts',(-17.1172886667511,-14.4628832908677,
5.03258289953719));
#16796=CARTESIAN_POINT('Ctrl Pts',(-17.2390389883794,-14.6833123338815,
5.02156923760385));
#16797=CARTESIAN_POINT('Ctrl Pts',(-17.3746778120002,-15.1084162217768,
5.00249792623135));
#16798=CARTESIAN_POINT('Ctrl Pts',(-17.405,-15.3037503177909,4.9944346986122));
#16799=CARTESIAN_POINT('Ctrl Pts',(-17.405,-15.5000000000001,4.98699999999988));
#16800=CARTESIAN_POINT('Origin',(-15.5,-15.5,-1.713));
#16801=CARTESIAN_POINT('',(-17.405,-15.5,4.42449999999995));
#16802=CARTESIAN_POINT('',(-17.405,-15.4999999574994,4.48700000322005));
#16803=CARTESIAN_POINT('',(-17.405,-15.5,-1.713));
#16804=CARTESIAN_POINT('Ctrl Pts',(-17.405,-15.5000000000001,4.42449999999995));
#16805=CARTESIAN_POINT('Ctrl Pts',(-17.405,-15.300946180348,4.43204093020726));
#16806=CARTESIAN_POINT('Ctrl Pts',(-17.3738049147864,-15.1028665454003,
4.44022726172271));
#16807=CARTESIAN_POINT('Ctrl Pts',(-17.2354136557939,-14.6756034049486,
4.45944057594965));
#16808=CARTESIAN_POINT('Ctrl Pts',(-17.1126253999981,-14.4556205858719,
4.47046003516288));
#16809=CARTESIAN_POINT('Ctrl Pts',(-16.7871854121762,-14.0731029611838,
4.49206939536787));
#16810=CARTESIAN_POINT('Ctrl Pts',(-16.586797360482,-13.9151580380625,4.50195855815905));
#16811=CARTESIAN_POINT('Ctrl Pts',(-16.1445619233844,-13.6909379581971,
4.52130394035929));
#16812=CARTESIAN_POINT('Ctrl Pts',(-15.90861573014,-13.6235199477863,4.53162529614427));
#16813=CARTESIAN_POINT('Ctrl Pts',(-15.4146849504325,-13.5802098264281,
4.55323206691012));
#16814=CARTESIAN_POINT('Ctrl Pts',(-15.1610652756953,-13.6084381761364,
4.56432654087063));
#16815=CARTESIAN_POINT('Ctrl Pts',(-14.6874548542244,-13.7597218463035,
4.58504440707669));
#16816=CARTESIAN_POINT('Ctrl Pts',(-14.4710755985286,-13.8782384657527,
4.59389962874866));
#16817=CARTESIAN_POINT('Ctrl Pts',(-14.0937570674529,-14.1915632010929,
4.61402239541429));
#16818=CARTESIAN_POINT('Ctrl Pts',(-13.9367488918255,-14.383864345526,4.62474163268767));
#16819=CARTESIAN_POINT('Ctrl Pts',(-13.7014796361299,-14.8231954715791,
4.64653107029409));
#16820=CARTESIAN_POINT('Ctrl Pts',(-13.6277136965757,-15.0672138774326,
4.65738886155556));
#16821=CARTESIAN_POINT('Ctrl Pts',(-13.5806899402637,-15.5585874680381,
4.67703251380268));
#16822=CARTESIAN_POINT('Ctrl Pts',(-13.6035044448897,-15.8008336512809,
4.6860827562014));
#16823=CARTESIAN_POINT('Ctrl Pts',(-13.7404400945265,-16.2712745947072,
4.70689997548424));
#16824=CARTESIAN_POINT('Ctrl Pts',(-13.8560896031551,-16.4942184303239,
4.71787546890398));
#16825=CARTESIAN_POINT('Ctrl Pts',(-14.1688115759052,-16.8858866889789,
4.73955331878264));
#16826=CARTESIAN_POINT('Ctrl Pts',(-14.3639288494479,-17.0498517421699,
4.74980309927576));
#16827=CARTESIAN_POINT('Ctrl Pts',(-14.7979250943807,-17.2874251666292,
4.76878806187125));
#16828=CARTESIAN_POINT('Ctrl Pts',(-15.0308360672455,-17.3621653543147,
4.77897664336141));
#16829=CARTESIAN_POINT('Ctrl Pts',(-15.521478859006,-17.4214529261841,4.80043958263354));
#16830=CARTESIAN_POINT('Ctrl Pts',(-15.7750225343709,-17.4017918333695,
4.81153073203709));
#16831=CARTESIAN_POINT('Ctrl Pts',(-16.2543703574976,-17.2665159232243,
4.83249957819312));
#16832=CARTESIAN_POINT('Ctrl Pts',(-16.4761118588062,-17.154343863983,4.84151015383185));
#16833=CARTESIAN_POINT('Ctrl Pts',(-16.8638520975196,-16.8524267802324,
4.86142870080129));
#16834=CARTESIAN_POINT('Ctrl Pts',(-17.0264160255427,-16.6658427318232,
4.87205286921227));
#16835=CARTESIAN_POINT('Ctrl Pts',(-17.2767855078975,-16.2328557607738,
4.89393224181132));
#16836=CARTESIAN_POINT('Ctrl Pts',(-17.3588258334554,-15.9887011344888,
4.9049761732021));
#16837=CARTESIAN_POINT('Ctrl Pts',(-17.4001334338982,-15.6573136012298,
4.91843390822054));
#16838=CARTESIAN_POINT('Ctrl Pts',(-17.405,-15.5786191688494,4.92152160116145));
#16839=CARTESIAN_POINT('Ctrl Pts',(-17.405,-15.5000000000001,4.92449999999995));
#16840=CARTESIAN_POINT('Ctrl Pts',(-17.405,-15.5000000000001,4.98699999999988));
#16841=CARTESIAN_POINT('Ctrl Pts',(-17.405,-15.5441523099634,4.98532733936716));
#16842=CARTESIAN_POINT('Ctrl Pts',(-17.4034650555517,-15.588348432899,4.98361944621604));
#16843=CARTESIAN_POINT('Ctrl Pts',(-17.3828269524683,-15.8843303780855,
4.97195510084708));
#16844=CARTESIAN_POINT('Ctrl Pts',(-17.3153906860251,-16.1301442874987,
4.96116773324529));
#16845=CARTESIAN_POINT('Ctrl Pts',(-17.0912870699373,-16.5759274289171,
4.93937808612846));
#16846=CARTESIAN_POINT('Ctrl Pts',(-16.9388204662768,-16.7726434333998,
4.92859093131468));
#16847=CARTESIAN_POINT('Ctrl Pts',(-16.5697988216603,-17.0949234111697,
4.90831037706324));
#16848=CARTESIAN_POINT('Ctrl Pts',(-16.3575362863681,-17.2183950289438,
4.89951252346313));
#16849=CARTESIAN_POINT('Ctrl Pts',(-15.8885431733751,-17.382089147163,4.87899663925522));
#16850=CARTESIAN_POINT('Ctrl Pts',(-15.6350588011372,-17.4170216974866,
4.86790808403922));
#16851=CARTESIAN_POINT('Ctrl Pts',(-15.1389165413175,-17.3862801935719,
4.84620457311099));
#16852=CARTESIAN_POINT('Ctrl Pts',(-14.9007609710995,-17.3246551866247,
4.83578656916445));
#16853=CARTESIAN_POINT('Ctrl Pts',(-14.4545564524755,-17.1120822196972,
4.81626756135064));
#16854=CARTESIAN_POINT('Ctrl Pts',(-14.2518816904769,-16.9608150588265,
4.80670882748964));
#16855=CARTESIAN_POINT('Ctrl Pts',(-13.9168450172487,-16.5886930567592,
4.78528339250663));
#16856=CARTESIAN_POINT('Ctrl Pts',(-13.7876907953647,-16.371566588569,4.77423290483257));
#16857=CARTESIAN_POINT('Ctrl Pts',(-13.623693143634,-15.9082831048492,4.75309493055782));
#16858=CARTESIAN_POINT('Ctrl Pts',(-13.5871296959008,-15.6676780010439,
4.74352443397239));
#16859=CARTESIAN_POINT('Ctrl Pts',(-13.6061249022657,-15.1744757364315,
4.72442455236517));
#16860=CARTESIAN_POINT('Ctrl Pts',(-13.6658641934304,-14.9267196306907,
4.7137319571291));
#16861=CARTESIAN_POINT('Ctrl Pts',(-13.8762571974879,-14.4735300670181,
4.69196160818337));
#16862=CARTESIAN_POINT('Ctrl Pts',(-14.023081911278,-14.2716258629011,4.68110130517412));
#16863=CARTESIAN_POINT('Ctrl Pts',(-14.3820348473883,-13.9386239728758,
4.66063478879943));
#16864=CARTESIAN_POINT('Ctrl Pts',(-14.5894703723234,-13.8092386072515,
4.65183069237424));
#16865=CARTESIAN_POINT('Ctrl Pts',(-15.0528208481337,-13.6308641948418,
4.63156164268873));
#16866=CARTESIAN_POINT('Ctrl Pts',(-15.305921621302,-13.5879444772796,4.62048986783447));
#16867=CARTESIAN_POINT('Ctrl Pts',(-15.8042860608109,-13.6036374054734,
4.59868914869584));
#16868=CARTESIAN_POINT('Ctrl Pts',(-16.0448845797942,-13.6582889446888,
4.58816427909903));
#16869=CARTESIAN_POINT('Ctrl Pts',(-16.4956875029771,-13.8570659644062,
4.56844411623013));
#16870=CARTESIAN_POINT('Ctrl Pts',(-16.7010308675647,-14.0006130954559,
4.55919998756135));
#16871=CARTESIAN_POINT('Ctrl Pts',(-17.0470873642231,-14.360456424669,4.53799868778837));
#16872=CARTESIAN_POINT('Ctrl Pts',(-17.1836196412927,-14.5740087589079,
4.52692222737616));
#16873=CARTESIAN_POINT('Ctrl Pts',(-17.3608848628781,-15.0285694828898,
4.50582451323252));
#16874=CARTESIAN_POINT('Ctrl Pts',(-17.4049999947116,-15.2633019929779,
4.4959670380467));
#16875=CARTESIAN_POINT('Ctrl Pts',(-17.405,-15.499999957438,4.48700000161229));
#16876=CARTESIAN_POINT('Origin',(-15.5,-15.5,-1.713));
#16877=CARTESIAN_POINT('',(-17.405,-15.4999999913089,3.92450000065845));
#16878=CARTESIAN_POINT('',(-17.405,-15.5,3.98699999999987));
#16879=CARTESIAN_POINT('',(-17.405,-15.5,-1.713));
#16880=CARTESIAN_POINT('Ctrl Pts',(-17.405,-15.4999999826177,3.92450000065845));
#16881=CARTESIAN_POINT('Ctrl Pts',(-17.4049999978143,-15.2604577159144,
3.9335747902183));
#16882=CARTESIAN_POINT('Ctrl Pts',(-17.359817730218,-15.0229721283851,3.94355990332549));
#16883=CARTESIAN_POINT('Ctrl Pts',(-17.1794744215171,-14.5664812063353,
3.96479806559331));
#16884=CARTESIAN_POINT('Ctrl Pts',(-17.0419187944687,-14.3534475582947,
3.97587725914485));
#16885=CARTESIAN_POINT('Ctrl Pts',(-16.6943411737859,-13.9953278652344,
3.99704653132888));
#16886=CARTESIAN_POINT('Ctrl Pts',(-16.4886247886422,-13.8528507646097,
4.00625307136287));
#16887=CARTESIAN_POINT('Ctrl Pts',(-16.0371837458011,-13.6560148499806,
4.02600114847753));
#16888=CARTESIAN_POINT('Ctrl Pts',(-15.7962570520486,-13.6023535784996,
4.03654037392603));
#16889=CARTESIAN_POINT('Ctrl Pts',(-15.297615099849,-13.5887906112471,4.05835323272741));
#16890=CARTESIAN_POINT('Ctrl Pts',(-15.0445879002524,-13.6328373649071,
4.06942178914021));
#16891=CARTESIAN_POINT('Ctrl Pts',(-14.5820463480311,-13.8132755459749,
4.08965545284191));
#16892=CARTESIAN_POINT('Ctrl Pts',(-14.3752851451608,-13.9434981112106,
4.09846707133362));
#16893=CARTESIAN_POINT('Ctrl Pts',(-14.0177708750154,-14.2780184110088,
4.11895964407112));
#16894=CARTESIAN_POINT('Ctrl Pts',(-13.8717630623921,-14.4806481670653,
4.12982956632042));
#16895=CARTESIAN_POINT('Ctrl Pts',(-13.6633412943098,-14.9348574141291,
4.15159542942769));
#16896=CARTESIAN_POINT('Ctrl Pts',(-13.6047019998018,-15.1828698074392,
4.1622736744108));
#16897=CARTESIAN_POINT('Ctrl Pts',(-13.5878892661774,-15.6761920399413,
4.18133036524241));
#16898=CARTESIAN_POINT('Ctrl Pts',(-13.6255339615237,-15.916682506097,4.19095339529093));
#16899=CARTESIAN_POINT('Ctrl Pts',(-13.7916727576322,-16.3793784160295,
4.21211594167251));
#16900=CARTESIAN_POINT('Ctrl Pts',(-13.9218837745339,-16.596010533555,4.223170815929));
#16901=CARTESIAN_POINT('Ctrl Pts',(-14.2585051113859,-16.9663893557281,
4.24456487268541));
#16902=CARTESIAN_POINT('Ctrl Pts',(-14.4615603940353,-17.1165497929753,
4.25407394549568));
#16903=CARTESIAN_POINT('Ctrl Pts',(-14.9084234963101,-17.3271671728719,
4.27362176274305));
#16904=CARTESIAN_POINT('Ctrl Pts',(-15.146936993668,-17.3878108216528,4.28405542404481));
#16905=CARTESIAN_POINT('Ctrl Pts',(-15.6434206839156,-17.4164292828546,
4.30577387068733));
#16906=CARTESIAN_POINT('Ctrl Pts',(-15.8968654809846,-17.3803672954393,
4.3168606947061));
#16907=CARTESIAN_POINT('Ctrl Pts',(-16.3650702726416,-17.2145908692008,
4.33734209416616));
#16908=CARTESIAN_POINT('Ctrl Pts',(-16.5766448830822,-17.0902845045195,
4.34613585570338));
#16909=CARTESIAN_POINT('Ctrl Pts',(-16.9442556557284,-16.7664921099221,
4.36644284719931));
#16910=CARTESIAN_POINT('Ctrl Pts',(-17.095939925573,-16.5690376427327,4.37724086642937));
#16911=CARTESIAN_POINT('Ctrl Pts',(-17.3181320330473,-16.1221883712515,
4.39902909366046));
#16912=CARTESIAN_POINT('Ctrl Pts',(-17.3844902892752,-15.8760866337007,
4.40980378678158));
#16913=CARTESIAN_POINT('Ctrl Pts',(-17.4036517297875,-15.5828007286006,
4.42133369774593));
#16914=CARTESIAN_POINT('Ctrl Pts',(-17.405,-15.5413804235327,4.42293234916886));
#16915=CARTESIAN_POINT('Ctrl Pts',(-17.405,-15.5000000000001,4.42449999999995));
#16916=CARTESIAN_POINT('Ctrl Pts',(-17.405,-15.499999957438,4.48700000161229));
#16917=CARTESIAN_POINT('Ctrl Pts',(-17.4050000001085,-15.5048557134102,
4.48681604675312));
#16918=CARTESIAN_POINT('Ctrl Pts',(-17.4049814345791,-15.5097122660366,
4.48663165565055));
#16919=CARTESIAN_POINT('Ctrl Pts',(-17.4030142719686,-15.7669161853031,
4.47684474798026));
#16920=CARTESIAN_POINT('Ctrl Pts',(-17.3509618993671,-16.0163535166326,
4.46625659172986));
#16921=CARTESIAN_POINT('Ctrl Pts',(-17.1544054843015,-16.4764685333068,
4.44452651733637));
#16922=CARTESIAN_POINT('Ctrl Pts',(-17.0133444914353,-16.6833609452157,
4.43360330731903));
#16923=CARTESIAN_POINT('Ctrl Pts',(-16.6644503982568,-17.02690772249,4.41295731943203));
#16924=CARTESIAN_POINT('Ctrl Pts',(-16.4616519094173,-17.1621103410901,
4.40406701266038));
#16925=CARTESIAN_POINT('Ctrl Pts',(-16.0039662811969,-17.3547409853283,
4.38404576908119));
#16926=CARTESIAN_POINT('Ctrl Pts',(-15.751473444106,-17.4054630353252,4.37300058810609));
#16927=CARTESIAN_POINT('Ctrl Pts',(-15.2513705135099,-17.4045485352596,
4.3511238194886));
#16928=CARTESIAN_POINT('Ctrl Pts',(-15.008583912302,-17.3567842193863,4.34050323325904));
#16929=CARTESIAN_POINT('Ctrl Pts',(-14.5534149045375,-17.1714240828892,
4.32059207806375));
#16930=CARTESIAN_POINT('Ctrl Pts',(-14.3455007806179,-17.0351933676591,
4.31157422775254));
#16931=CARTESIAN_POINT('Ctrl Pts',(-13.9890741217456,-16.6872392691384,
4.29059651917396));
#16932=CARTESIAN_POINT('Ctrl Pts',(-13.8455457084443,-16.4773475914728,
4.27950571726879));
#16933=CARTESIAN_POINT('Ctrl Pts',(-13.6521281424843,-16.0226193093072,
4.25804836699955));
#16934=CARTESIAN_POINT('Ctrl Pts',(-13.6006825475756,-15.7835100066402,
4.24786474810868));
#16935=CARTESIAN_POINT('Ctrl Pts',(-13.5899924845278,-15.2888905024329,
4.22889282827602));
#16936=CARTESIAN_POINT('Ctrl Pts',(-13.6347157041402,-15.0379852516787,
4.21862841815223));
#16937=CARTESIAN_POINT('Ctrl Pts',(-13.8180666535794,-14.571561386154,4.196948173568));
#16938=CARTESIAN_POINT('Ctrl Pts',(-13.9535367820056,-14.3601081049675,
4.18597446501882));
#16939=CARTESIAN_POINT('Ctrl Pts',(-14.2928560730081,-14.0066800250512,
4.16516355770824));
#16940=CARTESIAN_POINT('Ctrl Pts',(-14.491402872933,-13.8660108828828,4.15612060923297));
#16941=CARTESIAN_POINT('Ctrl Pts',(-14.9406933821584,-13.6615396576274,
4.13646660620472));
#16942=CARTESIAN_POINT('Ctrl Pts',(-15.1889677026202,-13.6036879578437,
4.125605962265));
#16943=CARTESIAN_POINT('Ctrl Pts',(-15.6870665518806,-13.5883237572087,
4.10381686124748));
#16944=CARTESIAN_POINT('Ctrl Pts',(-15.9320384291794,-13.6284081520162,
4.09310068113817));
#16945=CARTESIAN_POINT('Ctrl Pts',(-16.3918885303663,-13.7990130324649,
4.07298475370218));
#16946=CARTESIAN_POINT('Ctrl Pts',(-16.6026210354757,-13.9274064325583,
4.0641257857171));
#16947=CARTESIAN_POINT('Ctrl Pts',(-16.9700749212964,-14.2623619608257,
4.04339932292059));
#16948=CARTESIAN_POINT('Ctrl Pts',(-17.1210819760315,-14.4680350747609,
4.03230476172588));
#16949=CARTESIAN_POINT('Ctrl Pts',(-17.3300204514864,-14.9176282407073,
4.01070247210187));
#16950=CARTESIAN_POINT('Ctrl Pts',(-17.3893434322323,-15.15571156755,4.00038542487369));
#16951=CARTESIAN_POINT('Ctrl Pts',(-17.4041002263905,-15.4323602839601,
3.98958213469807));
#16952=CARTESIAN_POINT('Ctrl Pts',(-17.405,-15.4661957188126,3.98828063719431));
#16953=CARTESIAN_POINT('Ctrl Pts',(-17.405,-15.5,3.98699999999987));
#16954=CARTESIAN_POINT('Origin',(-15.5,-15.5,-1.713));
#16955=CARTESIAN_POINT('',(-17.405,-15.5,3.42449999999993));
#16956=CARTESIAN_POINT('',(-17.405,-15.4999999999999,3.48699999999987));
#16957=CARTESIAN_POINT('',(-17.405,-15.5,-1.713));
#16958=CARTESIAN_POINT('Ctrl Pts',(-17.405,-15.4999999999999,3.42449999999993));
#16959=CARTESIAN_POINT('Ctrl Pts',(-17.405,-15.4614919273425,3.42595883504683));
#16960=CARTESIAN_POINT('Ctrl Pts',(-17.4038324068547,-15.422945623307,3.42744465635428));
#16961=CARTESIAN_POINT('Ctrl Pts',(-17.3867253555674,-15.1415209695274,
3.43848028299768));
#16962=CARTESIAN_POINT('Ctrl Pts',(-17.3255583499887,-14.9037152031145,
3.44882714816257));
#16963=CARTESIAN_POINT('Ctrl Pts',(-17.1130008469439,-14.4554002870608,
3.47046016906023));
#16964=CARTESIAN_POINT('Ctrl Pts',(-16.9602578707828,-14.2507531198155,
3.48155383195293));
#16965=CARTESIAN_POINT('Ctrl Pts',(-16.5902498287586,-13.9188606573106,
3.50222011912992));
#16966=CARTESIAN_POINT('Ctrl Pts',(-16.3788495907395,-13.7922914531921,
3.51105513601302));
#16967=CARTESIAN_POINT('Ctrl Pts',(-15.917910107173,-13.6251789794874,3.53121871797131));
#16968=CARTESIAN_POINT('Ctrl Pts',(-15.6724556370897,-13.5869268055474,
3.5419560088761));
#16969=CARTESIAN_POINT('Ctrl Pts',(-15.1743158902438,-13.6061504385889,
3.56374689893934));
#16970=CARTESIAN_POINT('Ctrl Pts',(-14.9265037515429,-13.6659174378174,
3.57458732495425));
#16971=CARTESIAN_POINT('Ctrl Pts',(-14.4788704801155,-13.8738228385912,
3.59416883289068));
#16972=CARTESIAN_POINT('Ctrl Pts',(-14.2814591404654,-14.0159749912975,
3.60326496379597));
#16973=CARTESIAN_POINT('Ctrl Pts',(-13.9447558345002,-14.3720760147507,
3.62411991504735));
#16974=CARTESIAN_POINT('Ctrl Pts',(-13.8108291603664,-14.5847429374719,
3.63510584219906));
#16975=CARTESIAN_POINT('Ctrl Pts',(-13.6311050735004,-15.0528032762474,
3.65676875503005));
#16976=CARTESIAN_POINT('Ctrl Pts',(-13.5883709031569,-15.3040785387128,
3.66693274229893));
#16977=CARTESIAN_POINT('Ctrl Pts',(-13.6030062776106,-15.7988175390939,
3.6859954820102));
#16978=CARTESIAN_POINT('Ctrl Pts',(-13.6564327241794,-16.0376931449921,
3.69621357327602));
#16979=CARTESIAN_POINT('Ctrl Pts',(-13.8537624689396,-16.4911796393931,
3.71770944802686));
#16980=CARTESIAN_POINT('Ctrl Pts',(-13.9991810599468,-16.7000354706043,
3.72880235052296));
#16981=CARTESIAN_POINT('Ctrl Pts',(-14.358399335272,-17.0447335767602,3.74971776846828));
#16982=CARTESIAN_POINT('Ctrl Pts',(-14.5670178084669,-17.1789859548373,
3.75868713072889));
#16983=CARTESIAN_POINT('Ctrl Pts',(-15.0233682881308,-17.3606593439805,
3.77864996885944));
#16984=CARTESIAN_POINT('Ctrl Pts',(-15.2667228742052,-17.4065145378553,
3.78929540132114));
#16985=CARTESIAN_POINT('Ctrl Pts',(-15.7644940064487,-17.4033641976423,
3.81107016651116));
#16986=CARTESIAN_POINT('Ctrl Pts',(-16.0141322276006,-17.3516042446948,
3.82199047364817));
#16987=CARTESIAN_POINT('Ctrl Pts',(-16.4686139608441,-17.1580516102408,
3.84187156434124));
#16988=CARTESIAN_POINT('Ctrl Pts',(-16.6707818008129,-17.0220465010016,
3.85077996346433));
#16989=CARTESIAN_POINT('Ctrl Pts',(-17.0182773444189,-16.6770468578599,
3.8714504020934));
#16990=CARTESIAN_POINT('Ctrl Pts',(-17.158527732642,-16.4694767325026,3.88238155676259));
#16991=CARTESIAN_POINT('Ctrl Pts',(-17.3531512510743,-16.008436647136,3.90410439951443));
#16992=CARTESIAN_POINT('Ctrl Pts',(-17.4041360722943,-15.758785953557,3.91467728898608));
#16993=CARTESIAN_POINT('Ctrl Pts',(-17.4049963723817,-15.5042929847283,
3.92433728575485));
#16994=CARTESIAN_POINT('Ctrl Pts',(-17.4050000000196,-15.5021464040978,
3.92441868589383));
#16995=CARTESIAN_POINT('Ctrl Pts',(-17.405,-15.4999999826177,3.92450000065845));
#16996=CARTESIAN_POINT('Ctrl Pts',(-17.405,-15.5,3.98699999999987));
#16997=CARTESIAN_POINT('Ctrl Pts',(-17.405,-15.7183764833957,3.97872705239665));
#16998=CARTESIAN_POINT('Ctrl Pts',(-17.3674531932618,-15.9353913916047,
3.96968445279574));
#16999=CARTESIAN_POINT('Ctrl Pts',(-17.2097145334027,-16.3764419074438,
3.94952564785269));
#17000=CARTESIAN_POINT('Ctrl Pts',(-17.0803549969663,-16.5925903400615,
3.93850772126244));
#17001=CARTESIAN_POINT('Ctrl Pts',(-16.7513322330662,-16.9564719188534,
3.91752600327675));
#17002=CARTESIAN_POINT('Ctrl Pts',(-16.5571928795373,-17.1029549283145,
3.90824640767878));
#17003=CARTESIAN_POINT('Ctrl Pts',(-16.1144115409643,-17.3207811248282,
3.88887714527401));
#17004=CARTESIAN_POINT('Ctrl Pts',(-15.8680240062267,-17.3860756932498,
3.87809903789266));
#17005=CARTESIAN_POINT('Ctrl Pts',(-15.3699354945413,-17.4164903327027,
3.85631038908753));
#17006=CARTESIAN_POINT('Ctrl Pts',(-15.1231588456645,-17.3835747241081,
3.8455152600903));
#17007=CARTESIAN_POINT('Ctrl Pts',(-14.6591026105995,-17.2265810198167,
3.82521533729657));
#17008=CARTESIAN_POINT('Ctrl Pts',(-14.4457643415342,-17.1052342882286,
3.81642064056864));
#17009=CARTESIAN_POINT('Ctrl Pts',(-14.0684720259498,-16.7821838800442,
3.79593000111182));
#17010=CARTESIAN_POINT('Ctrl Pts',(-13.9107751972146,-16.5805645695418,
3.78484269318721));
#17011=CARTESIAN_POINT('Ctrl Pts',(-13.6878549632812,-16.1360821099788,
3.76312820418961));
#17012=CARTESIAN_POINT('Ctrl Pts',(-13.6213923552747,-15.8991527642048,
3.75269871441071));
#17013=CARTESIAN_POINT('Ctrl Pts',(-13.5809017461053,-15.4067401086061,
3.73315859308621));
#17014=CARTESIAN_POINT('Ctrl Pts',(-13.6097237057755,-15.155749122147,3.7236364016455));
#17015=CARTESIAN_POINT('Ctrl Pts',(-13.7627857675895,-14.6791704166862,
3.702233938971));
#17016=CARTESIAN_POINT('Ctrl Pts',(-13.8855451897592,-14.4582664818264,
3.69118021497846));
#17017=CARTESIAN_POINT('Ctrl Pts',(-14.2036046789724,-14.0834550905506,
3.67002422499248));
#17018=CARTESIAN_POINT('Ctrl Pts',(-14.3932240200836,-13.9308436246418,
3.66041539719665));
#17019=CARTESIAN_POINT('Ctrl Pts',(-14.8291239419257,-13.6992634410876,
3.64134715914579));
#17020=CARTESIAN_POINT('Ctrl Pts',(-15.0733167129576,-13.6263288506664,
3.63066506067544));
#17021=CARTESIAN_POINT('Ctrl Pts',(-15.57091270054,-13.5803148558224,3.60889795710666));
#17022=CARTESIAN_POINT('Ctrl Pts',(-15.8193408380043,-13.6057324145129,
3.59803058451417));
#17023=CARTESIAN_POINT('Ctrl Pts',(-16.2876421974074,-13.7486242565046,
3.57754496074325));
#17024=CARTESIAN_POINT('Ctrl Pts',(-16.5036951881227,-13.8628408826526,
3.56873551144344));
#17025=CARTESIAN_POINT('Ctrl Pts',(-16.8908612944749,-14.1736570247294,
3.54849239122817));
#17026=CARTESIAN_POINT('Ctrl Pts',(-17.0552700892148,-14.3709294205846,
3.53742295537314));
#17027=CARTESIAN_POINT('Ctrl Pts',(-17.292316215799,-14.8097683997458,3.51561329800583));
#17028=CARTESIAN_POINT('Ctrl Pts',(-17.3660349623944,-15.0453043822237,
3.50507788603606));
#17029=CARTESIAN_POINT('Ctrl Pts',(-17.4010777344063,-15.3587618909951,
3.49243643583445));
#17030=CARTESIAN_POINT('Ctrl Pts',(-17.405,-15.4294197625975,3.48967385295681));
#17031=CARTESIAN_POINT('Ctrl Pts',(-17.405,-15.4999999999999,3.48699999999987));
#17032=CARTESIAN_POINT('Origin',(-15.5,-15.5,-1.713));
#17033=CARTESIAN_POINT('',(-17.405,-15.4999999999999,2.92449999999993));
#17034=CARTESIAN_POINT('',(-17.405,-15.5,2.98699999999986));
#17035=CARTESIAN_POINT('',(-17.405,-15.5,-1.713));
#17036=CARTESIAN_POINT('Ctrl Pts',(-17.405,-15.4999999999999,2.92449999999993));
#17037=CARTESIAN_POINT('Ctrl Pts',(-17.405,-15.4246029704291,2.92735633171377));
#17038=CARTESIAN_POINT('Ctrl Pts',(-17.4005241425492,-15.3491261289197,
2.93031358415772));
#17039=CARTESIAN_POINT('Ctrl Pts',(-17.3625026971922,-15.030949658235,2.94319895726262));
#17040=CARTESIAN_POINT('Ctrl Pts',(-17.2869039689406,-14.7958112749887,
2.95376042609122));
#17041=CARTESIAN_POINT('Ctrl Pts',(-17.0462119101931,-14.3585090291066,
2.97559161084361));
#17042=CARTESIAN_POINT('Ctrl Pts',(-16.8800785444847,-14.1624005620978,
2.98665467283752));
#17043=CARTESIAN_POINT('Ctrl Pts',(-16.4903722843864,-13.8547788324716,
3.00683233524616));
#17044=CARTESIAN_POINT('Ctrl Pts',(-16.2736016230491,-13.7424065889116,
3.01565915909658));
#17045=CARTESIAN_POINT('Ctrl Pts',(-15.8042055235872,-13.6032175602641,
3.03619267175896));
#17046=CARTESIAN_POINT('Ctrl Pts',(-15.5553810743812,-13.5797787576298,
3.04707738082309));
#17047=CARTESIAN_POINT('Ctrl Pts',(-15.0579955564868,-13.6298855017054,
3.06883527749388));
#17048=CARTESIAN_POINT('Ctrl Pts',(-14.8144188605694,-13.7048120123677,
3.07949042604668));
#17049=CARTESIAN_POINT('Ctrl Pts',(-14.3803478613073,-13.9399897068444,
3.09847865873529));
#17050=CARTESIAN_POINT('Ctrl Pts',(-14.1919085752892,-14.0942297674633,
3.10818823180623));
#17051=CARTESIAN_POINT('Ctrl Pts',(-13.8767794458615,-14.4719269225963,
3.12938945210352));
#17052=CARTESIAN_POINT('Ctrl Pts',(-13.7557980800781,-14.6940588916751,
3.14045080866986));
#17053=CARTESIAN_POINT('Ctrl Pts',(-13.6069962562461,-15.1715532833019,
3.16179478002723));
#17054=CARTESIAN_POINT('Ctrl Pts',(-13.5802964278705,-15.4221320121638,
3.17122845836935));
#17055=CARTESIAN_POINT('Ctrl Pts',(-13.6245367961492,-15.913784746089,3.190821806644));
#17056=CARTESIAN_POINT('Ctrl Pts',(-13.6929081588293,-16.1503692156979,
3.20127997996693));
#17057=CARTESIAN_POINT('Ctrl Pts',(-13.9195525061294,-16.5934112583634,
3.22302135518752));
#17058=CARTESIAN_POINT('Ctrl Pts',(-14.0790234790521,-16.7939093902312,
3.23410499307334));
#17059=CARTESIAN_POINT('Ctrl Pts',(-14.4589246323286,-17.1137556039747,
3.25453130641737));
#17060=CARTESIAN_POINT('Ctrl Pts',(-14.6729691488013,-17.2332242138591,
3.26332192251953));
#17061=CARTESIAN_POINT('Ctrl Pts',(-15.1381451842514,-17.3865362903766,
3.28367083045699));
#17062=CARTESIAN_POINT('Ctrl Pts',(-15.3853746064769,-17.4175006398182,
3.29448576581245));
#17063=CARTESIAN_POINT('Ctrl Pts',(-15.8833818147483,-17.3830125865093,
3.3162708580378));
#17064=CARTESIAN_POINT('Ctrl Pts',(-16.1292196923062,-17.3157156943741,
3.32702492092311));
#17065=CARTESIAN_POINT('Ctrl Pts',(-16.570217563795,-17.0942905219578,3.34631616639506));
#17066=CARTESIAN_POINT('Ctrl Pts',(-16.7631725989519,-16.9462183677401,
3.35567342316665));
#17067=CARTESIAN_POINT('Ctrl Pts',(-17.0893626738479,-16.5794927492161,
3.37670092707341));
#17068=CARTESIAN_POINT('Ctrl Pts',(-17.2170253917602,-16.3620913328898,
3.38772920827698));
#17069=CARTESIAN_POINT('Ctrl Pts',(-17.3693031954026,-15.9246324502421,
3.40763250693426));
#17070=CARTESIAN_POINT('Ctrl Pts',(-17.405,-15.7129299879628,3.41643338675393));
#17071=CARTESIAN_POINT('Ctrl Pts',(-17.405,-15.4999999999999,3.42449999999993));
#17072=CARTESIAN_POINT('Ctrl Pts',(-17.405,-15.4999999999999,3.48699999999987));
#17073=CARTESIAN_POINT('Ctrl Pts',(-17.405,-15.6764531477386,3.4803152708433));
#17074=CARTESIAN_POINT('Ctrl Pts',(-17.3804873179637,-15.8523801803092,
3.47311432506748));
#17075=CARTESIAN_POINT('Ctrl Pts',(-17.2629771594338,-16.2641939190073,
3.45494301104277));
#17076=CARTESIAN_POINT('Ctrl Pts',(-17.147005924465,-16.4896706537741,3.4438645247018));
#17077=CARTESIAN_POINT('Ctrl Pts',(-16.8400905328106,-16.8753750105602,
3.42253961362769));
#17078=CARTESIAN_POINT('Ctrl Pts',(-16.6549001286324,-17.0341609160333,
3.41252056555695));
#17079=CARTESIAN_POINT('Ctrl Pts',(-16.2259290516944,-17.2792504677336,
3.39375542658327));
#17080=CARTESIAN_POINT('Ctrl Pts',(-15.9841393868079,-17.3596471123229,
3.38317845086646));
#17081=CARTESIAN_POINT('Ctrl Pts',(-15.4875102619216,-17.4210491324768,
3.36145364225377));
#17082=CARTESIAN_POINT('Ctrl Pts',(-15.2376720328314,-17.4030964029156,
3.35052458586313));
#17083=CARTESIAN_POINT('Ctrl Pts',(-14.7652944961111,-17.2741400167745,
3.3298606516234));
#17084=CARTESIAN_POINT('Ctrl Pts',(-14.546527920475,-17.1668079458835,3.32095721717422));
#17085=CARTESIAN_POINT('Ctrl Pts',(-14.1499117418974,-16.8679726763458,
3.30096128435465));
#17086=CARTESIAN_POINT('Ctrl Pts',(-13.9790956107818,-16.6751252050885,
3.28991933882874));
#17087=CARTESIAN_POINT('Ctrl Pts',(-13.7284685714235,-16.2421809384311,
3.26803595068229));
#17088=CARTESIAN_POINT('Ctrl Pts',(-13.6477317959478,-16.0082067494623,
3.25740620530981));
#17089=CARTESIAN_POINT('Ctrl Pts',(-13.5792898836175,-15.5216378862272,
3.23747611115332));
#17090=CARTESIAN_POINT('Ctrl Pts',(-13.5925554052722,-15.2736030156638,
3.22847667356028));
#17091=CARTESIAN_POINT('Ctrl Pts',(-13.7141357063192,-14.7906605136231,
3.2075217030503));
#17092=CARTESIAN_POINT('Ctrl Pts',(-13.8234698343903,-14.5610040823231,
3.19643004217174));
#17093=CARTESIAN_POINT('Ctrl Pts',(-14.1194602955704,-14.1651196850214,
3.17495842469075));
#17094=CARTESIAN_POINT('Ctrl Pts',(-14.3003771223459,-14.0004255695162,
3.16476211229926));
#17095=CARTESIAN_POINT('Ctrl Pts',(-14.7227040856981,-13.7425835691326,
3.14575681027953));
#17096=CARTESIAN_POINT('Ctrl Pts',(-14.9621109288452,-13.6551633959072,
3.13552970564974));
#17097=CARTESIAN_POINT('Ctrl Pts',(-15.4575797798197,-13.5792882748642,
3.11385565267621));
#17098=CARTESIAN_POINT('Ctrl Pts',(-15.7085427300214,-13.5901710364673,
3.10287739588699));
#17099=CARTESIAN_POINT('Ctrl Pts',(-16.1846495764087,-13.7059977045008,
3.08205032474143));
#17100=CARTESIAN_POINT('Ctrl Pts',(-16.4060079774435,-13.8069773445162,
3.07298847944479));
#17101=CARTESIAN_POINT('Ctrl Pts',(-16.8085181321564,-14.0926836357192,
3.05336100859792));
#17102=CARTESIAN_POINT('Ctrl Pts',(-16.9832809666978,-14.2782731379037,
3.04250769972486));
#17103=CARTESIAN_POINT('Ctrl Pts',(-17.2468705889534,-14.7012659478552,
3.02071779026886));
#17104=CARTESIAN_POINT('Ctrl Pts',(-17.3353128781264,-14.9332790215386,
3.00999380249955));
#17105=CARTESIAN_POINT('Ctrl Pts',(-17.3957395224265,-15.2830534969887,
2.99542132203213));
#17106=CARTESIAN_POINT('Ctrl Pts',(-17.405,-15.3915468179105,2.99110862689446));
#17107=CARTESIAN_POINT('Ctrl Pts',(-17.405,-15.5,2.98699999999986));
#17108=CARTESIAN_POINT('Origin',(-15.5,-15.5,-1.713));
#17109=CARTESIAN_POINT('',(-17.405,-15.5,2.42449999999992));
#17110=CARTESIAN_POINT('',(-17.405,-15.5,2.48699999999985));
#17111=CARTESIAN_POINT('',(-17.405,-15.5,-1.713));
#17112=CARTESIAN_POINT('Ctrl Pts',(-17.405,-15.5,2.42449999999992));
#17113=CARTESIAN_POINT('Ctrl Pts',(-17.405,-15.3866287216877,2.42879494344165));
#17114=CARTESIAN_POINT('Ctrl Pts',(-17.3948806441803,-15.2732338375239,
2.43331211440638));
#17115=CARTESIAN_POINT('Ctrl Pts',(-17.330832577681,-14.9188879456016,2.44813698655778));
#17116=CARTESIAN_POINT('Ctrl Pts',(-17.2404900805375,-14.6873986588248,
2.45888269310303));
#17117=CARTESIAN_POINT('Ctrl Pts',(-16.973408577859,-14.2663867214871,2.48067393476401));
#17118=CARTESIAN_POINT('Ctrl Pts',(-16.7971653949025,-14.0822139660179,
2.49150595035454));
#17119=CARTESIAN_POINT('Ctrl Pts',(-16.3924276582491,-13.799788061525,2.51105786970293));
#17120=CARTESIAN_POINT('Ctrl Pts',(-16.1703213448218,-13.7006022327362,
2.52017710652558));
#17121=CARTESIAN_POINT('Ctrl Pts',(-15.6931687253924,-13.5885289569252,
2.54104992452337));
#17122=CARTESIAN_POINT('Ctrl Pts',(-15.4419207498431,-13.5796720432962,
2.55204064961302));
#17123=CARTESIAN_POINT('Ctrl Pts',(-14.9448705760937,-13.6599948516569,
2.57378387681115));
#17124=CARTESIAN_POINT('Ctrl Pts',(-14.7043542991087,-13.7505153330003,
2.58395864765043));
#17125=CARTESIAN_POINT('Ctrl Pts',(-14.2830278447516,-14.0144258842274,
2.60317196649853));
#17126=CARTESIAN_POINT('Ctrl Pts',(-14.1038402602375,-14.1814147098486,
2.61341738895667));
#17127=CARTESIAN_POINT('Ctrl Pts',(-13.8122359953876,-14.5812645112853,
2.63494329526319));
#17128=CARTESIAN_POINT('Ctrl Pts',(-13.7055635984876,-14.8125202663001,
2.64603732663082));
#17129=CARTESIAN_POINT('Ctrl Pts',(-13.5900531890772,-15.2965866386149,
2.66690211141856));
#17130=CARTESIAN_POINT('Ctrl Pts',(-13.5797585477662,-15.5440797481913,
2.67583654661438));
#17131=CARTESIAN_POINT('Ctrl Pts',(-13.6536576949259,-16.0294590950737,
2.69584093937257));
#17132=CARTESIAN_POINT('Ctrl Pts',(-13.7371892876536,-16.2627520080675,
2.70650600435679));
#17133=CARTESIAN_POINT('Ctrl Pts',(-13.9917092405621,-16.6907175631168,
2.7282859264509));
#17134=CARTESIAN_POINT('Ctrl Pts',(-14.1626016047602,-16.8799033597708,
2.73919082094069));
#17135=CARTESIAN_POINT('Ctrl Pts',(-14.5593214870997,-17.1740429974242,
2.7590111332608));
#17136=CARTESIAN_POINT('Ctrl Pts',(-14.7787835918848,-17.2796492651576,
2.76795072580402));
#17137=CARTESIAN_POINT('Ctrl Pts',(-15.252177850505,-17.4050640088115,2.78865913606738));
#17138=CARTESIAN_POINT('Ctrl Pts',(-15.5023389993631,-17.4211126319878,
2.79960231843214));
#17139=CARTESIAN_POINT('Ctrl Pts',(-15.9987461698247,-17.3557948735195,
2.82131741775242));
#17140=CARTESIAN_POINT('Ctrl Pts',(-16.2398924930437,-17.2734770843301,
2.83183027289843));
#17141=CARTESIAN_POINT('Ctrl Pts',(-16.6670901386329,-17.0249503089065,
2.85058921094883));
#17142=CARTESIAN_POINT('Ctrl Pts',(-16.8511310705029,-16.8645487287507,
2.86069123672124));
#17143=CARTESIAN_POINT('Ctrl Pts',(-17.1551013135425,-16.4761253349775,
2.88205473838143));
#17144=CARTESIAN_POINT('Ctrl Pts',(-17.2693013185321,-16.2495057733069,
2.89313777862186));
#17145=CARTESIAN_POINT('Ctrl Pts',(-17.3819592475714,-15.8416977694031,
2.91105121063268));
#17146=CARTESIAN_POINT('Ctrl Pts',(-17.405,-15.6710735741344,2.91801906994232));
#17147=CARTESIAN_POINT('Ctrl Pts',(-17.405,-15.4999999999999,2.92449999999993));
#17148=CARTESIAN_POINT('Ctrl Pts',(-17.405,-15.5,2.98699999999986));
#17149=CARTESIAN_POINT('Ctrl Pts',(-17.405,-15.6348413314497,2.98189168772884));
#17150=CARTESIAN_POINT('Ctrl Pts',(-17.3906852736361,-15.7695966035171,
2.97647354021857));
#17151=CARTESIAN_POINT('Ctrl Pts',(-17.3087652033694,-16.1490564386062,
2.96030635334035));
#17152=CARTESIAN_POINT('Ctrl Pts',(-17.2067942988799,-16.3830339576779,
2.94921204329331));
#17153=CARTESIAN_POINT('Ctrl Pts',(-16.922972583008,-16.7896948145866,2.92759832978747));
#17154=CARTESIAN_POINT('Ctrl Pts',(-16.7468731843496,-16.9606478650304,
2.91727027275038));
#17155=CARTESIAN_POINT('Ctrl Pts',(-16.3321205610298,-17.2321519637799,
2.89791306547092));
#17156=CARTESIAN_POINT('Ctrl Pts',(-16.0954586961872,-17.3270829461848,
2.88804806195041));
#17157=CARTESIAN_POINT('Ctrl Pts',(-15.6017485836216,-17.418582659013,2.86645094416539));
#17158=CARTESIAN_POINT('Ctrl Pts',(-15.3497898078031,-17.4153981809549,
2.85542912545068));
#17159=CARTESIAN_POINT('Ctrl Pts',(-14.8697620227219,-17.3138206140289,
2.83443053467723));
#17160=CARTESIAN_POINT('Ctrl Pts',(-14.6455467021456,-17.2196022923227,
2.82512303677297));
#17161=CARTESIAN_POINT('Ctrl Pts',(-14.2346929933562,-16.9462855801242,
2.80578243876608));
#17162=CARTESIAN_POINT('Ctrl Pts',(-14.0544139525623,-16.7660972674064,
2.79501309595437));
#17163=CARTESIAN_POINT('Ctrl Pts',(-13.7777445899928,-16.3507193868928,
2.7732255859815));
#17164=CARTESIAN_POINT('Ctrl Pts',(-13.6821563903077,-16.1207596787417,
2.76242309040195));
#17165=CARTESIAN_POINT('Ctrl Pts',(-13.5847088675459,-15.6406980901775,
2.74210509860585));
#17166=CARTESIAN_POINT('Ctrl Pts',(-13.5823994058797,-15.3953897232232,
2.73331256079938));
#17167=CARTESIAN_POINT('Ctrl Pts',(-13.6720198072411,-14.9068760737457,
2.71284556905731));
#17168=CARTESIAN_POINT('Ctrl Pts',(-13.7670951492794,-14.6691356899221,
2.70175952868478));
#17169=CARTESIAN_POINT('Ctrl Pts',(-14.0394246976334,-14.2529140471301,
2.6800349752972));
#17170=CARTESIAN_POINT('Ctrl Pts',(-14.2109198649204,-14.0763443783639,
2.66959484396155));
#17171=CARTESIAN_POINT('Ctrl Pts',(-14.6161830495051,-13.7940142570894,
2.65003506051579));
#17172=CARTESIAN_POINT('Ctrl Pts',(-14.847434530759,-13.6928766622502,2.64054617100783));
#17173=CARTESIAN_POINT('Ctrl Pts',(-15.3362030982655,-13.5856111981726,
2.61916521879844));
#17174=CARTESIAN_POINT('Ctrl Pts',(-15.5889576943258,-13.5806775350222,
2.60810858729974));
#17175=CARTESIAN_POINT('Ctrl Pts',(-16.072966293995,-13.6672512129721,2.58693585765542));
#17176=CARTESIAN_POINT('Ctrl Pts',(-16.30024349174,-13.7544824009695,2.57729050033427));
#17177=CARTESIAN_POINT('Ctrl Pts',(-16.719562151595,-14.0149434292219,2.5582517778019));
#17178=CARTESIAN_POINT('Ctrl Pts',(-16.9053469084664,-14.18938943058,2.54757955351491));
#17179=CARTESIAN_POINT('Ctrl Pts',(-17.1952671189457,-14.5964930079793,
2.52581568014487));
#17180=CARTESIAN_POINT('Ctrl Pts',(-17.2981758603756,-14.8241099078218,
2.51494182238855));
#17181=CARTESIAN_POINT('Ctrl Pts',(-17.3881884443977,-15.2079235803331,
2.4984326936604));
#17182=CARTESIAN_POINT('Ctrl Pts',(-17.405,-15.3538704367668,2.49253595424323));
#17183=CARTESIAN_POINT('Ctrl Pts',(-17.405,-15.5,2.48699999999985));
#17184=CARTESIAN_POINT('Origin',(-15.5,-15.5,-1.713));
#17185=CARTESIAN_POINT('',(-17.405,-15.5,1.92449999999991));
#17186=CARTESIAN_POINT('',(-17.405,-15.5000000000001,1.98699999999984));
#17187=CARTESIAN_POINT('',(-17.405,-15.5,-1.713));
#17188=CARTESIAN_POINT('Ctrl Pts',(-17.405,-15.5,1.92449999999991));
#17189=CARTESIAN_POINT('Ctrl Pts',(-17.405,-15.3486986793144,1.93023188046098));
#17190=CARTESIAN_POINT('Ctrl Pts',(-17.3869774740474,-15.1976302972843,
1.93634912978389));
#17191=CARTESIAN_POINT('Ctrl Pts',(-17.2925795312766,-14.8093323449348,
1.95312405814599));
#17192=CARTESIAN_POINT('Ctrl Pts',(-17.1877032252396,-14.582387157065,1.96401550394565));
#17193=CARTESIAN_POINT('Ctrl Pts',(-16.8942477032967,-14.1775904447064,
1.9857693095993));
#17194=CARTESIAN_POINT('Ctrl Pts',(-16.7070086756833,-14.0047243622716,
1.99641348863026));
#17195=CARTESIAN_POINT('Ctrl Pts',(-16.2854263826576,-13.7477497935979,
2.01536964134727));
#17196=CARTESIAN_POINT('Ctrl Pts',(-16.0573006855409,-13.6624109872575,
2.02512114236464));
#17197=CARTESIAN_POINT('Ctrl Pts',(-15.5722291432103,-13.579946666267,2.04634036993816));
#17198=CARTESIAN_POINT('Ctrl Pts',(-15.3193016253507,-13.5871036514588,
2.05740456582003));
#17199=CARTESIAN_POINT('Ctrl Pts',(-14.8319183237239,-13.6986435441608,
2.07872492022189));
#17200=CARTESIAN_POINT('Ctrl Pts',(-14.6021272930825,-13.8014628299617,
2.08812467256909));
#17201=CARTESIAN_POINT('Ctrl Pts',(-14.1994820415506,-14.0867521555902,
2.10773930201741));
#17202=CARTESIAN_POINT('Ctrl Pts',(-14.029286629017,-14.2648482619827,2.11820883214505));
#17203=CARTESIAN_POINT('Ctrl Pts',(-13.7601789517598,-14.6836493550942,
2.13996063548694));
#17204=CARTESIAN_POINT('Ctrl Pts',(-13.6670272894183,-14.9223925914719,
2.15104259256723));
#17205=CARTESIAN_POINT('Ctrl Pts',(-13.5816226349698,-15.4115802655974,
2.17144291103771));
#17206=CARTESIAN_POINT('Ctrl Pts',(-13.5859774200922,-15.6565526410676,
2.18023347656324));
#17207=CARTESIAN_POINT('Ctrl Pts',(-13.6873032473563,-16.1357098037595,
2.20060203250936));
#17208=CARTESIAN_POINT('Ctrl Pts',(-13.7848735554849,-16.3650593087161,
2.21142476442983));
#17209=CARTESIAN_POINT('Ctrl Pts',(-14.0651457198649,-16.7782445247767,
2.23320800921402));
#17210=CARTESIAN_POINT('Ctrl Pts',(-14.2469301421843,-16.9568990841518,
2.24395217360948));
#17211=CARTESIAN_POINT('Ctrl Pts',(-14.6600831874615,-17.2267522515104,
2.26321185081259));
#17212=CARTESIAN_POINT('Ctrl Pts',(-14.8851133202991,-17.319086036431,2.27260207000412));
#17213=CARTESIAN_POINT('Ctrl Pts',(-15.3662227564387,-17.4166438315601,
2.29364797709685));
#17214=CARTESIAN_POINT('Ctrl Pts',(-15.6184201448337,-17.4176538394308,
2.30468023380706));
#17215=CARTESIAN_POINT('Ctrl Pts',(-16.1108249144034,-17.3219057393829,
2.32622024997372));
#17216=CARTESIAN_POINT('Ctrl Pts',(-16.3460254825939,-17.2253010985772,
2.33597673494084));
#17217=CARTESIAN_POINT('Ctrl Pts',(-16.7582463484608,-16.9508932005934,
2.35538857411786));
#17218=CARTESIAN_POINT('Ctrl Pts',(-16.9331340337932,-16.7784291356177,
2.36574737132588));
#17219=CARTESIAN_POINT('Ctrl Pts',(-17.2139188972246,-16.3691856695095,
2.38739250123395));
#17220=CARTESIAN_POINT('Ctrl Pts',(-17.3140623235137,-16.1341848427474,
2.39848560705332));
#17221=CARTESIAN_POINT('Ctrl Pts',(-17.3917862251892,-15.759050717556,2.41439713955902));
#17222=CARTESIAN_POINT('Ctrl Pts',(-17.405,-15.6295518546112,2.41959207361318));
#17223=CARTESIAN_POINT('Ctrl Pts',(-17.405,-15.5,2.42449999999992));
#17224=CARTESIAN_POINT('Ctrl Pts',(-17.405,-15.5,2.48699999999985));
#17225=CARTESIAN_POINT('Ctrl Pts',(-17.405,-15.5949683349577,2.48340223138093));
#17226=CARTESIAN_POINT('Ctrl Pts',(-17.3978991014891,-15.6900019365671,
2.47964667746751));
#17227=CARTESIAN_POINT('Ctrl Pts',(-17.3457037805944,-16.035815620742,2.46540428482014));
#17228=CARTESIAN_POINT('Ctrl Pts',(-17.2577563440206,-16.277172943574,2.45433712422308));
#17229=CARTESIAN_POINT('Ctrl Pts',(-16.9973983370484,-16.7027671265982,
2.43251934742135));
#17230=CARTESIAN_POINT('Ctrl Pts',(-16.8307514409228,-16.8849073795883,
2.42197422344043));
#17231=CARTESIAN_POINT('Ctrl Pts',(-16.4351306847412,-17.1780794189316,
2.40221460787432));
#17232=CARTESIAN_POINT('Ctrl Pts',(-16.2091894631102,-17.2853513335075,
2.3930231611159));
#17233=CARTESIAN_POINT('Ctrl Pts',(-15.7255640317756,-17.4082035102829,
2.37186719299102));
#17234=CARTESIAN_POINT('Ctrl Pts',(-15.4722692826481,-17.4212876437741,
2.36078693274924));
#17235=CARTESIAN_POINT('Ctrl Pts',(-14.9844212984852,-17.3497866434107,
2.33944625102733));
#17236=CARTESIAN_POINT('Ctrl Pts',(-14.7540109523672,-17.2694561740815,
2.32938405397293));
#17237=CARTESIAN_POINT('Ctrl Pts',(-14.3265001644784,-17.0217099393331,
2.31064783669698));
#17238=CARTESIAN_POINT('Ctrl Pts',(-14.1354929276868,-16.853069236674,2.30008131215583));
#17239=CARTESIAN_POINT('Ctrl Pts',(-13.8328034235953,-16.4545030489022,
2.27836157480911));
#17240=CARTESIAN_POINT('Ctrl Pts',(-13.7227580108401,-16.2294088619722,
2.26742719202244));
#17241=CARTESIAN_POINT('Ctrl Pts',(-13.5969187251782,-15.7561699905676,
2.24674667900731));
#17242=CARTESIAN_POINT('Ctrl Pts',(-13.5798018576392,-15.5131442345915,
2.23783037236436));
#17243=CARTESIAN_POINT('Ctrl Pts',(-13.6385605200307,-15.0227027697103,
2.21796536366566));
#17244=CARTESIAN_POINT('Ctrl Pts',(-13.7181303906783,-14.7804916560613,
2.2070490945133));
#17245=CARTESIAN_POINT('Ctrl Pts',(-13.9635498436067,-14.3473695137498,
2.18527286946309));
#17246=CARTESIAN_POINT('Ctrl Pts',(-14.1246435540447,-14.1592368872228,
2.17462219190088));
#17247=CARTESIAN_POINT('Ctrl Pts',(-14.5095940750912,-13.8542486731349,
2.15464831605754));
#17248=CARTESIAN_POINT('Ctrl Pts',(-14.7298789167439,-13.7403639765452,
2.14568858631908));
#17249=CARTESIAN_POINT('Ctrl Pts',(-15.2076990152618,-13.6007564602427,
2.12478656976098));
#17250=CARTESIAN_POINT('Ctrl Pts',(-15.4612907383838,-13.5787868978837,
2.1136933185308));
#17251=CARTESIAN_POINT('Ctrl Pts',(-15.9528706723896,-13.6337786144342,
2.0921893844098));
#17252=CARTESIAN_POINT('Ctrl Pts',(-16.1866229664858,-13.706554770831,2.08196399971618));
#17253=CARTESIAN_POINT('Ctrl Pts',(-16.6250552312494,-13.9417184916321,
2.06278498550955));
#17254=CARTESIAN_POINT('Ctrl Pts',(-16.8232548833612,-14.1060742689683,
2.05253139336743));
#17255=CARTESIAN_POINT('Ctrl Pts',(-17.1394238328743,-14.4983732171102,
2.03075425733394));
#17256=CARTESIAN_POINT('Ctrl Pts',(-17.2561233330502,-14.7208972749967,
2.01977170102725));
#17257=CARTESIAN_POINT('Ctrl Pts',(-17.3787284650258,-15.1353123617131,
2.00139039924266));
#17258=CARTESIAN_POINT('Ctrl Pts',(-17.405,-15.3173263053678,1.99392038758316));
#17259=CARTESIAN_POINT('Ctrl Pts',(-17.405,-15.5000000000001,1.98699999999984));
#17260=CARTESIAN_POINT('Origin',(-15.5,-15.5,-1.713));
#17261=CARTESIAN_POINT('',(-17.405,-15.5000000000001,1.4244999999999));
#17262=CARTESIAN_POINT('',(-17.405,-15.5,1.48699999999984));
#17263=CARTESIAN_POINT('',(-17.405,-15.5,-1.713));
#17264=CARTESIAN_POINT('Ctrl Pts',(-17.405,-15.5000000000001,1.42449999999991));
#17265=CARTESIAN_POINT('Ctrl Pts',(-17.405,-15.3118633378577,1.4316273459666));
#17266=CARTESIAN_POINT('Ctrl Pts',(-17.3771334387433,-15.1244839044587,
1.43933551001286));
#17267=CARTESIAN_POINT('Ctrl Pts',(-17.24934219222,-14.7057213235397,1.45799494380515));
#17268=CARTESIAN_POINT('Ctrl Pts',(-17.1306051942564,-14.4840272327072,
1.46899062243645));
#17269=CARTESIAN_POINT('Ctrl Pts',(-16.8113229405752,-14.0949843783885,
1.49071250003231));
#17270=CARTESIAN_POINT('Ctrl Pts',(-16.6123900156071,-13.9327769674847,
1.5008390194396));
#17271=CARTESIAN_POINT('Ctrl Pts',(-16.1726839958291,-13.7012553587294,
1.52007375346314));
#17272=CARTESIAN_POINT('Ctrl Pts',(-15.9381891396067,-13.6302529558287,
1.53033162118941));
#17273=CARTESIAN_POINT('Ctrl Pts',(-15.4457978890103,-13.5791344218338,
1.5518710459749));
#17274=CARTESIAN_POINT('Ctrl Pts',(-15.1921803263023,-13.603182159575,1.56296542754568));
#17275=CARTESIAN_POINT('Ctrl Pts',(-14.7157470931694,-13.7466772505015,
1.58380677632663));
#17276=CARTESIAN_POINT('Ctrl Pts',(-14.4967660670359,-13.8621014312398,
1.59272638657522));
#17277=CARTESIAN_POINT('Ctrl Pts',(-14.114338281745,-14.1698558360362,1.61274987849671));
#17278=CARTESIAN_POINT('Ctrl Pts',(-13.954584909938,-14.3593774914536,1.62342386161404));
#17279=CARTESIAN_POINT('Ctrl Pts',(-13.7125069078124,-14.7945807372207,
1.64520584182867));
#17280=CARTESIAN_POINT('Ctrl Pts',(-13.634853063525,-15.0374057231972,1.65610345900596));
#17281=CARTESIAN_POINT('Ctrl Pts',(-13.5799789460238,-15.5281670839837,
1.67589562280244));
#17282=CARTESIAN_POINT('Ctrl Pts',(-13.5989789668469,-15.7709288370138,
1.68485086346852));
#17283=CARTESIAN_POINT('Ctrl Pts',(-13.7284765422896,-16.243253711504,1.705576765825));
#17284=CARTESIAN_POINT('Ctrl Pts',(-13.8403731054317,-16.4676542695703,
1.71652536011545));
#17285=CARTESIAN_POINT('Ctrl Pts',(-14.1464186600125,-16.8640172845373,
1.73823503716585));
#17286=CARTESIAN_POINT('Ctrl Pts',(-14.3388048877782,-17.0311085657265,
1.74870406333214));
#17287=CARTESIAN_POINT('Ctrl Pts',(-14.768468555141,-17.27551976469,1.76749949934977));
#17288=CARTESIAN_POINT('Ctrl Pts',(-14.9997221812654,-17.3539974482555,
1.77761558098252));
#17289=CARTESIAN_POINT('Ctrl Pts',(-15.4884672042666,-17.4214811002394,
1.79899550324855));
#17290=CARTESIAN_POINT('Ctrl Pts',(-15.7418621364513,-17.4062346806301,
1.8100801459513));
#17291=CARTESIAN_POINT('Ctrl Pts',(-16.2240935842588,-17.2792838313506,
1.83117513491927));
#17292=CARTESIAN_POINT('Ctrl Pts',(-16.4486458433526,-17.1703969211375,
1.84030125781118));
#17293=CARTESIAN_POINT('Ctrl Pts',(-16.8416862876065,-16.8743501327491,
1.8601133427447));
#17294=CARTESIAN_POINT('Ctrl Pts',(-17.0070079317082,-16.6907437705779,
1.87068502235921));
#17295=CARTESIAN_POINT('Ctrl Pts',(-17.2641149130594,-16.2627020426674,
1.89252441435073));
#17296=CARTESIAN_POINT('Ctrl Pts',(-17.3501358504591,-16.0204129092833,
1.90358473864083));
#17297=CARTESIAN_POINT('Ctrl Pts',(-17.3986777732664,-15.6792907617315,
1.91756948960221));
#17298=CARTESIAN_POINT('Ctrl Pts',(-17.405,-15.589609821744,1.92110523263075));
#17299=CARTESIAN_POINT('Ctrl Pts',(-17.405,-15.5,1.92449999999991));
#17300=CARTESIAN_POINT('Ctrl Pts',(-17.405,-15.5000000000001,1.98699999999985));
#17301=CARTESIAN_POINT('Ctrl Pts',(-17.405,-15.5576762506347,1.98481500007663));
#17302=CARTESIAN_POINT('Ctrl Pts',(-17.4023807755921,-15.6154139218634,
1.98257038493044));
#17303=CARTESIAN_POINT('Ctrl Pts',(-17.3741939527039,-15.9244464994239,
1.97024652341651));
#17304=CARTESIAN_POINT('Ctrl Pts',(-17.3015165680925,-16.1687866178387,
1.95940035359952));
#17305=CARTESIAN_POINT('Ctrl Pts',(-17.0681604473867,-16.6092508752271,
1.93760983318351));
#17306=CARTESIAN_POINT('Ctrl Pts',(-16.9119269620305,-16.8023209402444,
1.92687841044976));
#17307=CARTESIAN_POINT('Ctrl Pts',(-16.5360369434423,-17.1171954523915,
1.90672817703692));
#17308=CARTESIAN_POINT('Ctrl Pts',(-16.3203758924028,-17.2365708955179,
1.89788695942264));
#17309=CARTESIAN_POINT('Ctrl Pts',(-15.8475577563769,-17.3900120669935,
1.87720375137252));
#17310=CARTESIAN_POINT('Ctrl Pts',(-15.5939493045371,-17.4194023058029,
1.86610976835241));
#17311=CARTESIAN_POINT('Ctrl Pts',(-15.0996125733408,-17.3782663055323,
1.8444852394287));
#17312=CARTESIAN_POINT('Ctrl Pts',(-14.8632730729469,-17.311848309036,1.83414667860658));
#17313=CARTESIAN_POINT('Ctrl Pts',(-14.4203422351862,-17.0896519219109,
1.81477087642983));
#17314=CARTESIAN_POINT('Ctrl Pts',(-14.219554067097,-16.9328779450836,1.80494338296207));
#17315=CARTESIAN_POINT('Ctrl Pts',(-13.8924269064666,-16.5521679595822,
1.78336560084335));
#17316=CARTESIAN_POINT('Ctrl Pts',(-13.7685238999814,-16.3326704187886,
1.77234014372881));
#17317=CARTESIAN_POINT('Ctrl Pts',(-13.615111347141,-15.8665290015337,1.75132541995281));
#17318=CARTESIAN_POINT('Ctrl Pts',(-13.5839053729158,-15.6253250129745,
1.74199046187692));
#17319=CARTESIAN_POINT('Ctrl Pts',(-13.6137650496087,-15.132767229072,1.72267736511237));
#17320=CARTESIAN_POINT('Ctrl Pts',(-13.6789651478017,-14.886362035283,1.71191650743335));
#17321=CARTESIAN_POINT('Ctrl Pts',(-13.899100443672,-14.43837788376,1.69013027367801));
#17322=CARTESIAN_POINT('Ctrl Pts',(-14.0499413576698,-14.2401343662606,
1.67932080826729));
#17323=CARTESIAN_POINT('Ctrl Pts',(-14.4160367346151,-13.9147211425423,
1.65898555861985));
#17324=CARTESIAN_POINT('Ctrl Pts',(-14.6268766935179,-13.7895204893169,
1.65019437036221));
#17325=CARTESIAN_POINT('Ctrl Pts',(-15.0942338092302,-13.6215167249473,
1.62975005208956));
#17326=CARTESIAN_POINT('Ctrl Pts',(-15.3476308678393,-13.5842452796376,
1.61866531636737));
#17327=CARTESIAN_POINT('Ctrl Pts',(-15.8444702391433,-13.6105884798816,
1.59693131062353));
#17328=CARTESIAN_POINT('Ctrl Pts',(-16.08336246302,-13.6701795096518,1.5864810821075));
#17329=CARTESIAN_POINT('Ctrl Pts',(-16.5309276996222,-13.8787046238777,
1.56690255032262));
#17330=CARTESIAN_POINT('Ctrl Pts',(-16.7343891762498,-14.0276855562089,
1.55744475601725));
#17331=CARTESIAN_POINT('Ctrl Pts',(-17.0726975821131,-14.3962002472928,
1.53608441974962));
#17332=CARTESIAN_POINT('Ctrl Pts',(-17.2040353110832,-14.6122988907963,
1.52502511181075));
#17333=CARTESIAN_POINT('Ctrl Pts',(-17.3660722950728,-15.0568360880483,
1.50464020377303));
#17334=CARTESIAN_POINT('Ctrl Pts',(-17.405,-15.2776473825378,1.49542357897272));
#17335=CARTESIAN_POINT('Ctrl Pts',(-17.405,-15.5,1.48699999999984));
#17336=CARTESIAN_POINT('Origin',(15.5,-15.5,-1.713));
#17337=CARTESIAN_POINT('',(13.595,-15.5,10.5495));
#17338=CARTESIAN_POINT('',(13.595,-15.5,10.612));
#17339=CARTESIAN_POINT('',(13.595,-15.5,-1.713));
#17340=CARTESIAN_POINT('',(16.8346987578547,-14.140733938563,10.7369999999983));
#17341=CARTESIAN_POINT('Ctrl Pts',(13.595,-15.5,10.5495));
#17342=CARTESIAN_POINT('Ctrl Pts',(13.595,-15.2823467000937,10.5590211417282));
#17343=CARTESIAN_POINT('Ctrl Pts',(13.6323041951647,-15.0660657837748,10.5684822491787));
#17344=CARTESIAN_POINT('Ctrl Pts',(13.7873649268709,-14.6308616850732,10.587520048772));
#17345=CARTESIAN_POINT('Ctrl Pts',(13.9125858088488,-14.4189647250675,10.5963406221173));
#17346=CARTESIAN_POINT('Ctrl Pts',(14.2422054289987,-14.0470719665195,10.6169620282376));
#17347=CARTESIAN_POINT('Ctrl Pts',(14.4460836501414,-13.8930475031147,10.6280545895014));
#17348=CARTESIAN_POINT('Ctrl Pts',(14.8934335791397,-13.6778143228103,10.6497095760738));
#17349=CARTESIAN_POINT('Ctrl Pts',(15.1310246903917,-13.6152821794268,10.6600781679263));
#17350=CARTESIAN_POINT('Ctrl Pts',(15.6249820475859,-13.5825299192131,10.6795075533079));
#17351=CARTESIAN_POINT('Ctrl Pts',(15.8768366076506,-13.6157681297062,10.6892302773471));
#17352=CARTESIAN_POINT('Ctrl Pts',(16.2498388977282,-13.742994250647,10.7061437733815));
#17353=CARTESIAN_POINT('Ctrl Pts',(16.3791092039297,-13.8039772459343,10.7123748699156));
#17354=CARTESIAN_POINT('Ctrl Pts',(16.6212238560751,-13.9533744742352,10.7248147672707));
#17355=CARTESIAN_POINT('Ctrl Pts',(16.733361069962,-14.0412278227297,10.7309845113732));
#17356=CARTESIAN_POINT('Ctrl Pts',(16.8346987578564,-14.1407339385622,10.7369999999993));
#17357=CARTESIAN_POINT('',(15.5,-13.595,10.737));
#17358=CARTESIAN_POINT('Origin',(15.5,-15.5,10.737));
#17359=CARTESIAN_POINT('Ctrl Pts',(15.5000000000012,-13.595,10.7370000000001));
#17360=CARTESIAN_POINT('Ctrl Pts',(15.2556996093285,-13.5949999999998,10.7277449543099));
#17361=CARTESIAN_POINT('Ctrl Pts',(15.0136080866584,-13.6419929658385,10.7175457464537));
#17362=CARTESIAN_POINT('Ctrl Pts',(14.554139443356,-13.8274550958886,10.6960828163414));
#17363=CARTESIAN_POINT('Ctrl Pts',(14.3421784047168,-13.9665356718971,10.6850109033022));
#17364=CARTESIAN_POINT('Ctrl Pts',(13.9869783327278,-14.3163501723868,10.6639033120506));
#17365=CARTESIAN_POINT('Ctrl Pts',(13.8461983203702,-14.5226600964613,10.6547532766204));
#17366=CARTESIAN_POINT('Ctrl Pts',(13.6524557631648,-14.9751135388291,10.6349609125623));
#17367=CARTESIAN_POINT('Ctrl Pts',(13.6003769945158,-15.2165551523544,10.6243991621894));
#17368=CARTESIAN_POINT('Ctrl Pts',(13.595131497578,-15.4741482639885,10.6131308720917));
#17369=CARTESIAN_POINT('Ctrl Pts',(13.595,-15.487077060846,10.6125653079245));
#17370=CARTESIAN_POINT('Ctrl Pts',(13.595,-15.5,10.612));
#17371=CARTESIAN_POINT('Origin',(15.5,-15.5,-1.713));
#17372=CARTESIAN_POINT('',(13.595,-15.5,10.0495));
#17373=CARTESIAN_POINT('',(13.595,-15.5,10.112));
#17374=CARTESIAN_POINT('',(13.595,-15.5,-1.713));
#17375=CARTESIAN_POINT('Ctrl Pts',(13.595,-15.5,10.0495));
#17376=CARTESIAN_POINT('Ctrl Pts',(13.595,-15.4885854639047,10.0499993235387));
#17377=CARTESIAN_POINT('Ctrl Pts',(13.5951025916268,-15.4771662931107,10.05049884982));
#17378=CARTESIAN_POINT('Ctrl Pts',(13.5997094823034,-15.2210165043723,10.0617040024332));
#17379=CARTESIAN_POINT('Ctrl Pts',(13.6512365443426,-14.9793981148592,10.072273485789));
#17380=CARTESIAN_POINT('Ctrl Pts',(13.8439031047659,-14.5265938173909,10.0920811978392));
#17381=CARTESIAN_POINT('Ctrl Pts',(13.9840951254248,-14.3200776670448,10.1012125562281));
#17382=CARTESIAN_POINT('Ctrl Pts',(14.3385164397248,-13.9692567662194,10.1223126573759));
#17383=CARTESIAN_POINT('Ctrl Pts',(14.5504233063801,-13.8295157144395,10.1333969642722));
#17384=CARTESIAN_POINT('Ctrl Pts',(15.0075282912686,-13.643915876073,10.1547733618354));
#17385=CARTESIAN_POINT('Ctrl Pts',(15.2470549408166,-13.5964192294268,10.164886418997));
#17386=CARTESIAN_POINT('Ctrl Pts',(15.7413437873917,-13.5935846520099,10.1836739949659));
#17387=CARTESIAN_POINT('Ctrl Pts',(15.9914666160098,-13.6422633525157,10.1941524169219));
#17388=CARTESIAN_POINT('Ctrl Pts',(16.454548301879,-13.8328030202801,10.2158632803459));
#17389=CARTESIAN_POINT('Ctrl Pts',(16.6635495836274,-13.9713189092327,10.2268107153369));
#17390=CARTESIAN_POINT('Ctrl Pts',(17.0116345047798,-14.315834058712,10.2475328482822));
#17391=CARTESIAN_POINT('Ctrl Pts',(17.14934504374,-14.5166690611182,10.2564846483428));
#17392=CARTESIAN_POINT('Ctrl Pts',(17.3469105138776,-14.9692567735138,10.2762828859804));
#17393=CARTESIAN_POINT('Ctrl Pts',(17.4009094163838,-15.2184123682085,10.287182080849));
#17394=CARTESIAN_POINT('Ctrl Pts',(17.4085380460922,-15.716338685697,10.3089636345449));
#17395=CARTESIAN_POINT('Ctrl Pts',(17.3647938906909,-15.9603021616113,10.3196357026077));
#17396=CARTESIAN_POINT('Ctrl Pts',(17.1871822359435,-16.4179451539634,10.3396550811008));
#17397=CARTESIAN_POINT('Ctrl Pts',(17.055093772971,-16.6273392867399,10.3485778184913));
#17398=CARTESIAN_POINT('Ctrl Pts',(16.713976725445,-16.9896048648143,10.3694242234719));
#17399=CARTESIAN_POINT('Ctrl Pts',(16.5062763678168,-17.1370893814211,10.3805185386244));
#17400=CARTESIAN_POINT('Ctrl Pts',(16.0541901813914,-17.3387032194885,10.4020550671098));
#17401=CARTESIAN_POINT('Ctrl Pts',(15.8155896670134,-17.3943024572225,10.4123102607089));
#17402=CARTESIAN_POINT('Ctrl Pts',(15.3189724577376,-17.413337548513,10.4315403860297));
#17403=CARTESIAN_POINT('Ctrl Pts',(15.0655514661997,-17.3721441088755,10.4416772271422));
#17404=CARTESIAN_POINT('Ctrl Pts',(14.5946111909685,-17.1945017469419,10.4634037110872));
#17405=CARTESIAN_POINT('Ctrl Pts',(14.3810461747161,-17.0617330829786,10.4743983331963));
#17406=CARTESIAN_POINT('Ctrl Pts',(14.0229544734009,-16.7269854446001,10.4952859241593));
#17407=CARTESIAN_POINT('Ctrl Pts',(13.8796963628073,-16.5304158725953,10.5044249399564));
#17408=CARTESIAN_POINT('Ctrl Pts',(13.6692420751003,-16.0840200856592,10.523952314713));
#17409=CARTESIAN_POINT('Ctrl Pts',(13.608054017622,-15.8365612745352,10.5347772845785));
#17410=CARTESIAN_POINT('Ctrl Pts',(13.5956225641649,-15.5562603941975,10.5470389153894));
#17411=CARTESIAN_POINT('Ctrl Pts',(13.595,-15.5281187444259,10.5482699586865));
#17412=CARTESIAN_POINT('Ctrl Pts',(13.595,-15.5,10.5495));
#17413=CARTESIAN_POINT('Ctrl Pts',(13.595,-15.5,10.612));
#17414=CARTESIAN_POINT('Ctrl Pts',(13.595,-15.7412909591996,10.60144483993));
#17415=CARTESIAN_POINT('Ctrl Pts',(13.6408457688845,-15.9805397719341,10.5909790126015));
#17416=CARTESIAN_POINT('Ctrl Pts',(13.8197845796609,-16.4297661061609,10.5713278168785));
#17417=CARTESIAN_POINT('Ctrl Pts',(13.9513442543879,-16.6354551426844,10.5625007719194));
#17418=CARTESIAN_POINT('Ctrl Pts',(14.2882893247519,-16.9906652611646,10.5419667364927));
#17419=CARTESIAN_POINT('Ctrl Pts',(14.4920727561511,-17.1353594156637,10.5310818412297));
#17420=CARTESIAN_POINT('Ctrl Pts',(14.9478948820757,-17.3406183841806,10.5093240536131));
#17421=CARTESIAN_POINT('Ctrl Pts',(15.1963067151894,-17.3974961759311,10.4986692043588));
#17422=CARTESIAN_POINT('Ctrl Pts',(15.6898143706627,-17.4108176576472,10.4796818505767));
#17423=CARTESIAN_POINT('Ctrl Pts',(15.9301253696938,-17.3714395343302,10.4699711404288));
#17424=CARTESIAN_POINT('Ctrl Pts',(16.3918716927025,-17.2018652329606,10.4487694257956));
#17425=CARTESIAN_POINT('Ctrl Pts',(16.6077003531134,-17.0699625826955,10.4377079897539));
#17426=CARTESIAN_POINT('Ctrl Pts',(16.9752781837248,-16.7308092166127,10.4163646641975));
#17427=CARTESIAN_POINT('Ctrl Pts',(17.1236678774154,-16.5271438579512,10.4069319272946));
#17428=CARTESIAN_POINT('Ctrl Pts',(17.3311410686046,-16.0792265773098,10.387337995508));
#17429=CARTESIAN_POINT('Ctrl Pts',(17.3902018446824,-15.840145597041,10.376879509932));
#17430=CARTESIAN_POINT('Ctrl Pts',(17.4153996480397,-15.343131166637,10.3551378463097));
#17431=CARTESIAN_POINT('Ctrl Pts',(17.3775197193691,-15.0897602206549,10.3440542528722));
#17432=CARTESIAN_POINT('Ctrl Pts',(17.2083963180158,-14.622830943006,10.3236286501754));
#17433=CARTESIAN_POINT('Ctrl Pts',(17.0827455582927,-14.4123598146853,10.3148380476183));
#17434=CARTESIAN_POINT('Ctrl Pts',(16.7565163753647,-14.0470286545255,10.2944886014262));
#17435=CARTESIAN_POINT('Ctrl Pts',(16.5578765661879,-13.8966142348298,10.2836734513476));
#17436=CARTESIAN_POINT('Ctrl Pts',(16.1093241222814,-13.6775176070575,10.261888406499));
#17437=CARTESIAN_POINT('Ctrl Pts',(15.8627681320143,-13.6129016625927,10.2511346128306));
#17438=CARTESIAN_POINT('Ctrl Pts',(15.3701374357996,-13.5842067572065,10.2318442300529));
#17439=CARTESIAN_POINT('Ctrl Pts',(15.1289999089402,-13.615985222063,10.2224860842217));
#17440=CARTESIAN_POINT('Ctrl Pts',(14.6631596610225,-13.7705267597449,10.2014580764508));
#17441=CARTESIAN_POINT('Ctrl Pts',(14.4439092045079,-13.8949918882011,10.1904296849652));
#17442=CARTESIAN_POINT('Ctrl Pts',(14.0641127575733,-14.2229686951434,10.1688679275381));
#17443=CARTESIAN_POINT('Ctrl Pts',(13.9079289550465,-14.4239586314856,10.1590709260069));
#17444=CARTESIAN_POINT('Ctrl Pts',(13.6867555065337,-14.8672400535419,10.1396797876843));
#17445=CARTESIAN_POINT('Ctrl Pts',(13.6208440607317,-15.1037768687542,10.1293325954178));
#17446=CARTESIAN_POINT('Ctrl Pts',(13.597065752003,-15.3974989140194,10.1164838620291));
#17447=CARTESIAN_POINT('Ctrl Pts',(13.595,-15.4487792632927,10.1142406271526));
#17448=CARTESIAN_POINT('Ctrl Pts',(13.595,-15.5,10.112));
#17449=CARTESIAN_POINT('Origin',(15.5,-15.5,-1.713));
#17450=CARTESIAN_POINT('',(13.595,-15.5,9.54949999999996));
#17451=CARTESIAN_POINT('',(13.595,-15.5,9.612));
#17452=CARTESIAN_POINT('',(13.595,-15.5,-1.713));
#17453=CARTESIAN_POINT('Ctrl Pts',(13.595,-15.5,9.54949999999995));
#17454=CARTESIAN_POINT('Ctrl Pts',(13.595,-15.4502744854574,9.55167521935877));
#17455=CARTESIAN_POINT('Ctrl Pts',(13.5969469079297,-15.4004916147963,9.553852947734));
#17456=CARTESIAN_POINT('Ctrl Pts',(13.6199184623743,-15.1081582486334,9.56664093400535));
#17457=CARTESIAN_POINT('Ctrl Pts',(13.6852966251491,-14.8714150898636,9.5769971526742));
#17458=CARTESIAN_POINT('Ctrl Pts',(13.9053946919737,-14.4277657801821,9.59640438406885));
#17459=CARTESIAN_POINT('Ctrl Pts',(14.0609593043538,-14.2265640689728,9.60616982353457));
#17460=CARTESIAN_POINT('Ctrl Pts',(14.439795526841,-13.8976963553052,9.62771469008669));
#17461=CARTESIAN_POINT('Ctrl Pts',(14.65878494751,-13.7726412812994,9.63874609596868));
#17462=CARTESIAN_POINT('Ctrl Pts',(15.1243079177073,-13.6169138584148,9.65978802202635));
#17463=CARTESIAN_POINT('Ctrl Pts',(15.3653763046083,-13.5845343459454,9.6691710250572));
#17464=CARTESIAN_POINT('Ctrl Pts',(15.8580824961113,-13.6120073228381,9.68843754154408));
#17465=CARTESIAN_POINT('Ctrl Pts',(16.1047951463693,-13.676010096271,9.69918385866022));
#17466=CARTESIAN_POINT('Ctrl Pts',(16.5539411468359,-13.894015560723,9.72096752351754));
#17467=CARTESIAN_POINT('Ctrl Pts',(16.7529957164446,-14.0439814927899,9.73178857688824));
#17468=CARTESIAN_POINT('Ctrl Pts',(17.0800802835538,-14.4085105467076,9.75215288446747));
#17469=CARTESIAN_POINT('Ctrl Pts',(17.2062028388546,-14.6185957461662,9.76094338347164));
#17470=CARTESIAN_POINT('Ctrl Pts',(17.3764987911599,-15.0850757309887,9.78134933206405));
#17471=CARTESIAN_POINT('Ctrl Pts',(17.4150163189817,-15.3384178102987,9.79243166274253));
#17472=CARTESIAN_POINT('Ctrl Pts',(17.3910192245,-15.8356128863494,9.81418122862402));
#17473=CARTESIAN_POINT('Ctrl Pts',(17.3325145603624,-16.074890375008,9.82464831036762));
#17474=CARTESIAN_POINT('Ctrl Pts',(17.1261431374813,-16.5231756890091,9.84425834160127));
#17475=CARTESIAN_POINT('Ctrl Pts',(16.9783714265357,-16.7270543597511,9.85366535294237));
#17476=CARTESIAN_POINT('Ctrl Pts',(16.6117745768507,-17.0670904080252,9.8749908213987));
#17477=CARTESIAN_POINT('Ctrl Pts',(16.3962299527202,-17.1995836267748,9.88605441411614));
#17478=CARTESIAN_POINT('Ctrl Pts',(15.9348178116792,-17.3703597238175,9.90726975463571));
#17479=CARTESIAN_POINT('Ctrl Pts',(15.6945683061102,-17.4103438385966,9.91701211657193));
#17480=CARTESIAN_POINT('Ctrl Pts',(15.2009978140301,-17.3982405944492,9.93597520523219));
#17481=CARTESIAN_POINT('Ctrl Pts',(14.9524496570676,-17.3419779720927,9.94662176381363));
#17482=CARTESIAN_POINT('Ctrl Pts',(14.4960700533142,-17.1378253197796,9.96837647320892));
#17483=CARTESIAN_POINT('Ctrl Pts',(14.2918860957013,-16.9935915259762,9.97926647282571));
#17484=CARTESIAN_POINT('Ctrl Pts',(13.9540961430899,-16.6391862209806,9.9998149125721));
#17485=CARTESIAN_POINT('Ctrl Pts',(13.8220704882375,-16.4338694301794,10.0086483188896));
#17486=CARTESIAN_POINT('Ctrl Pts',(13.6414552862163,-15.9836817917745,10.0283415664139));
#17487=CARTESIAN_POINT('Ctrl Pts',(13.595,-15.7428901843941,10.0388748825724));
#17488=CARTESIAN_POINT('Ctrl Pts',(13.595,-15.5,10.0495));
#17489=CARTESIAN_POINT('Ctrl Pts',(13.595,-15.5,10.112));
#17490=CARTESIAN_POINT('Ctrl Pts',(13.595,-15.7008367103392,10.1032144921112));
#17491=CARTESIAN_POINT('Ctrl Pts',(13.6267629324258,-15.900756920881,10.0944690760771));
#17492=CARTESIAN_POINT('Ctrl Pts',(13.7653182344057,-16.3243321971831,10.0759399738766));
#17493=CARTESIAN_POINT('Ctrl Pts',(13.8851281171556,-16.5396306949641,10.0671051936536));
#17494=CARTESIAN_POINT('Ctrl Pts',(14.200786992495,-16.9147965477635,10.0469410846696));
#17495=CARTESIAN_POINT('Ctrl Pts',(14.3942454641661,-17.0706361452585,10.0362035628064));
#17496=CARTESIAN_POINT('Ctrl Pts',(14.835280621152,-17.3030209097119,10.0144126602632));
#17497=CARTESIAN_POINT('Ctrl Pts',(15.0797818291005,-17.3751462450849,10.0035724623181));
#17498=CARTESIAN_POINT('Ctrl Pts',(15.5713993833167,-17.418869326979,9.98399176101256));
#17499=CARTESIAN_POINT('Ctrl Pts',(15.8134360435395,-17.3944470517877,9.97489501092434));
#17500=CARTESIAN_POINT('Ctrl Pts',(16.2830697953039,-17.2543658920727,9.95403957175722));
#17501=CARTESIAN_POINT('Ctrl Pts',(16.5053789616836,-17.137134027351,9.94305351235477));
#17502=CARTESIAN_POINT('Ctrl Pts',(16.8968287771957,-16.8201505199817,9.9212907285304));
#17503=CARTESIAN_POINT('Ctrl Pts',(17.0606228992972,-16.6217591407651,9.91107082855505));
#17504=CARTESIAN_POINT('Ctrl Pts',(17.2948368693994,-16.1829939416919,9.89187725029288));
#17505=CARTESIAN_POINT('Ctrl Pts',(17.3671514122205,-15.949046830156,9.88164334340155));
#17506=CARTESIAN_POINT('Ctrl Pts',(17.4211345562518,-15.4572525691451,9.86013003364604));
#17507=CARTESIAN_POINT('Ctrl Pts',(17.3986235514731,-15.2036525256751,9.84903641844612));
#17508=CARTESIAN_POINT('Ctrl Pts',(17.2580021132843,-14.7261927064949,9.82815016213902));
#17509=CARTESIAN_POINT('Ctrl Pts',(17.1437161358039,-14.5062482392129,9.81920140200463));
#17510=CARTESIAN_POINT('Ctrl Pts',(16.8380073730827,-14.1219539327206,9.79921458188554));
#17511=CARTESIAN_POINT('Ctrl Pts',(16.649512387961,-13.9612078910303,9.78855778107861));
#17512=CARTESIAN_POINT('Ctrl Pts',(16.2158461956214,-13.7166562727637,9.76677992681519));
#17513=CARTESIAN_POINT('Ctrl Pts',(15.9734738382061,-13.6375845413723,9.75586844455832));
#17514=CARTESIAN_POINT('Ctrl Pts',(15.4829480248446,-13.5798368529878,9.73602235270462));
#17515=CARTESIAN_POINT('Ctrl Pts',(15.23999153869,-13.5974435708591,9.7270964252791));
#17516=CARTESIAN_POINT('Ctrl Pts',(14.7669894001789,-13.7242335415259,9.70640408698826));
#17517=CARTESIAN_POINT('Ctrl Pts',(14.5420740146174,-13.8347603326945,9.69546594905376));
#17518=CARTESIAN_POINT('Ctrl Pts',(14.1440292603168,-14.1383602326029,9.67374605320853));
#17519=CARTESIAN_POINT('Ctrl Pts',(13.9758112521117,-14.3297413092978,9.66319241866602));
#17520=CARTESIAN_POINT('Ctrl Pts',(13.7289315632306,-14.7578028599957,9.64446706649201));
#17521=CARTESIAN_POINT('Ctrl Pts',(13.6491027494895,-14.9884388844074,9.63437800155712));
#17522=CARTESIAN_POINT('Ctrl Pts',(13.6015031498374,-15.3181544373058,9.61995474902438));
#17523=CARTESIAN_POINT('Ctrl Pts',(13.595,-15.4091197940947,9.61597551206935));
#17524=CARTESIAN_POINT('Ctrl Pts',(13.595,-15.5,9.612));
#17525=CARTESIAN_POINT('Origin',(15.5,-15.5,-1.713));
#17526=CARTESIAN_POINT('',(13.595,-15.5,9.04949999999995));
#17527=CARTESIAN_POINT('',(13.595,-15.5,9.11199999999999));
#17528=CARTESIAN_POINT('',(13.595,-15.5,-1.713));
#17529=CARTESIAN_POINT('Ctrl Pts',(13.595,-15.5,9.04949999999995));
#17530=CARTESIAN_POINT('Ctrl Pts',(13.595,-15.410571107507,9.05341202504338));
#17531=CARTESIAN_POINT('Ctrl Pts',(13.6012971006541,-15.3210561673908,9.05732781419969));
#17532=CARTESIAN_POINT('Ctrl Pts',(13.6479436729555,-14.9926259880107,9.07169483866952));
#17533=CARTESIAN_POINT('Ctrl Pts',(13.7272713627419,-14.761759744373,9.0817939744367));
#17534=CARTESIAN_POINT('Ctrl Pts',(13.9732357126391,-14.3331017483525,9.10054541783218));
#17535=CARTESIAN_POINT('Ctrl Pts',(14.1410360274765,-14.1413467593241,9.11106733583993));
#17536=CARTESIAN_POINT('Ctrl Pts',(14.5384579830271,-13.8368377733064,9.13278352142774));
#17537=CARTESIAN_POINT('Ctrl Pts',(14.7631831589794,-13.7258021200914,9.14372558345101));
#17538=CARTESIAN_POINT('Ctrl Pts',(15.2359343291776,-13.5980067128105,9.16443040526644));
#17539=CARTESIAN_POINT('Ctrl Pts',(15.4788180628624,-13.5798822975231,9.17336688771192));
#17540=CARTESIAN_POINT('Ctrl Pts',(15.9694321495217,-13.6365619282601,9.19319296285935));
#17541=CARTESIAN_POINT('Ctrl Pts',(16.2119737247838,-13.7151069957101,9.20409933641036));
#17542=CARTESIAN_POINT('Ctrl Pts',(16.6462128309944,-13.9587404009295,9.22587881147182));
#17543=CARTESIAN_POINT('Ctrl Pts',(16.8350899823954,-14.119118253725,9.23654203709323));
#17544=CARTESIAN_POINT('Ctrl Pts',(17.1415594948502,-14.5027190331107,9.2565425083515));
#17545=CARTESIAN_POINT('Ctrl Pts',(17.2562689319036,-14.72230470962,9.26548008353523));
#17546=CARTESIAN_POINT('Ctrl Pts',(17.3979598892063,-15.1993833986608,9.28634966748277));
#17547=CARTESIAN_POINT('Ctrl Pts',(17.4210424631524,-15.4529910108418,9.29744361377241));
#17548=CARTESIAN_POINT('Ctrl Pts',(17.3681244205606,-15.9450092692229,9.31896672218804));
#17549=CARTESIAN_POINT('Ctrl Pts',(17.2962975705816,-16.17916100399,9.32920958022685));
#17550=CARTESIAN_POINT('Ctrl Pts',(17.0630855458631,-16.6182768382877,9.34841849686281));
#17551=CARTESIAN_POINT('Ctrl Pts',(16.8998828532734,-16.8168700849708,9.35860327774385));
#17552=CARTESIAN_POINT('Ctrl Pts',(16.5093288066214,-17.1347108439304,9.38035087640664));
#17553=CARTESIAN_POINT('Ctrl Pts',(16.2872475205707,-17.2525035314174,9.39134056928365));
#17554=CARTESIAN_POINT('Ctrl Pts',(15.8179017431069,-17.3937009619574,9.41220951424044));
#17555=CARTESIAN_POINT('Ctrl Pts',(15.5759382291941,-17.4186930865504,9.42132366671565));
#17556=CARTESIAN_POINT('Ctrl Pts',(15.0842361807923,-17.3761386070571,9.44088200900592));
#17557=CARTESIAN_POINT('Ctrl Pts',(14.8395667426201,-17.3045949272268,9.45171585803926));
#17558=CARTESIAN_POINT('Ctrl Pts',(14.3979327965919,-17.0732344339334,9.47350704190107));
#17559=CARTESIAN_POINT('Ctrl Pts',(14.20406620879,-16.9178105839672,9.48425093144459));
#17560=CARTESIAN_POINT('Ctrl Pts',(13.8875820471894,-16.5434075363857,9.50442962119228));
#17561=CARTESIAN_POINT('Ctrl Pts',(13.7673152099352,-16.3284898256387,9.51325810036557));
#17562=CARTESIAN_POINT('Ctrl Pts',(13.6272628027254,-15.9038712930308,9.53183283932479));
#17563=CARTESIAN_POINT('Ctrl Pts',(13.595,-15.7024108270756,9.54064563311126));
#17564=CARTESIAN_POINT('Ctrl Pts',(13.595,-15.5,9.54949999999996));
#17565=CARTESIAN_POINT('Ctrl Pts',(13.595,-15.5,9.612));
#17566=CARTESIAN_POINT('Ctrl Pts',(13.595,-15.6592363994984,9.60503427823716));
#17567=CARTESIAN_POINT('Ctrl Pts',(13.6149664418887,-15.8182113811384,9.59807999207632));
#17568=CARTESIAN_POINT('Ctrl Pts',(13.7162061731805,-16.213048823518,9.58080801296959));
#17569=CARTESIAN_POINT('Ctrl Pts',(13.82389619804,-16.438630035475,9.57163400936754));
#17570=CARTESIAN_POINT('Ctrl Pts',(14.1178117380362,-16.8335843974178,9.55186080266696));
#17571=CARTESIAN_POINT('Ctrl Pts',(14.3003316472966,-16.9998901349052,9.54130875774747));
#17572=CARTESIAN_POINT('Ctrl Pts',(14.7265604220024,-17.2594103896354,9.51948526369304));
#17573=CARTESIAN_POINT('Ctrl Pts',(14.9681598682303,-17.3468610247554,9.50841979669683));
#17574=CARTESIAN_POINT('Ctrl Pts',(15.4592480622578,-17.419886963939,9.48821822971879));
#17575=CARTESIAN_POINT('Ctrl Pts',(15.7032719165713,-17.4095316129779,9.47939838857678));
#17576=CARTESIAN_POINT('Ctrl Pts',(16.179705827867,-17.2967441184858,9.45888230731463));
#17577=CARTESIAN_POINT('Ctrl Pts',(16.4071510785082,-17.1933275469165,9.44800384489947));
#17578=CARTESIAN_POINT('Ctrl Pts',(16.8136626439144,-16.9024937973762,9.42624241806902));
#17579=CARTESIAN_POINT('Ctrl Pts',(16.9877023586233,-16.7163326475971,9.41557735292926));
#17580=CARTESIAN_POINT('Ctrl Pts',(17.2472648561672,-16.2964293272925,9.39655988237394));
#17581=CARTESIAN_POINT('Ctrl Pts',(17.3340082850086,-16.0689342103612,9.38688776073332));
#17582=CARTESIAN_POINT('Ctrl Pts',(17.4195245794063,-15.584650961036,9.36570301666835));
#17583=CARTESIAN_POINT('Ctrl Pts',(17.4140187813701,-15.3318500259603,9.35464435809111));
#17584=CARTESIAN_POINT('Ctrl Pts',(17.3056516691084,-14.8434366460597,9.33327894339729));
#17585=CARTESIAN_POINT('Ctrl Pts',(17.2040806530936,-14.612561851177,9.32381356348501));
#17586=CARTESIAN_POINT('Ctrl Pts',(16.9209888558443,-14.207971510667,9.30423964142568));
#17587=CARTESIAN_POINT('Ctrl Pts',(16.7440258956182,-14.036809199301,9.2937918909984));
#17588=CARTESIAN_POINT('Ctrl Pts',(16.3271388577635,-13.7653056439892,9.27206019620634));
#17589=CARTESIAN_POINT('Ctrl Pts',(16.0891392566732,-13.6707238628737,9.26097513097483));
#17590=CARTESIAN_POINT('Ctrl Pts',(15.6004510343452,-13.5821870637115,9.24052522657206));
#17591=CARTESIAN_POINT('Ctrl Pts',(15.3552296432451,-13.5850223738718,9.23173377105869));
#17592=CARTESIAN_POINT('Ctrl Pts',(14.8753994325026,-13.6834655640153,9.2114027672495));
#17593=CARTESIAN_POINT('Ctrl Pts',(14.6455947298484,-13.779562778925,9.20059501056258));
#17594=CARTESIAN_POINT('Ctrl Pts',(14.2307765791858,-14.0571584130691,9.17880844566771));
#17595=CARTESIAN_POINT('Ctrl Pts',(14.0509806590752,-14.2378250741837,9.1680454900741));
#17596=CARTESIAN_POINT('Ctrl Pts',(13.7785522306151,-14.6492698322716,9.1487256161107));
#17597=CARTESIAN_POINT('Ctrl Pts',(13.6848174176791,-14.8736934308153,9.13939748771596));
#17598=CARTESIAN_POINT('Ctrl Pts',(13.6084807912089,-15.2383437374753,9.12344603073171));
#17599=CARTESIAN_POINT('Ctrl Pts',(13.595,-15.3691547988651,9.11772376207938));
#17600=CARTESIAN_POINT('Ctrl Pts',(13.595,-15.5,9.11199999999999));
#17601=CARTESIAN_POINT('Origin',(15.5,-15.5,-1.713));
#17602=CARTESIAN_POINT('',(13.595,-15.5,8.54949999999994));
#17603=CARTESIAN_POINT('',(13.595,-15.5,8.61199999999998));
#17604=CARTESIAN_POINT('',(13.595,-15.5,-1.713));
#17605=CARTESIAN_POINT('Ctrl Pts',(13.595,-15.5,8.54949999999994));
#17606=CARTESIAN_POINT('Ctrl Pts',(13.595,-15.3706312184885,8.55515917679397));
#17607=CARTESIAN_POINT('Ctrl Pts',(13.6081782572954,-15.2412882250917,8.56081722549889));
#17608=CARTESIAN_POINT('Ctrl Pts',(13.6833684033628,-14.8779059502326,8.57671321302554));
#17609=CARTESIAN_POINT('Ctrl Pts',(13.77658581932,-14.6532588833752,8.58606387124224));
#17610=CARTESIAN_POINT('Ctrl Pts',(14.0480634340968,-14.2411825017125,8.60536153973686));
#17611=CARTESIAN_POINT('Ctrl Pts',(14.2274385998401,-14.0601021103429,8.6161176047424));
#17612=CARTESIAN_POINT('Ctrl Pts',(14.6416556152634,-13.7815167346891,8.63790304419398));
#17613=CARTESIAN_POINT('Ctrl Pts',(14.8712932594593,-13.6848751833049,8.64871637793111));
#17614=CARTESIAN_POINT('Ctrl Pts',(15.3508753640126,-13.5853670120839,8.66906127606558));
#17615=CARTESIAN_POINT('Ctrl Pts',(15.5960042721982,-13.5819698294477,8.67785201458072));
#17616=CARTESIAN_POINT('Ctrl Pts',(16.0848780449043,-13.6693485876092,8.69828361937024));
#17617=CARTESIAN_POINT('Ctrl Pts',(16.3231535648926,-13.7634022146335,8.70936758555232));
#17618=CARTESIAN_POINT('Ctrl Pts',(16.7407498898442,-14.034021388476,8.73110680746206));
#17619=CARTESIAN_POINT('Ctrl Pts',(16.9181324415661,-14.2048270363753,8.74156265260331));
#17620=CARTESIAN_POINT('Ctrl Pts',(17.2020374331519,-14.6086982647906,8.76115165300497));
#17621=CARTESIAN_POINT('Ctrl Pts',(17.3040707483591,-14.8391714882777,8.77059236606621));
#17622=CARTESIAN_POINT('Ctrl Pts',(17.4136129180806,-15.3272046045457,8.7919411463054));
#17623=CARTESIAN_POINT('Ctrl Pts',(17.4197296533386,-15.5800536124631,8.8030019078066));
#17624=CARTESIAN_POINT('Ctrl Pts',(17.3353425167868,-16.0646292820051,8.82419944365709));
#17625=CARTESIAN_POINT('Ctrl Pts',(17.2491193178985,-16.2923574232655,8.83390056640762));
#17626=CARTESIAN_POINT('Ctrl Pts',(16.9905152523131,-16.7128834009353,8.85289534677308));
#17627=CARTESIAN_POINT('Ctrl Pts',(16.8169095940015,-16.8994448139881,8.86355272283891));
#17628=CARTESIAN_POINT('Ctrl Pts',(16.4110314361869,-17.1912511569425,8.88531142655658));
#17629=CARTESIAN_POINT('Ctrl Pts',(16.1837704005117,-17.2952088423174,8.89619474557987));
#17630=CARTESIAN_POINT('Ctrl Pts',(15.7075929037513,-17.4090592639519,8.91672436149072));
#17631=CARTESIAN_POINT('Ctrl Pts',(15.463653614066,-17.4199679649402,8.92554955866493));
#17632=CARTESIAN_POINT('Ctrl Pts',(14.9723958892026,-17.3480839035569,8.94573257267319));
#17633=CARTESIAN_POINT('Ctrl Pts',(14.7305396939158,-17.2611629600836,8.95679618076234));
#17634=CARTESIAN_POINT('Ctrl Pts',(14.3036369416927,-17.0025363920969,8.97862566074327));
#17635=CARTESIAN_POINT('Ctrl Pts',(14.1207134528123,-16.8365948553763,8.98918502892699));
#17636=CARTESIAN_POINT('Ctrl Pts',(13.8260068563253,-16.4423502430572,9.00897268008097));
#17637=CARTESIAN_POINT('Ctrl Pts',(13.7178723046654,-16.2171514711361,9.01812854456953));
#17638=CARTESIAN_POINT('Ctrl Pts',(13.6153487921593,-15.82122928745,9.03544797517697));
#17639=CARTESIAN_POINT('Ctrl Pts',(13.595,-15.6607536629728,9.04246790625661));
#17640=CARTESIAN_POINT('Ctrl Pts',(13.595,-15.5,9.04949999999995));
#17641=CARTESIAN_POINT('Ctrl Pts',(13.595,-15.5,9.11199999999999));
#17642=CARTESIAN_POINT('Ctrl Pts',(13.595,-15.6176025375141,9.10685553204224));
#17643=CARTESIAN_POINT('Ctrl Pts',(13.6058899738159,-15.7352326539994,9.1017098576554));
#17644=CARTESIAN_POINT('Ctrl Pts',(13.6742308708525,-16.0993980787507,9.08577961160329));
#17645=CARTESIAN_POINT('Ctrl Pts',(13.7695912343068,-16.335684931158,9.0759429345776));
#17646=CARTESIAN_POINT('Ctrl Pts',(14.0418391735161,-16.7497899605815,9.05657171208437));
#17647=CARTESIAN_POINT('Ctrl Pts',(14.213179571274,-16.9255805889196,9.04623573433626));
#17648=CARTESIAN_POINT('Ctrl Pts',(14.6205032004331,-17.2086275779359,9.02461385748055));
#17649=CARTESIAN_POINT('Ctrl Pts',(14.8547437993334,-17.3101319062483,9.01351978602818));
#17650=CARTESIAN_POINT('Ctrl Pts',(15.3408779598977,-17.4139985700453,8.99283134050786));
#17651=CARTESIAN_POINT('Ctrl Pts',(15.5873625676778,-17.4186132169735,8.98398811922745));
#17652=CARTESIAN_POINT('Ctrl Pts',(16.0704000423377,-17.3341792674494,8.96384202566675));
#17653=CARTESIAN_POINT('Ctrl Pts',(16.302280786376,-17.2452513854976,8.95311243004288));
#17654=CARTESIAN_POINT('Ctrl Pts',(16.7247704093841,-16.9807684807294,8.93132204514592));
#17655=CARTESIAN_POINT('Ctrl Pts',(16.9099992050158,-16.8056264225291,8.92047410675442));
#17656=CARTESIAN_POINT('Ctrl Pts',(17.1948681402976,-16.4025463604327,8.90086589302953));
#17657=CARTESIAN_POINT('Ctrl Pts',(17.2953896066004,-16.1809976105482,8.89178992172133));
#17658=CARTESIAN_POINT('Ctrl Pts',(17.4102594727264,-15.7046233105122,8.8709511509411));
#17659=CARTESIAN_POINT('Ctrl Pts',(17.4206259784906,-15.4535861600049,8.85996964829425));
#17660=CARTESIAN_POINT('Ctrl Pts',(17.3433017380162,-14.9556633660658,8.83818824873435));
#17661=CARTESIAN_POINT('Ctrl Pts',(17.2539668478584,-14.714110896276,8.82792455362117));
#17662=CARTESIAN_POINT('Ctrl Pts',(16.9920824638983,-14.2910418118942,8.80874987857501));
#17663=CARTESIAN_POINT('Ctrl Pts',(16.8261540972266,-14.1110498671306,8.79852703723084));
#17664=CARTESIAN_POINT('Ctrl Pts',(16.4281347961935,-13.8174079753212,8.77702590985569));
#17665=CARTESIAN_POINT('Ctrl Pts',(16.1976160092304,-13.7095001629511,8.76593277635856));
#17666=CARTESIAN_POINT('Ctrl Pts',(15.7140661012773,-13.5911788993635,8.74502607749248));
#17667=CARTESIAN_POINT('Ctrl Pts',(15.4663234134166,-13.5795094336733,8.73606301415881));
#17668=CARTESIAN_POINT('Ctrl Pts',(14.9803906031063,-13.6508785509999,8.71609299154619));
#17669=CARTESIAN_POINT('Ctrl Pts',(14.7467775836836,-13.7331143078645,8.70544414255637));
#17670=CARTESIAN_POINT('Ctrl Pts',(14.3175348174729,-13.9852300737107,8.68366841977192));
#17671=CARTESIAN_POINT('Ctrl Pts',(14.1274155894136,-14.1550903952042,8.67275073639511));
#17672=CARTESIAN_POINT('Ctrl Pts',(13.831060640224,-14.5502736758525,8.6528801084485));
#17673=CARTESIAN_POINT('Ctrl Pts',(13.7242349538834,-14.7692436797465,8.64396659318698));
#17674=CARTESIAN_POINT('Ctrl Pts',(13.6171517742805,-15.1649283516214,8.62665755242255));
#17675=CARTESIAN_POINT('Ctrl Pts',(13.595,-15.3322765292482,8.61933698472228));
#17676=CARTESIAN_POINT('Ctrl Pts',(13.595,-15.5,8.61199999999998));
#17677=CARTESIAN_POINT('Origin',(15.5,-15.5,-1.713));
#17678=CARTESIAN_POINT('',(13.595,-15.5,8.04949999999993));
#17679=CARTESIAN_POINT('',(13.595,-15.5,8.11199999999998));
#17680=CARTESIAN_POINT('',(13.595,-15.5,-1.713));
#17681=CARTESIAN_POINT('Ctrl Pts',(13.595,-15.5,8.04949999999993));
#17682=CARTESIAN_POINT('Ctrl Pts',(13.595,-15.3311510627383,8.05688621772792));
#17683=CARTESIAN_POINT('Ctrl Pts',(13.617450090195,-15.162692391182,8.06425536346524));
#17684=CARTESIAN_POINT('Ctrl Pts',(13.7255350044953,-14.7660823182981,8.08160488546367));
#17685=CARTESIAN_POINT('Ctrl Pts',(13.8327659814356,-14.5472751736397,8.09051029742115));
#17686=CARTESIAN_POINT('Ctrl Pts',(14.1298564730975,-14.1526035520423,8.11039759942469));
#17687=CARTESIAN_POINT('Ctrl Pts',(14.3202845677445,-13.9830872969252,8.12131945835369));
#17688=CARTESIAN_POINT('Ctrl Pts',(14.749948695651,-13.7317717547783,8.14309364124675));
#17689=CARTESIAN_POINT('Ctrl Pts',(14.9836665076678,-13.6499667726971,8.15373703816555));
#17690=CARTESIAN_POINT('Ctrl Pts',(15.4697825617727,-13.5794388007601,8.17369560500767));
#17691=CARTESIAN_POINT('Ctrl Pts',(15.7176088369337,-13.5915663013557,8.18266876340979));
#17692=CARTESIAN_POINT('Ctrl Pts',(16.200985293846,-13.7108233055556,8.20358935804573));
#17693=CARTESIAN_POINT('Ctrl Pts',(16.431257343107,-13.8191413162432,8.21468211612908));
#17694=CARTESIAN_POINT('Ctrl Pts',(16.8286650382414,-14.1134590723776,8.23617485618652));
#17695=CARTESIAN_POINT('Ctrl Pts',(16.9942395381288,-14.2937174227158,8.24639011857894));
#17696=CARTESIAN_POINT('Ctrl Pts',(17.2539964803157,-14.7150120255227,8.26544538595191));
#17697=CARTESIAN_POINT('Ctrl Pts',(17.3424675768812,-14.9540462123252,8.2756175071007));
#17698=CARTESIAN_POINT('Ctrl Pts',(17.4205245726411,-15.4492943382567,8.29728190456052));
#17699=CARTESIAN_POINT('Ctrl Pts',(17.4107131831776,-15.7004100784271,8.30826684507541));
#17700=CARTESIAN_POINT('Ctrl Pts',(17.2968718994881,-16.177071234859,8.32911816425442));
#17701=CARTESIAN_POINT('Ctrl Pts',(17.1968422883955,-16.3988248467073,8.33820970670972));
#17702=CARTESIAN_POINT('Ctrl Pts',(16.912872666671,-16.8025159955848,8.35779721680401));
#17703=CARTESIAN_POINT('Ctrl Pts',(16.7280319823578,-16.978064308801,8.36863933775223));
#17704=CARTESIAN_POINT('Ctrl Pts',(16.3060846545402,-17.24350511329,8.39043012984293));
#17705=CARTESIAN_POINT('Ctrl Pts',(16.0743470808187,-17.3329541050855,8.40116569947336));
#17706=CARTESIAN_POINT('Ctrl Pts',(15.5915390081312,-17.418405563219,8.42132535761712));
#17707=CARTESIAN_POINT('Ctrl Pts',(15.3451490992139,-17.4143358562908,8.43016215598123));
#17708=CARTESIAN_POINT('Ctrl Pts',(14.858822116526,-17.3115886025642,8.45083342231618));
#17709=CARTESIAN_POINT('Ctrl Pts',(14.6243004008481,-17.210585306207,8.46192718485752));
#17710=CARTESIAN_POINT('Ctrl Pts',(14.2162676588325,-16.9283707280214,8.48355771894564));
#17711=CARTESIAN_POINT('Ctrl Pts',(14.0445125088107,-16.7529121267539,8.49390214693266));
#17712=CARTESIAN_POINT('Ctrl Pts',(13.7714676912101,-16.3395015877221,8.51328836818941));
#17713=CARTESIAN_POINT('Ctrl Pts',(13.675647834441,-16.1036159659264,8.52309510210279));
#17714=CARTESIAN_POINT('Ctrl Pts',(13.6061757673627,-15.7382931073913,8.53907597955402));
#17715=CARTESIAN_POINT('Ctrl Pts',(13.595,-15.6191356188194,8.54428846811807));
#17716=CARTESIAN_POINT('Ctrl Pts',(13.595,-15.5,8.54949999999994));
#17717=CARTESIAN_POINT('Ctrl Pts',(13.595,-15.5,8.61199999999998));
#17718=CARTESIAN_POINT('Ctrl Pts',(13.595,-15.5794309395666,8.6085253307276));
#17719=CARTESIAN_POINT('Ctrl Pts',(13.5999678000312,-15.6589460501022,8.60504697943564));
#17720=CARTESIAN_POINT('Ctrl Pts',(13.641465784413,-15.9883922555288,8.59063550938198));
#17721=CARTESIAN_POINT('Ctrl Pts',(13.7224139007472,-16.2299939283492,8.58006675729009));
#17722=CARTESIAN_POINT('Ctrl Pts',(13.9685057180156,-16.6584443948786,8.56132439217507));
#17723=CARTESIAN_POINT('Ctrl Pts',(14.1277562475251,-16.8433063610855,8.55127142472815));
#17724=CARTESIAN_POINT('Ctrl Pts',(14.5142748007372,-17.1493795222357,8.52993409022724));
#17725=CARTESIAN_POINT('Ctrl Pts',(14.7400863745338,-17.2648350536812,8.51885419849063));
#17726=CARTESIAN_POINT('Ctrl Pts',(15.2202790765396,-17.4005804876757,8.49769357750874));
#17727=CARTESIAN_POINT('Ctrl Pts',(15.4696163825964,-17.4208116915508,8.48849688671508));
#17728=CARTESIAN_POINT('Ctrl Pts',(15.9588807925257,-17.3650172090941,8.46874130275205));
#17729=CARTESIAN_POINT('Ctrl Pts',(16.1943024582505,-17.2907505462864,8.45819823737484));
#17730=CARTESIAN_POINT('Ctrl Pts',(16.6326967446266,-17.0526412272871,8.43638217226655));
#17731=CARTESIAN_POINT('Ctrl Pts',(16.8296315264493,-16.8877291948126,8.42531451959006));
#17732=CARTESIAN_POINT('Ctrl Pts',(17.1395177580603,-16.4998220609018,8.40509042003568));
#17733=CARTESIAN_POINT('Ctrl Pts',(17.2531967787472,-16.2835605643862,8.39627649013066));
#17734=CARTESIAN_POINT('Ctrl Pts',(17.3950116373512,-15.8149399315971,8.37577689989492));
#17735=CARTESIAN_POINT('Ctrl Pts',(17.4198540512094,-15.5663949154174,8.36490441449773));
#17736=CARTESIAN_POINT('Ctrl Pts',(17.3726494328954,-15.0688566698042,8.34313983682436));
#17737=CARTESIAN_POINT('Ctrl Pts',(17.2991348321892,-14.824841396726,8.33246550291892));
#17738=CARTESIAN_POINT('Ctrl Pts',(17.066507698286,-14.3894725032585,8.31342049445577));
#17739=CARTESIAN_POINT('Ctrl Pts',(16.9134234150931,-14.2001966532814,8.30378297945824));
#17740=CARTESIAN_POINT('Ctrl Pts',(16.5377733451185,-13.8829872164622,8.28261380964455));
#17741=CARTESIAN_POINT('Ctrl Pts',(16.3165112992051,-13.7607430290753,8.27155778836951));
#17742=CARTESIAN_POINT('Ctrl Pts',(15.8396647684048,-13.6089185591677,8.25017224837243));
#17743=CARTESIAN_POINT('Ctrl Pts',(15.5887938715175,-13.5807136919527,8.24067632994134));
#17744=CARTESIAN_POINT('Ctrl Pts',(15.0966010032285,-13.6222926016751,8.22112073141286));
#17745=CARTESIAN_POINT('Ctrl Pts',(14.8597701187552,-13.6893089311827,8.21068286058571));
#17746=CARTESIAN_POINT('Ctrl Pts',(14.4157022868252,-13.9133101184512,8.18896043639108));
#17747=CARTESIAN_POINT('Ctrl Pts',(14.2144065933613,-14.0715222440947,8.17787411762319));
#17748=CARTESIAN_POINT('Ctrl Pts',(13.8922847111168,-14.4495722712142,8.15740208145966));
#17749=CARTESIAN_POINT('Ctrl Pts',(13.7714830508635,-14.6631148846274,8.14860914765412));
#17750=CARTESIAN_POINT('Ctrl Pts',(13.6283784023255,-15.0893069497315,8.12996557525237));
#17751=CARTESIAN_POINT('Ctrl Pts',(13.595,-15.2941185117879,8.12100618933559));
#17752=CARTESIAN_POINT('Ctrl Pts',(13.595,-15.5,8.11199999999998));
#17753=CARTESIAN_POINT('Origin',(15.5,-15.5,-1.713));
#17754=CARTESIAN_POINT('',(13.595,-15.5,7.54949999999993));
#17755=CARTESIAN_POINT('',(13.595,-15.5,7.61199999999997));
#17756=CARTESIAN_POINT('',(13.595,-15.5,-1.713));
#17757=CARTESIAN_POINT('Ctrl Pts',(13.595,-15.5,7.54949999999993));
#17758=CARTESIAN_POINT('Ctrl Pts',(13.595,-15.2929493792634,7.55855733249059));
#17759=CARTESIAN_POINT('Ctrl Pts',(13.6287585544377,-15.0869966833337,7.56756663677444));
#17760=CARTESIAN_POINT('Ctrl Pts',(13.7730330635226,-14.659900583067,7.58624975577124));
#17761=CARTESIAN_POINT('Ctrl Pts',(13.8942712821964,-14.4465216732759,7.59504406396131));
#17762=CARTESIAN_POINT('Ctrl Pts',(14.2171369312795,-14.0690784754299,7.61553100416422));
#17763=CARTESIAN_POINT('Ctrl Pts',(14.4186919319085,-13.9112790359548,7.62661812011093));
#17764=CARTESIAN_POINT('Ctrl Pts',(14.863092069992,-13.6881435985439,7.6483341974395));
#17765=CARTESIAN_POINT('Ctrl Pts',(15.1000019202232,-13.6215707720726,7.65876535937924));
#17766=CARTESIAN_POINT('Ctrl Pts',(15.5923708701065,-13.5808635018622,7.67830856382976));
#17767=CARTESIAN_POINT('Ctrl Pts',(15.8433379208265,-13.6095625320068,7.68782548676811));
#17768=CARTESIAN_POINT('Ctrl Pts',(16.3199700807978,-13.7623781380245,7.70922458395993));
#17769=CARTESIAN_POINT('Ctrl Pts',(16.5409454194786,-13.8850350400053,7.72027877065713));
#17770=CARTESIAN_POINT('Ctrl Pts',(16.915923850466,-14.2029253271881,7.741437387923));
#17771=CARTESIAN_POINT('Ctrl Pts',(17.0686294557123,-14.3924762194996,7.75105189061667));
#17772=CARTESIAN_POINT('Ctrl Pts',(17.3004182538365,-14.8282704095303,7.7701155034789));
#17773=CARTESIAN_POINT('Ctrl Pts',(17.373468436966,-15.0724279299405,7.78079605992729));
#17774=CARTESIAN_POINT('Ctrl Pts',(17.4197196437091,-15.5700126415031,7.80256267023187));
#17775=CARTESIAN_POINT('Ctrl Pts',(17.394416640621,-15.8184641689756,7.81343106600931));
#17776=CARTESIAN_POINT('Ctrl Pts',(17.251739357461,-16.2868291909747,7.8339194746707));
#17777=CARTESIAN_POINT('Ctrl Pts',(17.1376299104146,-16.502923705768,7.84272977902298));
#17778=CARTESIAN_POINT('Ctrl Pts',(16.8269990788688,-16.8902375863567,7.86296911111449));
#17779=CARTESIAN_POINT('Ctrl Pts',(16.6297938822244,-17.0547467440568,7.87403819636831));
#17780=CARTESIAN_POINT('Ctrl Pts',(16.1910433456394,-17.2920048615472,7.8958491399095));
#17781=CARTESIAN_POINT('Ctrl Pts',(15.9555300502227,-17.3658328375752,7.90638608150065));
#17782=CARTESIAN_POINT('Ctrl Pts',(15.4660857345857,-17.4207687430086,7.92612970196418));
#17783=CARTESIAN_POINT('Ctrl Pts',(15.2166577830259,-17.4000604106139,7.93534214140658));
#17784=CARTESIAN_POINT('Ctrl Pts',(14.736659339645,-17.2633485083323,7.95651654197027));
#17785=CARTESIAN_POINT('Ctrl Pts',(14.5111157371733,-17.1474800469075,7.96759531362881));
#17786=CARTESIAN_POINT('Ctrl Pts',(14.1252489758112,-16.840732545736,7.98892270507244));
#17787=CARTESIAN_POINT('Ctrl Pts',(13.9663704305421,-16.6556076801852,7.99894848293143));
#17788=CARTESIAN_POINT('Ctrl Pts',(13.7210808802104,-16.2267404176834,8.01770908059117));
#17789=CARTESIAN_POINT('Ctrl Pts',(13.6405741651424,-15.9849881593637,8.02828441997523));
#17790=CARTESIAN_POINT('Ctrl Pts',(13.5998236036108,-15.6566231870054,8.0426485919944));
#17791=CARTESIAN_POINT('Ctrl Pts',(13.595,-15.5782696639076,8.0460761301877));
#17792=CARTESIAN_POINT('Ctrl Pts',(13.595,-15.5,8.04949999999993));
#17793=CARTESIAN_POINT('Ctrl Pts',(13.595,-15.5,8.11199999999998));
#17794=CARTESIAN_POINT('Ctrl Pts',(13.595,-15.5401785671646,8.1102424073856));
#17795=CARTESIAN_POINT('Ctrl Pts',(13.5962710960814,-15.5803978824981,8.1084830322617));
#17796=CARTESIAN_POINT('Ctrl Pts',(13.6147984492805,-15.8724739282841,8.0957063023498));
#17797=CARTESIAN_POINT('Ctrl Pts',(13.6806733388295,-16.1187040113957,8.08493508261613));
#17798=CARTESIAN_POINT('Ctrl Pts',(13.8995422577313,-16.5609698965807,8.06558836847855));
#17799=CARTESIAN_POINT('Ctrl Pts',(14.0464846665982,-16.7547659878573,8.05628688580874));
#17800=CARTESIAN_POINT('Ctrl Pts',(14.4111890709962,-17.0829706259866,8.03529189026432));
#17801=CARTESIAN_POINT('Ctrl Pts',(14.6277011118655,-17.2118407447284,8.02427089345816));
#17802=CARTESIAN_POINT('Ctrl Pts',(15.1009405077996,-17.3797824410656,8.00266948544771));
#17803=CARTESIAN_POINT('Ctrl Pts',(15.3533937102224,-17.4160659498373,7.99279605189069));
#17804=CARTESIAN_POINT('Ctrl Pts',(15.8483877185811,-17.3885984573049,7.9734429839893));
#17805=CARTESIAN_POINT('Ctrl Pts',(16.086392355055,-17.3287429746659,7.96311727083424));
#17806=CARTESIAN_POINT('Ctrl Pts',(16.5356193755658,-17.1187588694243,7.94150598192568));
#17807=CARTESIAN_POINT('Ctrl Pts',(16.7409977273652,-16.9672499532929,7.93041161061722));
#17808=CARTESIAN_POINT('Ctrl Pts',(17.0750695532519,-16.5990575021999,7.909702471796));
#17809=CARTESIAN_POINT('Ctrl Pts',(17.2029358204013,-16.3881325397119,7.90085094224463));
#17810=CARTESIAN_POINT('Ctrl Pts',(17.3725337765339,-15.9279676166023,7.88072124307099));
#17811=CARTESIAN_POINT('Ctrl Pts',(17.412090442216,-15.6828552255489,7.86999891625325));
#17812=CARTESIAN_POINT('Ctrl Pts',(17.3956137144998,-15.1847415035945,7.8482091646367));
#17813=CARTESIAN_POINT('Ctrl Pts',(17.3372094330798,-14.9365988780476,7.8373542816294));
#17814=CARTESIAN_POINT('Ctrl Pts',(17.1317475349455,-14.4877852505327,7.81772113956837));
#17815=CARTESIAN_POINT('Ctrl Pts',(16.9906514017321,-14.2895661627728,7.80866338860339));
#17816=CARTESIAN_POINT('Ctrl Pts',(16.6364533234906,-13.9509993026596,7.78783976814033));
#17817=CARTESIAN_POINT('Ctrl Pts',(16.4246495253351,-13.8159724508042,7.77686247611286));
#17818=CARTESIAN_POINT('Ctrl Pts',(15.9577517677181,-13.6336642077804,7.75518708501145));
#17819=CARTESIAN_POINT('Ctrl Pts',(15.706738432325,-13.5895132845942,7.74495206001905));
#17820=CARTESIAN_POINT('Ctrl Pts',(15.2120813267271,-13.6013388582683,7.72595387950955));
#17821=CARTESIAN_POINT('Ctrl Pts',(14.9730376353124,-13.6533547357279,7.71576027285558));
#17822=CARTESIAN_POINT('Ctrl Pts',(14.5186634602065,-13.8478992469824,7.69429168868705));
#17823=CARTESIAN_POINT('Ctrl Pts',(14.3090682860259,-13.9919724974815,7.68320020265902));
#17824=CARTESIAN_POINT('Ctrl Pts',(13.9620507431484,-14.349204207856,7.66224036613768));
#17825=CARTESIAN_POINT('Ctrl Pts',(13.8263901549087,-14.5573208660807,7.6532370574768));
#17826=CARTESIAN_POINT('Ctrl Pts',(13.6422128223145,-15.0125264805873,7.63332430093671));
#17827=CARTESIAN_POINT('Ctrl Pts',(13.595,-15.2551322722671,7.62271162413527));
#17828=CARTESIAN_POINT('Ctrl Pts',(13.595,-15.5,7.61199999999997));
#17829=CARTESIAN_POINT('Origin',(15.5,-15.5,-1.713));
#17830=CARTESIAN_POINT('',(13.595,-15.5,7.04949999999992));
#17831=CARTESIAN_POINT('',(13.595,-15.5,7.11199999999996));
#17832=CARTESIAN_POINT('',(13.595,-15.5,-1.713));
#17833=CARTESIAN_POINT('Ctrl Pts',(13.595,-15.5,7.04949999999992));
#17834=CARTESIAN_POINT('Ctrl Pts',(13.595,-15.4991343357693,7.0495378680765));
#17835=CARTESIAN_POINT('Ctrl Pts',(13.5950005900588,-15.4982686422646,7.04957573743363));
#17836=CARTESIAN_POINT('Ctrl Pts',(13.5953359924214,-15.2522458300719,7.06033789019796));
#17837=CARTESIAN_POINT('Ctrl Pts',(13.6429915679965,-15.0094264327662,7.07095991107749));
#17838=CARTESIAN_POINT('Ctrl Pts',(13.8281413575464,-14.5541898043714,7.09087402430561));
#17839=CARTESIAN_POINT('Ctrl Pts',(13.9642588322537,-14.3462354806215,7.09988894990294));
#17840=CARTESIAN_POINT('Ctrl Pts',(14.3120270236143,-13.9896488844362,7.12086311378916));
#17841=CARTESIAN_POINT('Ctrl Pts',(14.5218599384075,-13.8460122470201,7.13195405663558));
#17842=CARTESIAN_POINT('Ctrl Pts',(14.9765181285096,-13.6523708761749,7.15341364666574));
#17843=CARTESIAN_POINT('Ctrl Pts',(15.2156145109008,-13.6008120471849,7.16359925277241));
#17844=CARTESIAN_POINT('Ctrl Pts',(15.7102416863387,-13.5898965411343,7.18257639417033));
#17845=CARTESIAN_POINT('Ctrl Pts',(15.9611684979088,-13.6345061488357,7.19283493915264));
#17846=CARTESIAN_POINT('Ctrl Pts',(16.4276866352902,-13.8176501538517,7.21451422877673));
#17847=CARTESIAN_POINT('Ctrl Pts',(16.639209586072,-13.9530323355161,7.22548865308526));
#17848=CARTESIAN_POINT('Ctrl Pts',(16.9927905859397,-14.2922022696668,7.2463020868235));
#17849=CARTESIAN_POINT('Ctrl Pts',(17.1335445138208,-14.4906839465111,7.25534794166705));
#17850=CARTESIAN_POINT('Ctrl Pts',(17.3382125741074,-14.939879781951,7.27499780323484));
#17851=CARTESIAN_POINT('Ctrl Pts',(17.3961740690682,-15.1881280415524,7.28585730715441));
#17852=CARTESIAN_POINT('Ctrl Pts',(17.411759261701,-15.6862300439605,7.3076465461049));
#17853=CARTESIAN_POINT('Ctrl Pts',(17.3717796671033,-15.931229923178,7.31836395114503));
#17854=CARTESIAN_POINT('Ctrl Pts',(17.2013748154031,-16.3911426119783,7.33848261644689));
#17855=CARTESIAN_POINT('Ctrl Pts',(17.0730862086873,-16.6019133458283,7.34734007234671));
#17856=CARTESIAN_POINT('Ctrl Pts',(16.738306266743,-16.9695140895441,7.36806309536767));
#17857=CARTESIAN_POINT('Ctrl Pts',(16.5326916408181,-17.1206209283353,7.37915762331326));
#17858=CARTESIAN_POINT('Ctrl Pts',(16.0831710552844,-17.3297672625767,7.40076170965258));
#17859=CARTESIAN_POINT('Ctrl Pts',(15.8451032740296,-17.3891960800257,7.41108048284215));
#17860=CARTESIAN_POINT('Ctrl Pts',(15.349945156537,-17.415819935853,7.43042131558722));
#17861=CARTESIAN_POINT('Ctrl Pts',(15.0973957888155,-17.3790480412991,7.4403198361288));
#17862=CARTESIAN_POINT('Ctrl Pts',(14.624381465431,-17.2101381010058,7.46193389520805));
#17863=CARTESIAN_POINT('Ctrl Pts',(14.4081606488506,-17.0808758006958,7.47295243720896));
#17864=CARTESIAN_POINT('Ctrl Pts',(14.0441154296759,-16.7520156512514,7.49393679777999));
#17865=CARTESIAN_POINT('Ctrl Pts',(13.8975410797082,-16.557944605115,7.50322070843755));
#17866=CARTESIAN_POINT('Ctrl Pts',(13.6795074139451,-16.1152657431494,7.52258548805109));
#17867=CARTESIAN_POINT('Ctrl Pts',(13.6140973678417,-15.8689094193862,7.53336223012298));
#17868=CARTESIAN_POINT('Ctrl Pts',(13.5961963787309,-15.5779984871332,7.54608799268872));
#17869=CARTESIAN_POINT('Ctrl Pts',(13.595,-15.5389797868994,7.54779484746714));
#17870=CARTESIAN_POINT('Ctrl Pts',(13.595,-15.5,7.54949999999993));
#17871=CARTESIAN_POINT('Ctrl Pts',(13.595,-15.5,7.61199999999997));
#17872=CARTESIAN_POINT('Ctrl Pts',(13.595,-15.5003277274783,7.61198566371483));
#17873=CARTESIAN_POINT('Ctrl Pts',(13.5950000845712,-15.5006554590083,7.6119713272525));
#17874=CARTESIAN_POINT('Ctrl Pts',(13.5951318731733,-15.756003956838,7.60080122673501));
#17875=CARTESIAN_POINT('Ctrl Pts',(13.6464713038349,-16.0084388450233,7.58975858070765));
#17876=CARTESIAN_POINT('Ctrl Pts',(13.8402272920192,-16.4656697349393,7.56975722944273));
#17877=CARTESIAN_POINT('Ctrl Pts',(13.9758927039181,-16.6681042598835,7.56085667132801));
#17878=CARTESIAN_POINT('Ctrl Pts',(14.3202774206731,-17.0161921226041,7.54019657313268));
#17879=CARTESIAN_POINT('Ctrl Pts',(14.5275609955708,-17.1567860835421,7.52926875939176));
#17880=CARTESIAN_POINT('Ctrl Pts',(14.98821042329,-17.3522284718803,7.50754280572542));
#17881=CARTESIAN_POINT('Ctrl Pts',(15.2377713581851,-17.4036653753014,7.49696342859849));
#17882=CARTESIAN_POINT('Ctrl Pts',(15.7318010893369,-17.4062280475813,7.47819161610757));
#17883=CARTESIAN_POINT('Ctrl Pts',(15.9715890158941,-17.3614766858768,7.46818242672917));
#17884=CARTESIAN_POINT('Ctrl Pts',(16.430331989696,-17.1812346610907,7.44686116332088));
#17885=CARTESIAN_POINT('Ctrl Pts',(16.6435859613336,-17.0441123582632,7.43578310084013));
#17886=CARTESIAN_POINT('Ctrl Pts',(17.0024361354668,-16.6971786416951,7.41460023884381));
#17887=CARTESIAN_POINT('Ctrl Pts',(17.1453663198282,-16.4916203149371,7.40537796653269));
#17888=CARTESIAN_POINT('Ctrl Pts',(17.343025031331,-16.0404494919582,7.38564171005943));
#17889=CARTESIAN_POINT('Ctrl Pts',(17.3971063213366,-15.7996614304134,7.37510854901198));
#17890=CARTESIAN_POINT('Ctrl Pts',(17.4115724937508,-15.3011360430778,7.35330078928601));
#17891=CARTESIAN_POINT('Ctrl Pts',(17.3680035532163,-15.0480770644475,7.34223084271425));
#17892=CARTESIAN_POINT('Ctrl Pts',(17.1884401117818,-14.5851921801101,7.32198216010981));
#17893=CARTESIAN_POINT('Ctrl Pts',(17.0585725890897,-14.378145289724,7.3131739326621));
#17894=CARTESIAN_POINT('Ctrl Pts',(16.7246962104993,-14.0200205218403,7.29269240118683));
#17895=CARTESIAN_POINT('Ctrl Pts',(16.5223738539402,-13.8736657419208,7.28182653546096));
#17896=CARTESIAN_POINT('Ctrl Pts',(16.0685961246215,-13.6644071382625,7.26005871642812));
#17897=CARTESIAN_POINT('Ctrl Pts',(15.8206918399668,-13.6053010700133,7.24937435762049));
#17898=CARTESIAN_POINT('Ctrl Pts',(15.3274201195724,-13.5875624482055,7.2302993291107));
#17899=CARTESIAN_POINT('Ctrl Pts',(15.0868812502939,-13.6247482194238,7.22069879957406));
#17900=CARTESIAN_POINT('Ctrl Pts',(14.6239355064353,-13.7899780527012,7.19954666959181));
#17901=CARTESIAN_POINT('Ctrl Pts',(14.4070929248025,-13.9197406682961,7.18849362969182));
#17902=CARTESIAN_POINT('Ctrl Pts',(14.0359738459738,-14.255689902187,7.16708622955883));
#17903=CARTESIAN_POINT('Ctrl Pts',(13.885343874168,-14.4585836779553,7.15755626955576));
#17904=CARTESIAN_POINT('Ctrl Pts',(13.6738959314522,-14.905167345095,7.1380206760676));
#17905=CARTESIAN_POINT('Ctrl Pts',(13.6128351904539,-15.1435292900942,7.12759364435285));
#17906=CARTESIAN_POINT('Ctrl Pts',(13.5961178635103,-15.4246035725244,7.11529818142939));
#17907=CARTESIAN_POINT('Ctrl Pts',(13.595,-15.4623209809862,7.11364825105044));
#17908=CARTESIAN_POINT('Ctrl Pts',(13.595,-15.5,7.11199999999997));
#17909=CARTESIAN_POINT('Origin',(15.5,-15.5,-1.713));
#17910=CARTESIAN_POINT('',(13.595,-15.5,6.54949999999991));
#17911=CARTESIAN_POINT('',(13.595,-15.5,6.61199999999996));
#17912=CARTESIAN_POINT('',(13.595,-15.5,-1.713));
#17913=CARTESIAN_POINT('Ctrl Pts',(13.595,-15.5,6.54949999999991));
#17914=CARTESIAN_POINT('Ctrl Pts',(13.595,-15.4610626456773,6.55120329633949));
#17915=CARTESIAN_POINT('Ctrl Pts',(13.5961937741644,-15.4220849065524,6.55290835929331));
#17916=CARTESIAN_POINT('Ctrl Pts',(13.6135439126654,-15.1398288859061,6.5652555168019));
#17917=CARTESIAN_POINT('Ctrl Pts',(13.6750573440076,-14.901632385016,6.57567531124154));
#17918=CARTESIAN_POINT('Ctrl Pts',(13.8874077255788,-14.455352793198,6.5951976030971));
#17919=CARTESIAN_POINT('Ctrl Pts',(14.0385487102697,-14.2526346764271,6.60475060010868));
#17920=CARTESIAN_POINT('Ctrl Pts',(14.4104722647551,-13.9174172546469,6.62617247050852));
#17921=CARTESIAN_POINT('Ctrl Pts',(14.6275426754921,-13.7881425696087,6.6372234693111));
#17922=CARTESIAN_POINT('Ctrl Pts',(15.0907593985093,-13.6239010437341,6.6583642485118));
#17923=CARTESIAN_POINT('Ctrl Pts',(15.3313513363661,-13.5872144057403,6.66794064636249));
#17924=CARTESIAN_POINT('Ctrl Pts',(15.8245674377791,-13.6059607746345,6.68703560952199));
#17925=CARTESIAN_POINT('Ctrl Pts',(16.0723530201276,-13.6655746954185,6.69772657931191));
#17926=CARTESIAN_POINT('Ctrl Pts',(16.5256592868876,-13.8757431795112,6.71949643866254));
#17927=CARTESIAN_POINT('Ctrl Pts',(16.7276463839847,-14.0224749216709,6.73035784847893));
#17928=CARTESIAN_POINT('Ctrl Pts',(17.0608214992481,-14.3812638928176,6.75082734101175));
#17929=CARTESIAN_POINT('Ctrl Pts',(17.1903023731798,-14.5886223743785,6.75963221235241));
#17930=CARTESIAN_POINT('Ctrl Pts',(17.368912415714,-15.0518806845181,6.77989723029377));
#17931=CARTESIAN_POINT('Ctrl Pts',(17.4119607652391,-15.304973303584,6.79096864845063));
#17932=CARTESIAN_POINT('Ctrl Pts',(17.3965108544052,-15.8033698669453,6.81277077283214));
#17933=CARTESIAN_POINT('Ctrl Pts',(17.3419722590831,-16.0440060481921,6.82329728994705));
#17934=CARTESIAN_POINT('Ctrl Pts',(17.1434168441495,-16.4948819322832,6.84302064445673));
#17935=CARTESIAN_POINT('Ctrl Pts',(16.9999920718481,-16.70026790681,6.85226039867485));
#17936=CARTESIAN_POINT('Ctrl Pts',(16.6403455757613,-17.0464984224452,6.87345804783543));
#17937=CARTESIAN_POINT('Ctrl Pts',(16.4268522650442,-17.1831477172723,6.88453483165137));
#17938=CARTESIAN_POINT('Ctrl Pts',(15.9678323975632,-17.3624186317035,6.90584534448146));
#17939=CARTESIAN_POINT('Ctrl Pts',(15.7279989456845,-17.4066813297663,6.91582574173733));
#17940=CARTESIAN_POINT('Ctrl Pts',(15.2340134689555,-17.403144337622,6.93461718828239));
#17941=CARTESIAN_POINT('Ctrl Pts',(14.9845514966635,-17.3512140199344,6.94520360841043));
#17942=CARTESIAN_POINT('Ctrl Pts',(14.5243302645298,-17.1548784572058,6.96693287611617));
#17943=CARTESIAN_POINT('Ctrl Pts',(14.3173601839665,-17.0139100171481,6.97785700418355));
#17944=CARTESIAN_POINT('Ctrl Pts',(13.9736471620034,-16.6651757950803,6.99850579332026));
#17945=CARTESIAN_POINT('Ctrl Pts',(13.8383527355207,-16.462449567229,7.00739809417185));
#17946=CARTESIAN_POINT('Ctrl Pts',(13.6458350057992,-16.0056519828164,7.02738049069033));
#17947=CARTESIAN_POINT('Ctrl Pts',(13.595,-15.7540869989855,7.03838508315891));
#17948=CARTESIAN_POINT('Ctrl Pts',(13.595,-15.5,7.04949999999992));
#17949=CARTESIAN_POINT('Ctrl Pts',(13.595,-15.5,7.11199999999997));
#17950=CARTESIAN_POINT('Ctrl Pts',(13.595,-15.7151084711071,7.10259018061645));
#17951=CARTESIAN_POINT('Ctrl Pts',(13.6314375584287,-15.9289657393821,7.09323509451523));
#17952=CARTESIAN_POINT('Ctrl Pts',(13.7837888964782,-16.3618713020821,7.0742978433035));
#17953=CARTESIAN_POINT('Ctrl Pts',(13.9077406040965,-16.5737379336832,7.06550254240705));
#17954=CARTESIAN_POINT('Ctrl Pts',(14.2308903575243,-16.9419485720183,7.04520677622757));
#17955=CARTESIAN_POINT('Ctrl Pts',(14.4280313004595,-17.0939658080948,7.03441335178549));
#17956=CARTESIAN_POINT('Ctrl Pts',(14.8744284026619,-17.3169710492469,7.0126244694032));
#17957=CARTESIAN_POINT('Ctrl Pts',(15.1204083881536,-17.3837876812905,7.00184436300425));
#17958=CARTESIAN_POINT('Ctrl Pts',(15.6127593154075,-17.4168741618687,6.98246852525851));
#17959=CARTESIAN_POINT('Ctrl Pts',(15.8541502591357,-17.3872519912577,6.97319522635436));
#17960=CARTESIAN_POINT('Ctrl Pts',(16.3211196205183,-17.236959840026,6.95221738709966));
#17961=CARTESIAN_POINT('Ctrl Pts',(16.5412928197739,-17.1146128808544,6.94120036770448));
#17962=CARTESIAN_POINT('Ctrl Pts',(16.9245245713851,-16.7898416281419,6.9195785803559));
#17963=CARTESIAN_POINT('Ctrl Pts',(17.082933253164,-16.5896119800978,6.90966456605852));
#17964=CARTESIAN_POINT('Ctrl Pts',(17.3079526732748,-16.1476518931442,6.89033122892145));
#17965=CARTESIAN_POINT('Ctrl Pts',(17.375764904958,-15.9118621302026,6.88001671610686));
#17966=CARTESIAN_POINT('Ctrl Pts',(17.4199326181634,-15.4180941903735,6.85841706869526));
#17967=CARTESIAN_POINT('Ctrl Pts',(17.3921628352553,-15.164471498879,6.84732246276811));
#17968=CARTESIAN_POINT('Ctrl Pts',(17.2417314993585,-14.6905493102034,6.82659095845158));
#17969=CARTESIAN_POINT('Ctrl Pts',(17.1235538851641,-14.4738860201229,6.81772974273954));
#17970=CARTESIAN_POINT('Ctrl Pts',(16.8108405892163,-14.0960047381003,6.7976178311296));
#17971=CARTESIAN_POINT('Ctrl Pts',(16.6188433475139,-13.9386922264281,6.78690345035065));
#17972=CARTESIAN_POINT('Ctrl Pts',(16.1799611386208,-13.7026704139082,6.7651145593432));
#17973=CARTESIAN_POINT('Ctrl Pts',(15.9360709048723,-13.6284758145378,6.75425224797636));
#17974=CARTESIAN_POINT('Ctrl Pts',(15.4447624444838,-13.5805885181933,6.73459217553703));
#17975=CARTESIAN_POINT('Ctrl Pts',(15.2024607337532,-13.6029827990872,6.72555345744808));
#17976=CARTESIAN_POINT('Ctrl Pts',(14.7318101012877,-13.7390972895958,6.70474625494253));
#17977=CARTESIAN_POINT('Ctrl Pts',(14.5087023988878,-13.854333231983,6.69377359924472));
#17978=CARTESIAN_POINT('Ctrl Pts',(14.1165104476134,-14.1663212633333,6.67209196282133));
#17979=CARTESIAN_POINT('Ctrl Pts',(13.9521980321027,-14.3611392816342,6.66181892906235));
#17980=CARTESIAN_POINT('Ctrl Pts',(13.7138657210454,-14.7946622708063,6.64285466881861));
#17981=CARTESIAN_POINT('Ctrl Pts',(13.6387111132089,-15.0273931336094,6.63267396615881));
#17982=CARTESIAN_POINT('Ctrl Pts',(13.5997187869975,-15.345083827799,6.61877673544186));
#17983=CARTESIAN_POINT('Ctrl Pts',(13.595,-15.4225853386876,6.61538646812386));
#17984=CARTESIAN_POINT('Ctrl Pts',(13.595,-15.5,6.61199999999996));
#17985=CARTESIAN_POINT('Origin',(15.5,-15.5,-1.713));
#17986=CARTESIAN_POINT('',(13.595,-15.5000000000007,6.04949999999984));
#17987=CARTESIAN_POINT('',(13.595,-15.5,6.11199999999995));
#17988=CARTESIAN_POINT('',(13.595,-15.5,-1.713));
#17989=CARTESIAN_POINT('Ctrl Pts',(13.595,-15.5000000000014,6.04949999999984));
#17990=CARTESIAN_POINT('Ctrl Pts',(13.5949999999999,-15.4212996333131,6.05294271070362));
#17991=CARTESIAN_POINT('Ctrl Pts',(13.5998768365782,-15.3425152813848,6.05638909525989));
#17992=CARTESIAN_POINT('Ctrl Pts',(13.6396656510538,-15.0236734792597,6.07033668065492));
#17993=CARTESIAN_POINT('Ctrl Pts',(13.7152677517337,-14.791138118477,6.08050883121264));
#17994=CARTESIAN_POINT('Ctrl Pts',(13.9544193128816,-14.3581281491297,6.09945064964428));
#17995=CARTESIAN_POINT('Ctrl Pts',(14.1191066045505,-14.1636342658724,6.1097490860317));
#17996=CARTESIAN_POINT('Ctrl Pts',(14.5118631593489,-13.8524405146268,6.13143473911924));
#17997=CARTESIAN_POINT('Ctrl Pts',(14.7351471528063,-13.7376518540051,6.14240429033984));
#17998=CARTESIAN_POINT('Ctrl Pts',(15.2060239795073,-13.6024250338468,6.16320064659774));
#17999=CARTESIAN_POINT('Ctrl Pts',(15.4483861027075,-13.5804852546147,6.17222719514705));
#18000=CARTESIAN_POINT('Ctrl Pts',(15.9396234792267,-13.6293069089211,6.19190501117974));
#18001=CARTESIAN_POINT('Ctrl Pts',(16.1833741630851,-13.7039650529646,6.20277217462826));
#18002=CARTESIAN_POINT('Ctrl Pts',(16.6217691980785,-13.9408001486887,6.2245603979467));
#18003=CARTESIAN_POINT('Ctrl Pts',(16.8134370968083,-14.0984413002525,6.23526949003646));
#18004=CARTESIAN_POINT('Ctrl Pts',(17.1254884498018,-14.4769312778602,6.25536963823337));
#18005=CARTESIAN_POINT('Ctrl Pts',(17.2432989432679,-14.6939024955189,6.2642376419736));
#18006=CARTESIAN_POINT('Ctrl Pts',(17.3928068238889,-15.1681616774429,6.28498388790203));
#18007=CARTESIAN_POINT('Ctrl Pts',(17.4200800648353,-15.4217867335681,6.29607859726884));
#18008=CARTESIAN_POINT('Ctrl Pts',(17.3749840443236,-15.9153766743346,6.31767045819477));
#18009=CARTESIAN_POINT('Ctrl Pts',(17.3067452371384,-16.150996284795,6.32797752776871));
#18010=CARTESIAN_POINT('Ctrl Pts',(17.0808598623415,-16.5926576436372,6.34729779718439));
#18011=CARTESIAN_POINT('Ctrl Pts',(16.9219479764644,-16.7927154491698,6.357239048736));
#18012=CARTESIAN_POINT('Ctrl Pts',(16.5379425112565,-17.1167607502192,6.37887426914662));
#18013=CARTESIAN_POINT('Ctrl Pts',(16.3175639018305,-17.2386290144578,6.38988860013231));
#18014=CARTESIAN_POINT('Ctrl Pts',(15.8503415097167,-17.3879626090542,6.41085505936614));
#18015=CARTESIAN_POINT('Ctrl Pts',(15.608892168395,-17.4170977909834,6.42011013650055));
#18016=CARTESIAN_POINT('Ctrl Pts',(15.1166063757536,-17.3830178532379,6.43950523585411));
#18017=CARTESIAN_POINT('Ctrl Pts',(14.870759502855,-17.3157040667844,6.4502911733256));
#18018=CARTESIAN_POINT('Ctrl Pts',(14.4248547550533,-17.0918174858598,6.47208068031278));
#18019=CARTESIAN_POINT('Ctrl Pts',(14.2280546533922,-16.9394396391344,6.48286907973836));
#18020=CARTESIAN_POINT('Ctrl Pts',(13.9056026551441,-16.5705783121195,6.50315264428303));
#18021=CARTESIAN_POINT('Ctrl Pts',(13.7820360793138,-16.3583941382296,6.51194995020858));
#18022=CARTESIAN_POINT('Ctrl Pts',(13.630989180424,-15.9263442702941,6.53084976945334));
#18023=CARTESIAN_POINT('Ctrl Pts',(13.595,-15.7137808200968,6.54014825808841));
#18024=CARTESIAN_POINT('Ctrl Pts',(13.595,-15.5,6.54949999999991));
#18025=CARTESIAN_POINT('Ctrl Pts',(13.595,-15.5,6.61199999999996));
#18026=CARTESIAN_POINT('Ctrl Pts',(13.595,-15.6733284920729,6.60441782624349));
#18027=CARTESIAN_POINT('Ctrl Pts',(13.6186572328438,-15.8462216114541,6.59685469766167));
#18028=CARTESIAN_POINT('Ctrl Pts',(13.7320473190416,-16.2510329369089,6.57914641570826));
#18029=CARTESIAN_POINT('Ctrl Pts',(13.8438568570137,-16.4730835714652,6.57012424533666));
#18030=CARTESIAN_POINT('Ctrl Pts',(14.1451247601535,-16.8614120171819,6.55021742642492));
#18031=CARTESIAN_POINT('Ctrl Pts',(14.3313806311313,-17.0242843089789,6.53959894603257));
#18032=CARTESIAN_POINT('Ctrl Pts',(14.7638243009585,-17.275405367102,6.51772371712454));
#18033=CARTESIAN_POINT('Ctrl Pts',(15.0077751382723,-17.3578889533404,6.50667781093437));
#18034=CARTESIAN_POINT('Ctrl Pts',(15.5004085561524,-17.4202581848602,6.48665079123196));
#18035=CARTESIAN_POINT('Ctrl Pts',(15.7436629817923,-17.4047379468316,6.47776337013216));
#18036=CARTESIAN_POINT('Ctrl Pts',(16.2176685098711,-17.2819927315602,6.45712148752121));
#18037=CARTESIAN_POINT('Ctrl Pts',(16.443337539286,-17.1735154737238,6.44619962657462));
#18038=CARTESIAN_POINT('Ctrl Pts',(16.8438200723545,-16.8736189807942,6.42446838012343));
#18039=CARTESIAN_POINT('Ctrl Pts',(17.0137541208759,-16.6837468325642,6.41387768558701));
#18040=CARTESIAN_POINT('Ctrl Pts',(17.2643108649679,-16.258032038322,6.39507427777451));
#18041=CARTESIAN_POINT('Ctrl Pts',(17.3461668124714,-16.0283235145553,6.38511126485366));
#18042=CARTESIAN_POINT('Ctrl Pts',(17.4210201547905,-15.5413152243351,6.36380731515024));
#18043=CARTESIAN_POINT('Ctrl Pts',(17.4097474835946,-15.2881182828737,6.35273133345901));
#18044=CARTESIAN_POINT('Ctrl Pts',(17.2903402726451,-14.803334467194,6.33152469235316));
#18045=CARTESIAN_POINT('Ctrl Pts',(17.1844249027143,-14.5762233150762,6.32227412134972));
#18046=CARTESIAN_POINT('Ctrl Pts',(16.893661371229,-14.1784483926715,6.3025586328999));
#18047=CARTESIAN_POINT('Ctrl Pts',(16.7127531792213,-14.01070398294,6.29203617905489));
#18048=CARTESIAN_POINT('Ctrl Pts',(16.2892221203122,-13.7476468776041,6.27023752599387));
#18049=CARTESIAN_POINT('Ctrl Pts',(16.0486544659216,-13.6580970861074,6.25916523396503));
#18050=CARTESIAN_POINT('Ctrl Pts',(15.5582496795982,-13.5805324739975,6.23889028605827));
#18051=CARTESIAN_POINT('Ctrl Pts',(15.3138847564439,-13.5886882666418,6.23008728511492));
#18052=CARTESIAN_POINT('Ctrl Pts',(14.8364404563567,-13.6972603894447,6.20962512613989));
#18053=CARTESIAN_POINT('Ctrl Pts',(14.6082773598722,-13.7985291079087,6.19876644735625));
#18054=CARTESIAN_POINT('Ctrl Pts',(14.1992779535143,-14.0854940002442,6.17699539214162));
#18055=CARTESIAN_POINT('Ctrl Pts',(14.0235269280418,-14.2700582652036,6.16630042340671));
#18056=CARTESIAN_POINT('Ctrl Pts',(13.7601702895471,-14.6874866951327,6.14719334754687));
#18057=CARTESIAN_POINT('Ctrl Pts',(13.6713668820483,-14.914065163743,6.13763144515555));
#18058=CARTESIAN_POINT('Ctrl Pts',(13.6057278858963,-15.2665198483617,6.12221347994914));
#18059=CARTESIAN_POINT('Ctrl Pts',(13.595,-15.3832758813928,6.11710604193377));
#18060=CARTESIAN_POINT('Ctrl Pts',(13.595,-15.5,6.11199999999995));
#18061=CARTESIAN_POINT('Origin',(15.5,-15.5,-1.713));
#18062=CARTESIAN_POINT('',(13.595,-15.5,5.5494999999999));
#18063=CARTESIAN_POINT('',(13.595,-15.5,5.61199999999994));
#18064=CARTESIAN_POINT('',(13.595,-15.5,-1.713));
#18065=CARTESIAN_POINT('Ctrl Pts',(13.595,-15.5,5.5494999999999));
#18066=CARTESIAN_POINT('Ctrl Pts',(13.595,-15.3804229784334,5.55473084083833));
#18067=CARTESIAN_POINT('Ctrl Pts',(13.6062587391732,-15.2608257903983,5.55996256384943));
#18068=CARTESIAN_POINT('Ctrl Pts',(13.6760576354803,-14.8951700410971,5.57595800345141));
#18069=CARTESIAN_POINT('Ctrl Pts',(13.7720096984448,-14.659399845156,5.58575619329743));
#18070=CARTESIAN_POINT('Ctrl Pts',(14.0452839613624,-14.2461894092018,5.6051467301244));
#18071=CARTESIAN_POINT('Ctrl Pts',(14.2171584892425,-14.0708266465022,5.61549358440075));
#18072=CARTESIAN_POINT('Ctrl Pts',(14.6253952287875,-13.7888522129699,5.63712659419822));
#18073=CARTESIAN_POINT('Ctrl Pts',(14.8599977473058,-13.6879934063342,5.6482202575467));
#18074=CARTESIAN_POINT('Ctrl Pts',(15.3463800940963,-13.5855686749737,5.66888656699346));
#18075=CARTESIAN_POINT('Ctrl Pts',(15.5927427947672,-13.5816559429033,5.67772159176443));
#18076=CARTESIAN_POINT('Ctrl Pts',(16.0754846316176,-13.667400719653,5.69788515618075));
#18077=CARTESIAN_POINT('Ctrl Pts',(16.3071807117551,-13.7569999255946,5.70862243939717));
#18078=CARTESIAN_POINT('Ctrl Pts',(16.7289712752251,-14.0227167140848,5.73041332904226));
#18079=CARTESIAN_POINT('Ctrl Pts',(16.9136998866891,-14.1983819978148,5.74125376264675));
#18080=CARTESIAN_POINT('Ctrl Pts',(17.1974101361019,-14.6022492014921,5.76083529742995));
#18081=CARTESIAN_POINT('Ctrl Pts',(17.2972979319089,-14.8240619808842,5.76993140773759));
#18082=CARTESIAN_POINT('Ctrl Pts',(17.410842370381,-15.3008057952467,5.79078634274907));
#18083=CARTESIAN_POINT('Ctrl Pts',(17.4204935309802,-15.5519439892812,5.80177226549774));
#18084=CARTESIAN_POINT('Ctrl Pts',(17.342110451467,-16.0471583288573,5.82343518498926));
#18085=CARTESIAN_POINT('Ctrl Pts',(17.2534824024277,-16.286136426886,5.83359920856734));
#18086=CARTESIAN_POINT('Ctrl Pts',(16.9934395803382,-16.7072759792659,5.85266191487493));
#18087=CARTESIAN_POINT('Ctrl Pts',(16.8277337075192,-16.8874355430668,5.86287999349777));
#18088=CARTESIAN_POINT('Ctrl Pts',(16.4300989084042,-17.181502621719,5.88437585424967));
#18089=CARTESIAN_POINT('Ctrl Pts',(16.1997352103395,-17.2896684655832,5.89546875611168));
#18090=CARTESIAN_POINT('Ctrl Pts',(15.7162942946846,-17.4085782046526,5.91638419721932));
#18091=CARTESIAN_POINT('Ctrl Pts',(15.468499068742,-17.4205357017102,5.92535357637161));
#18092=CARTESIAN_POINT('Ctrl Pts',(14.982450960336,-17.3496956343957,5.94531639540041));
#18093=CARTESIAN_POINT('Ctrl Pts',(14.7487719351981,-17.2677308223166,5.95596181876614));
#18094=CARTESIAN_POINT('Ctrl Pts',(14.3192639573802,-17.0161183157408,5.97773658137359));
#18095=CARTESIAN_POINT('Ctrl Pts',(14.1289503778061,-16.8464743447295,5.9886568954638));
#18096=CARTESIAN_POINT('Ctrl Pts',(13.8321327423216,-16.4516128328056,6.00853801394947));
#18097=CARTESIAN_POINT('Ctrl Pts',(13.7250521360265,-16.2327453046096,6.01744639962329));
#18098=CARTESIAN_POINT('Ctrl Pts',(13.617339209274,-15.8364783055986,6.03478091401572));
#18099=CARTESIAN_POINT('Ctrl Pts',(13.5950000000001,-15.6684314912174,6.04213204325374));
#18100=CARTESIAN_POINT('Ctrl Pts',(13.595,-15.5000000000014,6.04949999999984));
#18101=CARTESIAN_POINT('Ctrl Pts',(13.595,-15.5,6.11199999999995));
#18102=CARTESIAN_POINT('Ctrl Pts',(13.595,-15.6322811156622,6.10621342451166));
#18103=CARTESIAN_POINT('Ctrl Pts',(13.6087783153306,-15.7645212428739,6.10042864204396));
#18104=CARTESIAN_POINT('Ctrl Pts',(13.6882026227428,-16.1396868723561,6.08401719718472));
#18105=CARTESIAN_POINT('Ctrl Pts',(13.7879432930104,-16.3721536353157,6.07445003434073));
#18106=CARTESIAN_POINT('Ctrl Pts',(14.0727367572805,-16.7867289243291,6.05459325308234));
#18107=CARTESIAN_POINT('Ctrl Pts',(14.2556056457461,-16.964313169297,6.043781300895));
#18108=CARTESIAN_POINT('Ctrl Pts',(14.6747839923046,-17.2345693802169,6.02199008469658));
#18109=CARTESIAN_POINT('Ctrl Pts',(14.9057817799496,-17.3266442004838,6.01122510821138));
#18110=CARTESIAN_POINT('Ctrl Pts',(15.3874249059554,-17.417224156811,5.99099741088668));
#18111=CARTESIAN_POINT('Ctrl Pts',(15.6333450122464,-17.4158917348987,5.98218660102253));
#18112=CARTESIAN_POINT('Ctrl Pts',(16.1206259002119,-17.318772490929,5.96160229438465));
#18113=CARTESIAN_POINT('Ctrl Pts',(16.3565452350119,-17.2202990011103,5.95051091721535));
#18114=CARTESIAN_POINT('Ctrl Pts',(16.7681176293856,-16.9422948126497,5.92883837814036));
#18115=CARTESIAN_POINT('Ctrl Pts',(16.9419481430325,-16.7685197996487,5.91845215122558));
#18116=CARTESIAN_POINT('Ctrl Pts',(17.2189872203211,-16.3586015615324,5.89899099646484));
#18117=CARTESIAN_POINT('Ctrl Pts',(17.3171025973776,-16.1247187974314,5.88932803138367));
#18118=CARTESIAN_POINT('Ctrl Pts',(17.4166878372089,-15.6335097383612,5.86784032101315));
#18119=CARTESIAN_POINT('Ctrl Pts',(17.4176502390534,-15.3811120576987,5.85679930261146));
#18120=CARTESIAN_POINT('Ctrl Pts',(17.3237377628468,-14.8990312316065,5.83571090251993));
#18121=CARTESIAN_POINT('Ctrl Pts',(17.2331048196069,-14.6732587208355,5.82624068948459));
#18122=CARTESIAN_POINT('Ctrl Pts',(16.9663803747131,-14.2580406281809,5.80705437314968));
#18123=CARTESIAN_POINT('Ctrl Pts',(16.7891198766685,-14.0749102807301,5.79633358276825));
#18124=CARTESIAN_POINT('Ctrl Pts',(16.3779387565676,-13.7914042355473,5.77455552860573));
#18125=CARTESIAN_POINT('Ctrl Pts',(16.1491538474421,-13.6920495639437,5.76371515769118));
#18126=CARTESIAN_POINT('Ctrl Pts',(15.6708189064625,-13.5872293846082,5.74330132129251));
#18127=CARTESIAN_POINT('Ctrl Pts',(15.426142783217,-13.5810384099919,5.73450737397273));
#18128=CARTESIAN_POINT('Ctrl Pts',(14.9363614071728,-13.6626564055833,5.71416738658206));
#18129=CARTESIAN_POINT('Ctrl Pts',(14.6967303705424,-13.7540722981582,5.70308976140513));
#18130=CARTESIAN_POINT('Ctrl Pts',(14.2756337788508,-14.0202670563068,5.68131470782129));
#18131=CARTESIAN_POINT('Ctrl Pts',(14.0961750870679,-14.1892841101539,5.67081933105237));
#18132=CARTESIAN_POINT('Ctrl Pts',(13.8082370891342,-14.5895773327889,5.65115580383265));
#18133=CARTESIAN_POINT('Ctrl Pts',(13.7039174596371,-14.8180681428012,5.64183078990369));
#18134=CARTESIAN_POINT('Ctrl Pts',(13.6121927841121,-15.20462306897,5.62492112559185));
#18135=CARTESIAN_POINT('Ctrl Pts',(13.595,-15.3522360348498,5.61846386549207));
#18136=CARTESIAN_POINT('Ctrl Pts',(13.595,-15.5,5.61199999999994));
#18137=CARTESIAN_POINT('Origin',(15.5,-15.5,-1.713));
#18138=CARTESIAN_POINT('',(13.595,-15.5,5.04949999999989));
#18139=CARTESIAN_POINT('',(13.595,-15.5,5.11199999999994));
#18140=CARTESIAN_POINT('',(13.595,-15.5,-1.713));
#18141=CARTESIAN_POINT('Ctrl Pts',(13.595,-15.5,5.04949999999989));
#18142=CARTESIAN_POINT('Ctrl Pts',(13.595,-15.3388115089796,5.05655111509265));
#18143=CARTESIAN_POINT('Ctrl Pts',(13.6154590374407,-15.1779059102152,5.06358985519597));
#18144=CARTESIAN_POINT('Ctrl Pts',(13.7183515548725,-14.7816733255799,5.08092286414765));
#18145=CARTESIAN_POINT('Ctrl Pts',(13.8266134541381,-14.5565840536403,5.09007360954104));
#18146=CARTESIAN_POINT('Ctrl Pts',(14.1215467805684,-14.1625430065832,5.10986539767052));
#18147=CARTESIAN_POINT('Ctrl Pts',(14.304585872829,-13.9967060878679,5.1204268571255));
#18148=CARTESIAN_POINT('Ctrl Pts',(14.7316815678331,-13.7383361116675,5.14225803428301));
#18149=CARTESIAN_POINT('Ctrl Pts',(14.9736111872449,-13.6515671979833,5.15332109872661));
#18150=CARTESIAN_POINT('Ctrl Pts',(15.4649173561457,-13.580010626106,5.17349878504518));
#18151=CARTESIAN_POINT('Ctrl Pts',(15.7088324857421,-13.5910780271475,5.18232560154669));
#18152=CARTESIAN_POINT('Ctrl Pts',(16.1849362774886,-13.7052334734392,5.20285909680639));
#18153=CARTESIAN_POINT('Ctrl Pts',(16.4121442114176,-13.8093464029553,5.21374379967087));
#18154=CARTESIAN_POINT('Ctrl Pts',(16.8178401514487,-14.1014316240207,5.23550169996886));
#18155=CARTESIAN_POINT('Ctrl Pts',(16.9913210625043,-14.2881077192111,5.24615685848334));
#18156=CARTESIAN_POINT('Ctrl Pts',(17.2496499625203,-14.7088122754508,5.26514512042844));
#18157=CARTESIAN_POINT('Ctrl Pts',(17.3357238111982,-14.9366074284007,5.27485465566038));
#18158=CARTESIAN_POINT('Ctrl Pts',(17.4197865213486,-15.4212669482105,5.29605585950158));
#18159=CARTESIAN_POINT('Ctrl Pts',(17.4134942607844,-15.674129498803,5.30711721342076));
#18160=CARTESIAN_POINT('Ctrl Pts',(17.303614738454,-16.1620531754266,5.32846120627395));
#18161=CARTESIAN_POINT('Ctrl Pts',(17.2014486992905,-16.3924111516025,5.3378949159657));
#18162=CARTESIAN_POINT('Ctrl Pts',(16.9173100980276,-16.7960756528741,5.35748824481634));
#18163=CARTESIAN_POINT('Ctrl Pts',(16.7398070669348,-16.9667785935818,5.36794640774411));
#18164=CARTESIAN_POINT('Ctrl Pts',(16.3220071965648,-17.2371432267537,5.38968777336196));
#18165=CARTESIAN_POINT('Ctrl Pts',(16.0836525717957,-17.3310448981499,5.40077141272581));
#18166=CARTESIAN_POINT('Ctrl Pts',(15.5947256536311,-17.4180907622543,5.42119774972392));
#18167=CARTESIAN_POINT('Ctrl Pts',(15.3496232410368,-17.4145320800743,5.42998836628871));
#18168=CARTESIAN_POINT('Ctrl Pts',(14.8701126178109,-17.3147175905374,5.45033725630913));
#18169=CARTESIAN_POINT('Ctrl Pts',(14.6405232658285,-17.2179194954329,5.46115218451594));
#18170=CARTESIAN_POINT('Ctrl Pts',(14.2264796200393,-16.9390496379886,5.4829372783152));
#18171=CARTESIAN_POINT('Ctrl Pts',(14.0472256745101,-16.7578504143529,5.49369135016012));
#18172=CARTESIAN_POINT('Ctrl Pts',(13.7760216724758,-16.3455924692783,5.51298262434675));
#18173=CARTESIAN_POINT('Ctrl Pts',(13.6829531189867,-16.1208809938508,5.52233985153742));
#18174=CARTESIAN_POINT('Ctrl Pts',(13.6080918026188,-15.7578640712236,5.53821985690169));
#18175=CARTESIAN_POINT('Ctrl Pts',(13.595,-15.6289437604014,5.54385941555539));
#18176=CARTESIAN_POINT('Ctrl Pts',(13.595,-15.5,5.5494999999999));
#18177=CARTESIAN_POINT('Ctrl Pts',(13.595,-15.5,5.61199999999994));
#18178=CARTESIAN_POINT('Ctrl Pts',(13.595,-15.6018657066951,5.60754393234049));
#18179=CARTESIAN_POINT('Ctrl Pts',(13.6031704055488,-15.7038031752657,5.60308472549142));
#18180=CARTESIAN_POINT('Ctrl Pts',(13.6581997788096,-16.0432791052309,5.5882345098324));
#18181=CARTESIAN_POINT('Ctrl Pts',(13.7418506174913,-16.2721685073446,5.57838310477812));
#18182=CARTESIAN_POINT('Ctrl Pts',(13.9957147777142,-16.6957591219942,5.55950085984424));
#18183=CARTESIAN_POINT('Ctrl Pts',(14.1671636173094,-16.8842814200629,5.54888230343246));
#18184=CARTESIAN_POINT('Ctrl Pts',(14.5698803024982,-17.1808694560447,5.52713878208984));
#18185=CARTESIAN_POINT('Ctrl Pts',(14.7962133781878,-17.2874944048164,5.5162322786931));
#18186=CARTESIAN_POINT('Ctrl Pts',(15.2711157138763,-17.4065903198754,5.49563623999878));
#18187=CARTESIAN_POINT('Ctrl Pts',(15.5146461896474,-17.420222559271,5.4867780974336));
#18188=CARTESIAN_POINT('Ctrl Pts',(16.0067243777368,-17.3539584279855,5.46668692170409));
#18189=CARTESIAN_POINT('Ctrl Pts',(16.2498274691176,-17.2696533893205,5.45563329212373));
#18190=CARTESIAN_POINT('Ctrl Pts',(16.6800192677288,-17.0154474103198,5.43377589861552));
#18191=CARTESIAN_POINT('Ctrl Pts',(16.8649176699945,-16.8513113361359,5.42318120261494));
#18192=CARTESIAN_POINT('Ctrl Pts',(17.16350620977,-16.4605606452633,5.4033229083822));
#18193=CARTESIAN_POINT('Ctrl Pts',(17.2738175281523,-16.2372296372666,5.39424976540973));
#18194=CARTESIAN_POINT('Ctrl Pts',(17.4043803380836,-15.756240748363,5.37320913159943));
#18195=CARTESIAN_POINT('Ctrl Pts',(17.4215384742162,-15.5027722235257,5.36212126962054));
#18196=CARTESIAN_POINT('Ctrl Pts',(17.357600920214,-15.0131883429537,5.34070465192272));
#18197=CARTESIAN_POINT('Ctrl Pts',(17.2807387247273,-14.7812092050215,5.33055683311553));
#18198=CARTESIAN_POINT('Ctrl Pts',(17.0392813406235,-14.3496550077741,5.311678696753));
#18199=CARTESIAN_POINT('Ctrl Pts',(16.8735395704595,-14.1560794282237,5.30130708115627));
#18200=CARTESIAN_POINT('Ctrl Pts',(16.4791980485955,-13.847132194246,5.27961051979625));
#18201=CARTESIAN_POINT('Ctrl Pts',(16.2554212933711,-13.7336070322138,5.26864993642719));
#18202=CARTESIAN_POINT('Ctrl Pts',(15.7839087786619,-13.6008853677485,5.24788429127527));
#18203=CARTESIAN_POINT('Ctrl Pts',(15.5413739862863,-13.5802296539214,5.23889046790109));
#18204=CARTESIAN_POINT('Ctrl Pts',(15.0503410554409,-13.6316931270879,5.2191626144982));
#18205=CARTESIAN_POINT('Ctrl Pts',(14.8069898013851,-13.7076603642555,5.20828195016578));
#18206=CARTESIAN_POINT('Ctrl Pts',(14.3699802854607,-13.9467893376302,5.18649604337778));
#18207=CARTESIAN_POINT('Ctrl Pts',(14.1792464667997,-14.1053559943617,5.17580209496627));
#18208=CARTESIAN_POINT('Ctrl Pts',(13.8690687315096,-14.4855658574476,5.15573530887737));
#18209=CARTESIAN_POINT('Ctrl Pts',(13.7522980475817,-14.7034110952668,5.14684640878099));
#18210=CARTESIAN_POINT('Ctrl Pts',(13.6235390607378,-15.1199647574862,5.12862446380201));
#18211=CARTESIAN_POINT('Ctrl Pts',(13.595,-15.3096276017258,5.1203277514555));
#18212=CARTESIAN_POINT('Ctrl Pts',(13.595,-15.5,5.11199999999994));
#18213=CARTESIAN_POINT('Origin',(15.5,-15.5,-1.713));
#18214=CARTESIAN_POINT('',(13.595,-15.5,4.54949999999989));
#18215=CARTESIAN_POINT('',(13.595,-15.5,4.61199999999993));
#18216=CARTESIAN_POINT('',(13.595,-15.5,-1.713));
#18217=CARTESIAN_POINT('Ctrl Pts',(13.595,-15.5,4.54949999999989));
#18218=CARTESIAN_POINT('Ctrl Pts',(13.595,-15.2971397602935,4.55837402623377));
#18219=CARTESIAN_POINT('Ctrl Pts',(13.6274062319185,-15.0952396842029,4.56720605055957));
#18220=CARTESIAN_POINT('Ctrl Pts',(13.7678871857877,-14.6703239363409,4.58579379106097));
#18221=CARTESIAN_POINT('Ctrl Pts',(13.8882844780646,-14.4555148301993,4.59462055989613));
#18222=CARTESIAN_POINT('Ctrl Pts',(14.2050042984144,-14.0813297617617,4.61480340961284));
#18223=CARTESIAN_POINT('Ctrl Pts',(14.3989873176053,-13.926024873821,4.62554910805958));
#18224=CARTESIAN_POINT('Ctrl Pts',(14.8407918880583,-13.6949572788758,4.64734034948534));
#18225=CARTESIAN_POINT('Ctrl Pts',(15.0855091254695,-13.6235798401537,4.65817237326937));
#18226=CARTESIAN_POINT('Ctrl Pts',(15.5772351323095,-13.5813592039928,4.67772432128798));
#18227=CARTESIAN_POINT('Ctrl Pts',(15.8191778495975,-13.606514183194,4.68684353533109));
#18228=CARTESIAN_POINT('Ctrl Pts',(16.2884411473533,-13.7480307581005,4.70771633604734));
#18229=CARTESIAN_POINT('Ctrl Pts',(16.5104570271441,-13.8659837151826,4.71870705654094));
#18230=CARTESIAN_POINT('Ctrl Pts',(16.9007548492801,-14.1840692972141,4.7404503032613));
#18231=CARTESIAN_POINT('Ctrl Pts',(17.0637885719494,-14.3827202135971,4.75062511870481));
#18232=CARTESIAN_POINT('Ctrl Pts',(17.2967139942101,-14.8219362333497,4.76983841790658));
#18233=CARTESIAN_POINT('Ctrl Pts',(17.3684012078891,-15.0561463292249,4.78008382892474));
#18234=CARTESIAN_POINT('Ctrl Pts',(17.4210143756365,-15.5482282622774,4.80160972275907));
#18235=CARTESIAN_POINT('Ctrl Pts',(17.3977682372132,-15.8018378108878,4.8127037537569));
#18236=CARTESIAN_POINT('Ctrl Pts',(17.2557713716644,-16.2788072810669,4.83356855997647));
#18237=CARTESIAN_POINT('Ctrl Pts',(17.1409407810477,-16.4982903817682,4.84250300911577));
#18238=CARTESIAN_POINT('Ctrl Pts',(16.8342535452258,-16.8816925438905,4.86250738436947));
#18239=CARTESIAN_POINT('Ctrl Pts',(16.6452670974676,-17.041964810415,4.87317244114951));
#18240=CARTESIAN_POINT('Ctrl Pts',(16.2108643087021,-17.2853350570797,4.89495236126665));
#18241=CARTESIAN_POINT('Ctrl Pts',(15.9682744977844,-17.3637292576169,4.90585726236999));
#18242=CARTESIAN_POINT('Ctrl Pts',(15.4776352951499,-17.4201030864084,4.92567760042641));
#18243=CARTESIAN_POINT('Ctrl Pts',(15.2347723103959,-17.4018304096479,4.93461717900942));
#18244=CARTESIAN_POINT('Ctrl Pts',(14.7620931614237,-17.2737469265487,4.95532557325259));
#18245=CARTESIAN_POINT('Ctrl Pts',(14.5374226942709,-17.1625655212275,4.96626875062334));
#18246=CARTESIAN_POINT('Ctrl Pts',(14.1401795508119,-16.8577962651154,4.98798385481279));
#18247=CARTESIAN_POINT('Ctrl Pts',(13.9724990658054,-16.6659342866535,4.99849675036491));
#18248=CARTESIAN_POINT('Ctrl Pts',(13.7267972620337,-16.2371057275703,5.01725565496171));
#18249=CARTESIAN_POINT('Ctrl Pts',(13.6476132850042,-16.006173713243,5.02735766783692));
#18250=CARTESIAN_POINT('Ctrl Pts',(13.6012386706273,-15.6781123337951,5.04170855932633));
#18251=CARTESIAN_POINT('Ctrl Pts',(13.595,-15.5890130318589,5.04560616658524));
#18252=CARTESIAN_POINT('Ctrl Pts',(13.595,-15.5,5.04949999999989));
#18253=CARTESIAN_POINT('Ctrl Pts',(13.595,-15.5,5.11199999999994));
#18254=CARTESIAN_POINT('Ctrl Pts',(13.595,-15.5611707631063,5.10932411359984));
#18255=CARTESIAN_POINT('Ctrl Pts',(13.5979462709872,-15.6224147859416,5.10664502248724));
#18256=CARTESIAN_POINT('Ctrl Pts',(13.6272636334491,-15.9253242853065,5.09339438821931));
#18257=CARTESIAN_POINT('Ctrl Pts',(13.6967086552716,-16.1604577698354,5.08310858399669));
#18258=CARTESIAN_POINT('Ctrl Pts',(13.9250484322185,-16.6012699913425,5.06382545969629));
#18259=CARTESIAN_POINT('Ctrl Pts',(14.0853910786963,-16.8008393480576,5.05380523133158));
#18260=CARTESIAN_POINT('Ctrl Pts',(14.4715898770798,-17.1228186274331,5.0321321075346));
#18261=CARTESIAN_POINT('Ctrl Pts',(14.6925459349015,-17.2433266240215,5.02112565270137));
#18262=CARTESIAN_POINT('Ctrl Pts',(15.1604831200914,-17.3899398186166,5.00019161564768));
#18263=CARTESIAN_POINT('Ctrl Pts',(15.4021006853459,-17.4176916792359,4.99098640127391));
#18264=CARTESIAN_POINT('Ctrl Pts',(15.894197495309,-17.3807866060864,4.97153666920373));
#18265=CARTESIAN_POINT('Ctrl Pts',(16.1396601805575,-17.3120604793286,4.96073439516675));
#18266=CARTESIAN_POINT('Ctrl Pts',(16.5841552313493,-17.0856734720978,4.938943602977));
#18267=CARTESIAN_POINT('Ctrl Pts',(16.7799825417739,-16.9322741671381,4.92816971504776));
#18268=CARTESIAN_POINT('Ctrl Pts',(17.1004482091901,-16.5615636385129,4.90792095418443));
#18269=CARTESIAN_POINT('Ctrl Pts',(17.2229176548675,-16.348473177732,4.89911606201802));
#18270=CARTESIAN_POINT('Ctrl Pts',(17.3841085989977,-15.8785374579043,4.87855894391533));
#18271=CARTESIAN_POINT('Ctrl Pts',(17.417685068939,-15.6250119572512,4.86746858955605));
#18272=CARTESIAN_POINT('Ctrl Pts',(17.3843966400302,-15.1292914917116,4.84578352982115));
#18273=CARTESIAN_POINT('Ctrl Pts',(17.3215954113712,-14.8915711092175,4.83538456295789));
#18274=CARTESIAN_POINT('Ctrl Pts',(17.1066720877883,-14.4461610901709,4.8159003101562));
#18275=CARTESIAN_POINT('Ctrl Pts',(16.9540693082927,-14.2439448462617,4.80627967554572));
#18276=CARTESIAN_POINT('Ctrl Pts',(16.5798512566287,-13.9108227723273,4.78481671070483));
#18277=CARTESIAN_POINT('Ctrl Pts',(16.3621361692523,-13.7829433415911,4.7737718064256));
#18278=CARTESIAN_POINT('Ctrl Pts',(15.8981495645829,-13.6215234816301,4.75266357735125));
#18279=CARTESIAN_POINT('Ctrl Pts',(15.6574035720047,-13.5862627923587,4.74315415992228));
#18280=CARTESIAN_POINT('Ctrl Pts',(15.164350304509,-13.6078922913303,4.72400230495482));
#18281=CARTESIAN_POINT('Ctrl Pts',(14.9169102804823,-13.6689580320699,4.71329267166129));
#18282=CARTESIAN_POINT('Ctrl Pts',(14.4649631449192,-13.8817241688144,4.69151748491861));
#18283=CARTESIAN_POINT('Ctrl Pts',(14.2639391179947,-14.0295304408853,4.68066905752914));
#18284=CARTESIAN_POINT('Ctrl Pts',(13.932772664396,-14.3902181328522,4.66023413155884));
#18285=CARTESIAN_POINT('Ctrl Pts',(13.8043992661642,-14.5984718038406,4.65143692896586));
#18286=CARTESIAN_POINT('Ctrl Pts',(13.6367795651532,-15.0410028370471,4.63207861605219));
#18287=CARTESIAN_POINT('Ctrl Pts',(13.595,-15.2696606056661,4.62207608899091));
#18288=CARTESIAN_POINT('Ctrl Pts',(13.595,-15.5,4.61199999999993));
#18289=CARTESIAN_POINT('Origin',(15.5,-15.5,-1.713));
#18290=CARTESIAN_POINT('',(13.595,-15.5,4.04949999999988));
#18291=CARTESIAN_POINT('',(13.595,-15.5,4.11199999999992));
#18292=CARTESIAN_POINT('',(13.595,-15.5,-1.713));
#18293=CARTESIAN_POINT('Ctrl Pts',(13.595,-15.5,4.04949999999988));
#18294=CARTESIAN_POINT('Ctrl Pts',(13.595,-15.2566554804107,4.0601449921079));
#18295=CARTESIAN_POINT('Ctrl Pts',(13.6416291796205,-15.0154257502269,4.07069747374311));
#18296=CARTESIAN_POINT('Ctrl Pts',(13.8227217236572,-14.5649657826882,4.09040263417788));
#18297=CARTESIAN_POINT('Ctrl Pts',(13.9548797991019,-14.3597546423013,4.09923794107462));
#18298=CARTESIAN_POINT('Ctrl Pts',(14.292909829855,-14.0055782155994,4.11979046982463));
#18299=CARTESIAN_POINT('Ctrl Pts',(14.49720746026,-13.8614754836012,4.1306819091887));
#18300=CARTESIAN_POINT('Ctrl Pts',(14.9537450464085,-13.6576375985826,4.15243571889545));
#18301=CARTESIAN_POINT('Ctrl Pts',(15.2023316701596,-13.6015499101801,4.16307990854595));
#18302=CARTESIAN_POINT('Ctrl Pts',(15.6959198510094,-13.5897930012685,4.18203609218897));
#18303=CARTESIAN_POINT('Ctrl Pts',(15.9361519808382,-13.6299495035781,4.19178755236659));
#18304=CARTESIAN_POINT('Ctrl Pts',(16.3974688465401,-13.8010675464048,4.21300676261618));
#18305=CARTESIAN_POINT('Ctrl Pts',(16.6129323732134,-13.9337286843887,4.22407095582179));
#18306=CARTESIAN_POINT('Ctrl Pts',(16.9792499981077,-14.2740155925913,4.24539133303587));
#18307=CARTESIAN_POINT('Ctrl Pts',(17.1268460120532,-14.4779549496283,4.25479111765629));
#18308=CARTESIAN_POINT('Ctrl Pts',(17.3329037707492,-14.9263449102112,4.27440572660567));
#18309=CARTESIAN_POINT('Ctrl Pts',(17.3912499783115,-15.165678119567,4.28487524582508));
#18310=CARTESIAN_POINT('Ctrl Pts',(17.4149050488048,-15.6629241163841,4.30662703921166));
#18311=CARTESIAN_POINT('Ctrl Pts',(17.3762059499559,-15.9162576936056,4.31770899797026));
#18312=CARTESIAN_POINT('Ctrl Pts',(17.2055762083363,-16.3826095479846,4.3381093415564));
#18313=CARTESIAN_POINT('Ctrl Pts',(17.0793192680661,-16.5925849475532,4.34689990669029));
#18314=CARTESIAN_POINT('Ctrl Pts',(16.7519910378125,-16.9568853337845,4.3672684436934));
#18315=CARTESIAN_POINT('Ctrl Pts',(16.5528184484167,-17.1067232510974,4.37809116813831));
#18316=CARTESIAN_POINT('Ctrl Pts',(16.1035037812404,-17.3244174572891,4.39987441482088));
#18317=CARTESIAN_POINT('Ctrl Pts',(15.8567467722634,-17.3882454163308,4.41061858883035));
#18318=CARTESIAN_POINT('Ctrl Pts',(15.3640192511005,-17.4153701521319,4.42987829654564));
#18319=CARTESIAN_POINT('Ctrl Pts',(15.1229704593036,-17.3828192570121,4.43926848345183));
#18320=CARTESIAN_POINT('Ctrl Pts',(14.6575381615535,-17.2267535835976,4.46031437279132));
#18321=CARTESIAN_POINT('Ctrl Pts',(14.4386234773176,-17.1015303353839,4.47134662571857));
#18322=CARTESIAN_POINT('Ctrl Pts',(14.0600612599842,-16.7724088007001,4.49288666353421));
#18323=CARTESIAN_POINT('Ctrl Pts',(13.9046731226827,-16.5711467140639,4.50264318836092));
#18324=CARTESIAN_POINT('Ctrl Pts',(13.6848819544518,-16.1273925403157,4.52205500698508));
#18325=CARTESIAN_POINT('Ctrl Pts',(13.6196561257824,-15.8905906989304,4.53241379269747));
#18326=CARTESIAN_POINT('Ctrl Pts',(13.5969136295473,-15.5986541054857,4.54518442233197));
#18327=CARTESIAN_POINT('Ctrl Pts',(13.595,-15.5492987001803,4.54734345143557));
#18328=CARTESIAN_POINT('Ctrl Pts',(13.595,-15.5,4.54949999999988));
#18329=CARTESIAN_POINT('Ctrl Pts',(13.595,-15.5,4.61199999999993));
#18330=CARTESIAN_POINT('Ctrl Pts',(13.595,-15.5232640386944,4.61098232551636));
#18331=CARTESIAN_POINT('Ctrl Pts',(13.5954261508269,-15.5465452312985,4.60996390064311));
#18332=CARTESIAN_POINT('Ctrl Pts',(13.6052367897315,-15.8139970169025,4.59826434746708));
#18333=CARTESIAN_POINT('Ctrl Pts',(13.6610845605679,-16.0541929504136,4.5877570887833));
#18334=CARTESIAN_POINT('Ctrl Pts',(13.8622121225949,-16.5042202298844,4.56807085608553));
#18335=CARTESIAN_POINT('Ctrl Pts',(14.0070602801722,-16.7091112186004,4.55877900762857));
#18336=CARTESIAN_POINT('Ctrl Pts',(14.3689922543407,-17.0533161570304,4.53753907966327));
#18337=CARTESIAN_POINT('Ctrl Pts',(14.5831675755589,-17.188604275571,4.52646623065589));
#18338=CARTESIAN_POINT('Ctrl Pts',(15.0429789041739,-17.3650856346105,4.50518674810786));
#18339=CARTESIAN_POINT('Ctrl Pts',(15.2829454294141,-17.4079441568564,4.49528726380417));
#18340=CARTESIAN_POINT('Ctrl Pts',(15.7768001897292,-17.4016027587752,4.47643943059099));
#18341=CARTESIAN_POINT('Ctrl Pts',(16.025971640107,-17.3482529436014,4.46583296893254));
#18342=CARTESIAN_POINT('Ctrl Pts',(16.484950380057,-17.1493510893542,4.44409464103588));
#18343=CARTESIAN_POINT('Ctrl Pts',(16.6910142239839,-17.0073082566105,4.43318134532223));
#18344=CARTESIAN_POINT('Ctrl Pts',(17.0327916159658,-16.656715134371,4.4125652269926));
#18345=CARTESIAN_POINT('Ctrl Pts',(17.1670173530641,-16.453145959696,4.40369492387121));
#18346=CARTESIAN_POINT('Ctrl Pts',(17.3572681428002,-15.9945022723093,4.38363177044223));
#18347=CARTESIAN_POINT('Ctrl Pts',(17.4066852004337,-15.7418916985545,4.37258143913187));
#18348=CARTESIAN_POINT('Ctrl Pts',(17.4032935450824,-15.2420497972705,4.35071608911945));
#18349=CARTESIAN_POINT('Ctrl Pts',(17.3543721336288,-14.9996155181024,4.3401109150526));
#18350=CARTESIAN_POINT('Ctrl Pts',(17.1667709809438,-14.5451685249118,4.32023134404688));
#18351=CARTESIAN_POINT('Ctrl Pts',(17.0293310383393,-14.3376828194855,4.31118114347071));
#18352=CARTESIAN_POINT('Ctrl Pts',(16.6793953047937,-13.9829651227589,4.29016574175129));
#18353=CARTESIAN_POINT('Ctrl Pts',(16.468880140008,-13.840592555518,4.27907660070989));
#18354=CARTESIAN_POINT('Ctrl Pts',(16.0134108536659,-13.6495638134254,4.25764342732135));
#18355=CARTESIAN_POINT('Ctrl Pts',(15.7741670261507,-13.5993262037908,4.24748113348303));
#18356=CARTESIAN_POINT('Ctrl Pts',(15.279635668209,-13.591040510831,4.22856514199461));
#18357=CARTESIAN_POINT('Ctrl Pts',(15.0289634893632,-13.6369750738018,4.21823722129387));
#18358=CARTESIAN_POINT('Ctrl Pts',(14.5635507617894,-13.8225308635711,4.1965470576802));
#18359=CARTESIAN_POINT('Ctrl Pts',(14.3528429333689,-13.9589370809773,4.18558111538397));
#18360=CARTESIAN_POINT('Ctrl Pts',(14.0010471827939,-14.2998483865189,4.16479722607023));
#18361=CARTESIAN_POINT('Ctrl Pts',(13.8612826681553,-14.499091586802,4.15578427004365));
#18362=CARTESIAN_POINT('Ctrl Pts',(13.6589153177444,-14.9493916272471,4.13608610554475));
#18363=CARTESIAN_POINT('Ctrl Pts',(13.6022372644996,-15.1979412367233,4.12521341921595));
#18364=CARTESIAN_POINT('Ctrl Pts',(13.5952160880688,-15.4668590274496,4.11344973633204));
#18365=CARTESIAN_POINT('Ctrl Pts',(13.595,-15.4834339841796,4.11272467260799));
#18366=CARTESIAN_POINT('Ctrl Pts',(13.595,-15.5,4.11199999999992));
#18367=CARTESIAN_POINT('Origin',(15.5,-15.5,-1.713));
#18368=CARTESIAN_POINT('',(13.595,-15.5,3.54949999999988));
#18369=CARTESIAN_POINT('',(13.595,-15.5,3.61199999999992));
#18370=CARTESIAN_POINT('',(13.595,-15.5,-1.713));
#18371=CARTESIAN_POINT('Ctrl Pts',(13.595,-15.5,3.54949999999987));
#18372=CARTESIAN_POINT('Ctrl Pts',(13.595,-15.4714306338019,3.55074975355185));
#18373=CARTESIAN_POINT('Ctrl Pts',(13.5956426779202,-15.4428377365097,3.55200053646039));
#18374=CARTESIAN_POINT('Ctrl Pts',(13.6082936904735,-15.1620947970368,3.56428150494126));
#18375=CARTESIAN_POINT('Ctrl Pts',(13.6696572782828,-14.9146802469339,3.57510453862906));
#18376=CARTESIAN_POINT('Ctrl Pts',(13.880426471005,-14.4684377853199,3.59462520624122));
#18377=CARTESIAN_POINT('Ctrl Pts',(14.0238215350029,-14.2719721542518,3.60376972316979));
#18378=CARTESIAN_POINT('Ctrl Pts',(14.3821595775149,-13.9374669693537,3.62466134348506));
#18379=CARTESIAN_POINT('Ctrl Pts',(14.5958353841015,-13.8048421102622,3.6356570174231));
#18380=CARTESIAN_POINT('Ctrl Pts',(15.0668629636705,-13.6275606276633,3.65737891554599));
#18381=CARTESIAN_POINT('Ctrl Pts',(15.3202477975265,-13.5865505315346,3.66750548084134));
#18382=CARTESIAN_POINT('Ctrl Pts',(15.816805451799,-13.6058985466812,3.68674019434164));
#18383=CARTESIAN_POINT('Ctrl Pts',(16.0553852487261,-13.6616553849759,3.69699805016475));
#18384=CARTESIAN_POINT('Ctrl Pts',(16.5073683092457,-13.8635796722318,3.71853746206844));
#18385=CARTESIAN_POINT('Ctrl Pts',(16.714984071283,-14.0112137363233,3.72963184335436));
#18386=CARTESIAN_POINT('Ctrl Pts',(17.05584097305,-14.373699760751,3.75047321466667));
#18387=CARTESIAN_POINT('Ctrl Pts',(17.187772715427,-14.5831502941422,3.75939283876362));
#18388=CARTESIAN_POINT('Ctrl Pts',(17.3650890119976,-15.0408869006376,3.77941631236359));
#18389=CARTESIAN_POINT('Ctrl Pts',(17.4086793510686,-15.2848939598667,3.79009028695804));
#18390=CARTESIAN_POINT('Ctrl Pts',(17.4007248859629,-15.7828299846122,3.81187226529337));
#18391=CARTESIAN_POINT('Ctrl Pts',(17.3465633227248,-16.0319496742149,3.82276988951046));
#18392=CARTESIAN_POINT('Ctrl Pts',(17.1487063266573,-16.4843991573608,3.84256208037425));
#18393=CARTESIAN_POINT('Ctrl Pts',(17.0108715057099,-16.6851374249942,3.85151730562961));
#18394=CARTESIAN_POINT('Ctrl Pts',(16.6625618840933,-17.0294349516063,3.87224319119429));
#18395=CARTESIAN_POINT('Ctrl Pts',(16.4534568032229,-17.1678238226488,3.88319178032881));
#18396=CARTESIAN_POINT('Ctrl Pts',(15.990232707778,-17.3580628314253,3.90490146268614));
#18397=CARTESIAN_POINT('Ctrl Pts',(15.7400758586494,-17.406575753888,3.91537053064848));
#18398=CARTESIAN_POINT('Ctrl Pts',(15.2457706807686,-17.4034117022829,3.93416593165765));
#18399=CARTESIAN_POINT('Ctrl Pts',(15.0062602511874,-17.3557492987601,3.94428199982258));
#18400=CARTESIAN_POINT('Ctrl Pts',(14.5492523840756,-17.1698208151633,3.9656619064038));
#18401=CARTESIAN_POINT('Ctrl Pts',(14.3374287724992,-17.0299202761496,3.97674654762224));
#18402=CARTESIAN_POINT('Ctrl Pts',(13.9832783004022,-16.6788629497716,3.99784155938021));
#18403=CARTESIAN_POINT('Ctrl Pts',(13.8432530482872,-16.4722882519258,4.0069677055148));
#18404=CARTESIAN_POINT('Ctrl Pts',(13.650892065042,-16.0193844357471,4.02677977096443));
#18405=CARTESIAN_POINT('Ctrl Pts',(13.5995218004781,-15.7777160633025,4.03735144080016));
#18406=CARTESIAN_POINT('Ctrl Pts',(13.5950950344528,-15.5219764732979,4.04853864946178));
#18407=CARTESIAN_POINT('Ctrl Pts',(13.595,-15.5109860814884,4.04901941900738));
#18408=CARTESIAN_POINT('Ctrl Pts',(13.595,-15.5,4.04949999999988));
#18409=CARTESIAN_POINT('Ctrl Pts',(13.595,-15.5,4.11199999999992));
#18410=CARTESIAN_POINT('Ctrl Pts',(13.595,-15.7289515329785,4.10198462235432));
#18411=CARTESIAN_POINT('Ctrl Pts',(13.6362767838862,-15.9561952829852,4.09204395087554));
#18412=CARTESIAN_POINT('Ctrl Pts',(13.8031781282484,-16.399850271514,4.07263647106237));
#18413=CARTESIAN_POINT('Ctrl Pts',(13.9326934273677,-16.6101744716854,4.06376028309602));
#18414=CARTESIAN_POINT('Ctrl Pts',(14.2695258573257,-16.9760551325534,4.04299712598332));
#18415=CARTESIAN_POINT('Ctrl Pts',(14.4758216995285,-17.1259934829378,4.031902348414));
#18416=CARTESIAN_POINT('Ctrl Pts',(14.9261854058435,-17.3327070455456,4.01031953161981));
#18417=CARTESIAN_POINT('Ctrl Pts',(15.1644321192768,-17.3908977234114,4.00002106070406));
#18418=CARTESIAN_POINT('Ctrl Pts',(15.6600647053582,-17.4150713967616,3.98071584429264));
#18419=CARTESIAN_POINT('Ctrl Pts',(15.91289423843,-17.3768775258912,3.97074286366531));
#18420=CARTESIAN_POINT('Ctrl Pts',(16.3852486918124,-17.2051526017849,3.9490922329447));
#18421=CARTESIAN_POINT('Ctrl Pts',(16.6006191253838,-17.0747539459622,3.93808105207819));
#18422=CARTESIAN_POINT('Ctrl Pts',(16.9627468340224,-16.7439911348198,3.9171277187157));
#18423=CARTESIAN_POINT('Ctrl Pts',(17.1082515721606,-16.5491183901532,3.90789319292009));
#18424=CARTESIAN_POINT('Ctrl Pts',(17.3238511193209,-16.1052398174181,3.88847593252048));
#18425=CARTESIAN_POINT('Ctrl Pts',(17.3879059803852,-15.8585209725764,3.87768333213371));
#18426=CARTESIAN_POINT('Ctrl Pts',(17.4158038721806,-15.360398937719,3.8558932168731));
#18427=CARTESIAN_POINT('Ctrl Pts',(17.3816850354908,-15.1139096327732,3.84511065760162));
#18428=CARTESIAN_POINT('Ctrl Pts',(17.2224165141855,-14.6505493382599,3.82484117840156));
#18429=CARTESIAN_POINT('Ctrl Pts',(17.0999032647057,-14.4376467115784,3.81604112977348));
#18430=CARTESIAN_POINT('Ctrl Pts',(16.7748696009735,-14.061977534995,3.79551085863747));
#18431=CARTESIAN_POINT('Ctrl Pts',(16.5725626027766,-13.9053845439179,3.78442164186843));
#18432=CARTESIAN_POINT('Ctrl Pts',(16.1272021809119,-13.6847779241333,3.76272449623994));
#18433=CARTESIAN_POINT('Ctrl Pts',(15.8900665879685,-13.6194996239372,3.7523130965143));
#18434=CARTESIAN_POINT('Ctrl Pts',(15.3971856556628,-13.5813381708641,3.73280617897475));
#18435=CARTESIAN_POINT('Ctrl Pts',(15.1459364906506,-13.6114840999463,3.72322615732184));
#18436=CARTESIAN_POINT('Ctrl Pts',(14.6699367047473,-13.7671979148179,3.70178762651588));
#18437=CARTESIAN_POINT('Ctrl Pts',(14.4498038355065,-13.8910577433524,3.6907390450969));
#18438=CARTESIAN_POINT('Ctrl Pts',(14.0767904715835,-14.2109353139354,3.66961140579681));
#18439=CARTESIAN_POINT('Ctrl Pts',(13.9251913483846,-14.401292583377,3.66006244167204));
#18440=CARTESIAN_POINT('Ctrl Pts',(13.6958596666349,-14.8383295596045,3.64094446370933));
#18441=CARTESIAN_POINT('Ctrl Pts',(13.6241715837739,-15.0828985570044,3.63024590739263));
#18442=CARTESIAN_POINT('Ctrl Pts',(13.5974013523169,-15.3894873060977,3.61683432606746));
#18443=CARTESIAN_POINT('Ctrl Pts',(13.595,-15.4447751296727,3.61441578610347));
#18444=CARTESIAN_POINT('Ctrl Pts',(13.595,-15.5,3.61199999999992));
#18445=CARTESIAN_POINT('Origin',(15.5,-15.5,-1.713));
#18446=CARTESIAN_POINT('',(13.595,-15.5,3.04949999999987));
#18447=CARTESIAN_POINT('',(13.595,-15.5,3.11199999999991));
#18448=CARTESIAN_POINT('',(13.595,-15.5,-1.713));
#18449=CARTESIAN_POINT('Ctrl Pts',(13.595,-15.5,3.04949999999986));
#18450=CARTESIAN_POINT('Ctrl Pts',(13.595,-15.4321105957089,3.05246979021382));
#18451=CARTESIAN_POINT('Ctrl Pts',(13.5986290164635,-15.3641437215775,3.05544296930955));
#18452=CARTESIAN_POINT('Ctrl Pts',(13.6328808295919,-15.0455144947905,3.06938125569569));
#18453=CARTESIAN_POINT('Ctrl Pts',(13.7094288974123,-14.8024529166051,3.08001387066443));
#18454=CARTESIAN_POINT('Ctrl Pts',(13.947539576482,-14.3698817602423,3.09893649342746));
#18455=CARTESIAN_POINT('Ctrl Pts',(14.1031156679202,-14.1824041143387,3.10873274825438));
#18456=CARTESIAN_POINT('Ctrl Pts',(14.4831736554388,-13.869683883395,3.12997071796454));
#18457=CARTESIAN_POINT('Ctrl Pts',(14.7063014598291,-13.7501680402349,3.14103774633167));
#18458=CARTESIAN_POINT('Ctrl Pts',(15.1845327630667,-13.6048554585229,3.1623333171254));
#18459=CARTESIAN_POINT('Ctrl Pts',(15.4347763272853,-13.5798893549735,3.17169857042788));
#18460=CARTESIAN_POINT('Ctrl Pts',(15.9257996252396,-13.6272081761908,3.19133540596976));
#18461=CARTESIAN_POINT('Ctrl Pts',(16.1620890876457,-13.6971483687584,3.20181671714098));
#18462=CARTESIAN_POINT('Ctrl Pts',(16.6039237010221,-13.926849213995,3.223579202796));
#18463=CARTESIAN_POINT('Ctrl Pts',(16.8034884338474,-14.0877738251061,3.2346592742694));
#18464=CARTESIAN_POINT('Ctrl Pts',(17.1206937121615,-14.4698128490763,3.25503229881968));
#18465=CARTESIAN_POINT('Ctrl Pts',(17.2386202282881,-14.6844418676755,3.26382379123663));
#18466=CARTESIAN_POINT('Ctrl Pts',(17.3888917629425,-15.1505366019541,3.28421288722432));
#18467=CARTESIAN_POINT('Ctrl Pts',(17.4182411410945,-15.398128473592,3.29504367775966));
#18468=CARTESIAN_POINT('Ctrl Pts',(17.3803891247896,-15.8960433325684,3.31682473020833));
#18469=CARTESIAN_POINT('Ctrl Pts',(17.3114425366699,-16.1414147811316,3.32755838937558));
#18470=CARTESIAN_POINT('Ctrl Pts',(17.0870494462786,-16.5809326899874,3.34678489457488));
#18471=CARTESIAN_POINT('Ctrl Pts',(16.9376592234311,-16.7729119854775,3.35621069918009));
#18472=CARTESIAN_POINT('Ctrl Pts',(16.5685797137467,-17.096747035341,3.37727586787364));
#18473=CARTESIAN_POINT('Ctrl Pts',(16.3501494254049,-17.2229943740628,3.38831216918689));
#18474=CARTESIAN_POINT('Ctrl Pts',(15.875438963893,-17.3845028077707,3.40982859683191));
#18475=CARTESIAN_POINT('Ctrl Pts',(15.6236218003128,-17.4175504251718,3.41954222081694));
#18476=CARTESIAN_POINT('Ctrl Pts',(15.1297300926185,-17.3844660181691,3.43897638394394));
#18477=CARTESIAN_POINT('Ctrl Pts',(14.8921660094684,-17.3217654308467,3.44934763611788));
#18478=CARTESIAN_POINT('Ctrl Pts',(14.4449362538756,-17.1062023062259,3.47100528668579));
#18479=CARTESIAN_POINT('Ctrl Pts',(14.2411534699628,-16.9520199343099,3.48209768623437));
#18480=CARTESIAN_POINT('Ctrl Pts',(13.9118146101572,-16.5798949736209,3.50271353485158));
#18481=CARTESIAN_POINT('Ctrl Pts',(13.7867599790489,-16.3679365738482,3.51153252082878));
#18482=CARTESIAN_POINT('Ctrl Pts',(13.6321534490399,-15.9330658290354,3.53055573801219));
#18483=CARTESIAN_POINT('Ctrl Pts',(13.595,-15.7172130300017,3.53999811767259));
#18484=CARTESIAN_POINT('Ctrl Pts',(13.595,-15.5,3.54949999999988));
#18485=CARTESIAN_POINT('Ctrl Pts',(13.595,-15.5,3.61199999999992));
#18486=CARTESIAN_POINT('Ctrl Pts',(13.595,-15.6912263683259,3.60363489202415));
#18487=CARTESIAN_POINT('Ctrl Pts',(13.6237955742172,-15.8816979151119,3.59530280336343));
#18488=CARTESIAN_POINT('Ctrl Pts',(13.7525672066139,-16.2963954817282,3.57716205241783));
#18489=CARTESIAN_POINT('Ctrl Pts',(13.8679408263096,-16.5120016187347,3.56836062535117));
#18490=CARTESIAN_POINT('Ctrl Pts',(14.1807548240299,-16.8975712486844,3.54807673717706));
#18491=CARTESIAN_POINT('Ctrl Pts',(14.378749169732,-17.0608955312897,3.53700367180145));
#18492=CARTESIAN_POINT('Ctrl Pts',(14.8185361132323,-17.2956523714065,3.51520817375324));
#18493=CARTESIAN_POINT('Ctrl Pts',(15.0543137168578,-17.3681921867867,3.504689394135));
#18494=CARTESIAN_POINT('Ctrl Pts',(15.5442842580433,-17.420605965555,3.4849810028333));
#18495=CARTESIAN_POINT('Ctrl Pts',(15.7939800289263,-17.3984927944794,3.4757205697281));
#18496=CARTESIAN_POINT('Ctrl Pts',(16.2734020976102,-17.2589383174709,3.45450583092146));
#18497=CARTESIAN_POINT('Ctrl Pts',(16.4981534303578,-17.1418589191606,3.44343058757723));
#18498=CARTESIAN_POINT('Ctrl Pts',(16.8821020250365,-16.8331318042905,3.42213256508492));
#18499=CARTESIAN_POINT('Ctrl Pts',(17.039887556192,-16.6472320007423,3.4121851268916));
#18500=CARTESIAN_POINT('Ctrl Pts',(17.2828123298839,-16.2171395290268,3.39337093302828));
#18501=CARTESIAN_POINT('Ctrl Pts',(17.3620167587507,-15.974948381623,3.38277639464667));
#18502=CARTESIAN_POINT('Ctrl Pts',(17.4209499111993,-15.4781318962858,3.36104339003874));
#18503=CARTESIAN_POINT('Ctrl Pts',(17.4017949090046,-15.2285052132451,3.35012358763101));
#18504=CARTESIAN_POINT('Ctrl Pts',(17.2705998510944,-14.756774399514,3.32948794398572));
#18505=CARTESIAN_POINT('Ctrl Pts',(17.1621720414811,-14.5384461715233,3.32060482498444));
#18506=CARTESIAN_POINT('Ctrl Pts',(16.8614197732683,-14.143328147286,3.30056903685509));
#18507=CARTESIAN_POINT('Ctrl Pts',(16.6678535046653,-13.9735260229966,3.28952203912671));
#18508=CARTESIAN_POINT('Ctrl Pts',(16.2339422406164,-13.7250547244282,3.267649168307));
#18509=CARTESIAN_POINT('Ctrl Pts',(15.9997053097084,-13.6454347321454,3.25703389583053));
#18510=CARTESIAN_POINT('Ctrl Pts',(15.5126654428033,-13.5791741921149,3.23713366978456));
#18511=CARTESIAN_POINT('Ctrl Pts',(15.2644104975039,-13.5936329492472,3.22810485701442));
#18512=CARTESIAN_POINT('Ctrl Pts',(14.7819276091953,-13.7176467043136,3.20711407330051));
#18513=CARTESIAN_POINT('Ctrl Pts',(14.5529205606612,-13.8280415224273,3.19602381386336));
#18514=CARTESIAN_POINT('Ctrl Pts',(14.1586389397585,-14.1257757598693,3.17457477542644));
#18515=CARTESIAN_POINT('Ctrl Pts',(13.9948696580682,-14.3073777317988,3.16439851364743));
#18516=CARTESIAN_POINT('Ctrl Pts',(13.7390376698131,-14.7307767400854,3.14544591062588));
#18517=CARTESIAN_POINT('Ctrl Pts',(13.6527198374731,-14.9705690984086,3.13515970698127));
#18518=CARTESIAN_POINT('Ctrl Pts',(13.6018721779538,-15.3130738890647,3.12017699522903));
#18519=CARTESIAN_POINT('Ctrl Pts',(13.595,-15.406576934727,3.11608674826207));
#18520=CARTESIAN_POINT('Ctrl Pts',(13.595,-15.5,3.11199999999991));
#18521=CARTESIAN_POINT('Origin',(15.5,-15.5,-1.713));
#18522=CARTESIAN_POINT('',(13.595,-15.5,2.54949999999986));
#18523=CARTESIAN_POINT('',(13.595,-15.5,2.6119999999999));
#18524=CARTESIAN_POINT('',(13.595,-15.5,-1.713));
#18525=CARTESIAN_POINT('Ctrl Pts',(13.595,-15.5,2.54949999999986));
#18526=CARTESIAN_POINT('Ctrl Pts',(13.595,-15.3940361834186,2.5541353375581));
#18527=CARTESIAN_POINT('Ctrl Pts',(13.6038410612059,-15.288011292421,2.55877334678806));
#18528=CARTESIAN_POINT('Ctrl Pts',(13.6637959758933,-14.9326929260908,2.57431658241056));
#18529=CARTESIAN_POINT('Ctrl Pts',(13.7556513218222,-14.6933434299402,2.58439405147275));
#18530=CARTESIAN_POINT('Ctrl Pts',(14.0218508967873,-14.2739914824746,2.60365090047229));
#18531=CARTESIAN_POINT('Ctrl Pts',(14.1900364862303,-14.0957225603647,2.61392156775413));
#18532=CARTESIAN_POINT('Ctrl Pts',(14.5919478068822,-13.8064400352437,2.63547479068998));
#18533=CARTESIAN_POINT('Ctrl Pts',(14.8240308016903,-13.7011730185504,2.64656942225763));
#18534=CARTESIAN_POINT('Ctrl Pts',(15.3086740652865,-13.5888469871871,2.66738641235951));
#18535=CARTESIAN_POINT('Ctrl Pts',(15.5558872301103,-13.5801080383882,2.67629150394634));
#18536=CARTESIAN_POINT('Ctrl Pts',(16.0406340441411,-13.6568795152485,2.69633475826763));
#18537=CARTESIAN_POINT('Ctrl Pts',(16.2735546088288,-13.7418824267643,2.70701789833068));
#18538=CARTESIAN_POINT('Ctrl Pts',(16.7000523184248,-13.9991266542888,2.72880179880874));
#18539=CARTESIAN_POINT('Ctrl Pts',(16.8881704153838,-14.1711854189613,2.73969175651716));
#18540=CARTESIAN_POINT('Ctrl Pts',(17.1797897502373,-14.5696454767515,2.75945465157896));
#18541=CARTESIAN_POINT('Ctrl Pts',(17.2840108819561,-14.7896704164612,2.76842696484944));
#18542=CARTESIAN_POINT('Ctrl Pts',(17.4065692980086,-15.263878896105,2.78917099283035));
#18543=CARTESIAN_POINT('Ctrl Pts',(17.4210805548441,-15.5142899744512,2.80012510824357));
#18544=CARTESIAN_POINT('Ctrl Pts',(17.3526145046678,-16.0104396109907,2.82182894186297));
#18545=CARTESIAN_POINT('Ctrl Pts',(17.2687722227482,-16.2510780878475,2.83225316559533));
#18546=CARTESIAN_POINT('Ctrl Pts',(17.0174591997819,-16.6768447431001,2.85108635850073));
#18547=CARTESIAN_POINT('Ctrl Pts',(16.8557719537965,-16.8599648202848,2.86121694909931));
#18548=CARTESIAN_POINT('Ctrl Pts',(16.4651080959497,-17.1615752395479,2.88261371352921));
#18549=CARTESIAN_POINT('Ctrl Pts',(16.2375728975395,-17.2743330486224,2.89369989754563));
#18550=CARTESIAN_POINT('Ctrl Pts',(15.7561389183535,-17.4037991586832,2.91477019987504));
#18551=CARTESIAN_POINT('Ctrl Pts',(15.5073852023538,-17.4209364189226,2.92387165431679));
#18552=CARTESIAN_POINT('Ctrl Pts',(15.0193020385475,-17.3595502717834,2.94370479047538));
#18553=CARTESIAN_POINT('Ctrl Pts',(14.7844977321494,-17.2824246763799,2.95428699922258));
#18554=CARTESIAN_POINT('Ctrl Pts',(14.3484663173313,-17.0387757372993,2.97613471364169));
#18555=CARTESIAN_POINT('Ctrl Pts',(14.1533146606275,-16.8712461198078,2.98719206714309));
#18556=CARTESIAN_POINT('Ctrl Pts',(13.8482952604552,-16.4794816922368,3.00731616001192));
#18557=CARTESIAN_POINT('Ctrl Pts',(13.7374206757829,-16.2621233443958,3.01616127102353));
#18558=CARTESIAN_POINT('Ctrl Pts',(13.6202078713138,-15.8572987167627,3.0338701348745));
#18559=CARTESIAN_POINT('Ctrl Pts',(13.595,-15.6789183932981,3.04167329863075));
#18560=CARTESIAN_POINT('Ctrl Pts',(13.595,-15.5,3.04949999999987));
#18561=CARTESIAN_POINT('Ctrl Pts',(13.595,-15.5,3.11199999999991));
#18562=CARTESIAN_POINT('Ctrl Pts',(13.595,-15.6541792241808,3.10525550200425));
#18563=CARTESIAN_POINT('Ctrl Pts',(13.613718234728,-15.8081406136927,3.09852053308432));
#18564=CARTESIAN_POINT('Ctrl Pts',(13.7090394672623,-16.1925812119671,3.08170335905656));
#18565=CARTESIAN_POINT('Ctrl Pts',(13.8110165548982,-16.4135268313214,3.07267100412813));
#18566=CARTESIAN_POINT('Ctrl Pts',(14.0985444841908,-16.8147940837865,3.05300170765842));
#18567=CARTESIAN_POINT('Ctrl Pts',(14.284916456441,-16.9887287487779,3.04213686973113));
#18568=CARTESIAN_POINT('Ctrl Pts',(14.7089980877039,-17.2503705018038,3.02034831581753));
#18569=CARTESIAN_POINT('Ctrl Pts',(14.9412957771862,-17.3377551330109,3.00963667907495));
#18570=CARTESIAN_POINT('Ctrl Pts',(15.425009209639,-17.4191761013693,2.9895308783385));
#18571=CARTESIAN_POINT('Ctrl Pts',(15.6717770752374,-17.4129441093406,2.98066617426629));
#18572=CARTESIAN_POINT('Ctrl Pts',(16.1573332309325,-17.3057573161853,2.95992700705835));
#18573=CARTESIAN_POINT('Ctrl Pts',(16.390733983597,-17.202771203951,2.9488323422645));
#18574=CARTESIAN_POINT('Ctrl Pts',(16.7959446123815,-16.9172652580428,2.92723673109367));
#18575=CARTESIAN_POINT('Ctrl Pts',(16.9660511030679,-16.7404954349544,2.91692608131995));
#18576=CARTESIAN_POINT('Ctrl Pts',(17.2359307593028,-16.3243308173734,2.89759953070515));
#18577=CARTESIAN_POINT('Ctrl Pts',(17.329922430845,-16.086848361495,2.88767140688958));
#18578=CARTESIAN_POINT('Ctrl Pts',(17.419039281697,-15.5924146793421,2.86604263689164));
#18579=CARTESIAN_POINT('Ctrl Pts',(17.4146395404487,-15.3405974098753,2.85502700830604));
#18580=CARTESIAN_POINT('Ctrl Pts',(17.3108147227307,-14.8611790687817,2.83405507737456));
#18581=CARTESIAN_POINT('Ctrl Pts',(17.2155386186557,-14.6374175395723,2.82479128585809));
#18582=CARTESIAN_POINT('Ctrl Pts',(16.9402795018166,-14.2278595428682,2.80540544219412));
#18583=CARTESIAN_POINT('Ctrl Pts',(16.7592354923017,-14.0484317997801,2.79462230208097));
#18584=CARTESIAN_POINT('Ctrl Pts',(16.3426399863644,-13.7737933372308,2.77283308412301));
#18585=CARTESIAN_POINT('Ctrl Pts',(16.1123449290347,-13.679319787484,2.76204226413672));
#18586=CARTESIAN_POINT('Ctrl Pts',(15.6317787700925,-13.5840519387568,2.74175283166924));
#18587=CARTESIAN_POINT('Ctrl Pts',(15.3862782785964,-13.5828955095755,2.73295653304968));
#18588=CARTESIAN_POINT('Ctrl Pts',(14.8981505326115,-13.6748912262251,2.7124522072999));
#18589=CARTESIAN_POINT('Ctrl Pts',(14.6609818552512,-13.7710462848872,2.70136420953493));
#18590=CARTESIAN_POINT('Ctrl Pts',(14.2462245208683,-14.0451812116636,2.67965564210842));
#18591=CARTESIAN_POINT('Ctrl Pts',(14.0705192229696,-14.2174030232141,2.66923236313488));
#18592=CARTESIAN_POINT('Ctrl Pts',(13.7898612961189,-14.6241409731265,2.64970367243574));
#18593=CARTESIAN_POINT('Ctrl Pts',(13.6896766603476,-14.8562213087964,2.64016179751552));
#18594=CARTESIAN_POINT('Ctrl Pts',(13.6090916105792,-15.2324968962277,2.62370179806533));
#18595=CARTESIAN_POINT('Ctrl Pts',(13.595,-15.366223536707,2.61785198877037));
#18596=CARTESIAN_POINT('Ctrl Pts',(13.595,-15.5,2.6119999999999));
#18597=CARTESIAN_POINT('Origin',(15.5,-15.5,-1.713));
#18598=CARTESIAN_POINT('',(13.595,-15.5,2.04949999999985));
#18599=CARTESIAN_POINT('',(13.595,-15.5,2.1119999999999));
#18600=CARTESIAN_POINT('',(13.595,-15.5,-1.713));
#18601=CARTESIAN_POINT('Ctrl Pts',(13.595,-15.5,2.04949999999985));
#18602=CARTESIAN_POINT('Ctrl Pts',(13.595,-15.3526486934652,2.05594581393401));
#18603=CARTESIAN_POINT('Ctrl Pts',(13.6120968804531,-15.2054448958345,2.06238517516013));
#18604=CARTESIAN_POINT('Ctrl Pts',(13.7034856401193,-14.8191904603802,2.07928169464633));
#18605=CARTESIAN_POINT('Ctrl Pts',(13.807683709322,-14.5905944092652,2.08861259389317));
#18606=CARTESIAN_POINT('Ctrl Pts',(14.0954068155114,-14.1901100509355,2.10827216075147));
#18607=CARTESIAN_POINT('Ctrl Pts',(14.2747550927947,-14.0209968668794,2.11876545717668));
#18608=CARTESIAN_POINT('Ctrl Pts',(14.6956659242681,-13.7545647545419,2.14053866491739));
#18609=CARTESIAN_POINT('Ctrl Pts',(14.9352252828671,-13.6630075465578,2.15161666554088));
#18610=CARTESIAN_POINT('Ctrl Pts',(15.4249588273584,-13.5810818633938,2.17196157071134));
#18611=CARTESIAN_POINT('Ctrl Pts',(15.6696588246589,-13.5871236646452,2.18075506056207));
#18612=CARTESIAN_POINT('Ctrl Pts',(16.1480609274808,-13.6916595237858,2.20116522258474));
#18613=CARTESIAN_POINT('Ctrl Pts',(16.3768922992146,-13.7908690686559,2.21200417943249));
#18614=CARTESIAN_POINT('Ctrl Pts',(16.7882374895011,-14.0741124315941,2.23378270375365));
#18615=CARTESIAN_POINT('Ctrl Pts',(16.9656118429198,-14.2571336410767,2.24450542032328));
#18616=CARTESIAN_POINT('Ctrl Pts',(17.232591142638,-14.6721839437799,2.26369772160026));
#18617=CARTESIAN_POINT('Ctrl Pts',(17.32336258372,-14.8978957552497,2.27316123163802));
#18618=CARTESIAN_POINT('Ctrl Pts',(17.4175725023467,-15.379897660735,2.29424617938454));
#18619=CARTESIAN_POINT('Ctrl Pts',(17.416771052051,-15.6322795723552,2.30528650797685));
#18620=CARTESIAN_POINT('Ctrl Pts',(17.3174983539088,-16.1235866145717,2.32677850457425));
#18621=CARTESIAN_POINT('Ctrl Pts',(17.2195060026385,-16.3575766402513,2.33644892562892));
#18622=CARTESIAN_POINT('Ctrl Pts',(16.9426815429992,-16.7676830021745,2.35590606453524));
#18623=CARTESIAN_POINT('Ctrl Pts',(16.7689623850692,-16.9415492968901,2.36629006940178));
#18624=CARTESIAN_POINT('Ctrl Pts',(16.3575795447531,-17.2197813255831,2.38796041081653));
#18625=CARTESIAN_POINT('Ctrl Pts',(16.1217348139336,-17.3183915250379,2.39905195184739));
#18626=CARTESIAN_POINT('Ctrl Pts',(15.6345046479807,-17.4158138950701,2.41964096699268));
#18627=CARTESIAN_POINT('Ctrl Pts',(15.3885595106893,-17.4172936498083,2.42845290769226));
#18628=CARTESIAN_POINT('Ctrl Pts',(14.9068531433475,-17.3269904646265,2.4486769472318));
#18629=CARTESIAN_POINT('Ctrl Pts',(14.6758146573805,-17.235057316894,2.45944036682785));
#18630=CARTESIAN_POINT('Ctrl Pts',(14.2564853609403,-16.9650604282408,2.48123162962728));
#18631=CARTESIAN_POINT('Ctrl Pts',(14.07350939839,-16.7875855524868,2.49204524597581));
#18632=CARTESIAN_POINT('Ctrl Pts',(13.7938372069924,-16.3809882663696,2.51153351655939));
#18633=CARTESIAN_POINT('Ctrl Pts',(13.6961550187377,-16.1582494665765,2.52070518518896));
#18634=CARTESIAN_POINT('Ctrl Pts',(13.6108922085804,-15.7840215340723,2.5370756109328));
#18635=CARTESIAN_POINT('Ctrl Pts',(13.595,-15.6420656569251,2.54328540433385));
#18636=CARTESIAN_POINT('Ctrl Pts',(13.595,-15.5,2.54949999999986));
#18637=CARTESIAN_POINT('Ctrl Pts',(13.595,-15.5,2.6119999999999));
#18638=CARTESIAN_POINT('Ctrl Pts',(13.595,-15.615287445997,2.60695680463695));
#18639=CARTESIAN_POINT('Ctrl Pts',(13.6054654128687,-15.7306118946473,2.6019119906104));
#18640=CARTESIAN_POINT('Ctrl Pts',(13.670049584727,-16.081817780845,2.58654865350639));
#18641=CARTESIAN_POINT('Ctrl Pts',(13.7583532889062,-16.3086177155276,2.57696069284612));
#18642=CARTESIAN_POINT('Ctrl Pts',(14.020789732391,-16.7266478553754,2.55787531678046));
#18643=CARTESIAN_POINT('Ctrl Pts',(14.1961267477515,-16.9116012234265,2.54718752178696));
#18644=CARTESIAN_POINT('Ctrl Pts',(14.6045256721147,-17.1995071556895,2.52541863248213));
#18645=CARTESIAN_POINT('Ctrl Pts',(14.8325163477983,-17.3012976294405,2.51455507369634));
#18646=CARTESIAN_POINT('Ctrl Pts',(15.3097162815879,-17.41089322416,2.49407978661385));
#18647=CARTESIAN_POINT('Ctrl Pts',(15.5539975592879,-17.4195838172506,2.48527334429313));
#18648=CARTESIAN_POINT('Ctrl Pts',(16.0445699132335,-17.3431226694445,2.46501618354009));
#18649=CARTESIAN_POINT('Ctrl Pts',(16.2853900758208,-17.2540823090537,2.45394546793468));
#18650=CARTESIAN_POINT('Ctrl Pts',(16.7095797727962,-16.9918828300599,2.43214062134231));
#18651=CARTESIAN_POINT('Ctrl Pts',(16.8908809222461,-16.8244868770546,2.4216109022845));
#18652=CARTESIAN_POINT('Ctrl Pts',(17.182411929644,-16.4273976284614,2.40188133611241));
#18653=CARTESIAN_POINT('Ctrl Pts',(17.2887599224322,-16.2006598902134,2.39265003894187));
#18654=CARTESIAN_POINT('Ctrl Pts',(17.4092659708329,-15.716244240958,2.37145950310392));
#18655=CARTESIAN_POINT('Ctrl Pts',(17.4211158419616,-15.4630147587218,2.36038209793174));
#18656=CARTESIAN_POINT('Ctrl Pts',(17.3473304857396,-14.9757380640176,2.33906640699979));
#18657=CARTESIAN_POINT('Ctrl Pts',(17.2659610749238,-14.7458062619205,2.32907219089834));
#18658=CARTESIAN_POINT('Ctrl Pts',(17.0163007825848,-14.3195177133891,2.31029019484638));
#18659=CARTESIAN_POINT('Ctrl Pts',(16.8467786602378,-14.1292823167842,2.29970716060499));
#18660=CARTESIAN_POINT('Ctrl Pts',(16.4469056037788,-13.8284931106128,2.27797947782861));
#18661=CARTESIAN_POINT('Ctrl Pts',(16.2214188791038,-13.7195150770427,2.26705357019215));
#18662=CARTESIAN_POINT('Ctrl Pts',(15.7476574275375,-13.5957822729623,2.24639933334043));
#18663=CARTESIAN_POINT('Ctrl Pts',(15.5044765268383,-13.5797520093936,2.23750309629325));
#18664=CARTESIAN_POINT('Ctrl Pts',(15.0116950071339,-13.6410692883709,2.21749347450548));
#18665=CARTESIAN_POINT('Ctrl Pts',(14.7675175251247,-13.7230597672649,2.20644976751076));
#18666=CARTESIAN_POINT('Ctrl Pts',(14.3344695720043,-13.9733447110082,2.18456993372551));
#18667=CARTESIAN_POINT('Ctrl Pts',(14.1478486714339,-14.1358739422802,2.17394512810839));
#18668=CARTESIAN_POINT('Ctrl Pts',(13.8458586534847,-14.5235480647069,2.15402526422184));
#18669=CARTESIAN_POINT('Ctrl Pts',(13.7336458769756,-14.7452548620724,2.14501597278763));
#18670=CARTESIAN_POINT('Ctrl Pts',(13.6190362478944,-15.1510323337707,2.12726542721903));
#18671=CARTESIAN_POINT('Ctrl Pts',(13.595,-15.3252887149695,2.11964266338706));
#18672=CARTESIAN_POINT('Ctrl Pts',(13.595,-15.5,2.1119999999999));
#18673=CARTESIAN_POINT('Origin',(15.5,-15.5,-1.713));
#18674=CARTESIAN_POINT('',(13.595,-15.5,1.54949999999985));
#18675=CARTESIAN_POINT('',(13.595,-15.5,1.61199999999989));
#18676=CARTESIAN_POINT('',(13.595,-15.5,-1.713));
#18677=CARTESIAN_POINT('Ctrl Pts',(13.595,-15.5,1.54949999999985));
#18678=CARTESIAN_POINT('Ctrl Pts',(13.595,-15.3100000278905,1.55781145984716));
#18679=CARTESIAN_POINT('Ctrl Pts',(13.6234274993569,-15.1207028088503,1.5660921780903));
#18680=CARTESIAN_POINT('Ctrl Pts',(13.7518428572065,-14.7044017556307,1.58430307280682));
#18681=CARTESIAN_POINT('Ctrl Pts',(13.8685053079182,-14.4864653856672,1.59319428948728));
#18682=CARTESIAN_POINT('Ctrl Pts',(14.1784881282718,-14.1060768557497,1.61325759929138));
#18683=CARTESIAN_POINT('Ctrl Pts',(14.3691246157502,-13.9474143171397,1.62394995757439));
#18684=CARTESIAN_POINT('Ctrl Pts',(14.8059894395499,-13.7080473986579,1.64573558726254));
#18685=CARTESIAN_POINT('Ctrl Pts',(15.0492987655172,-13.6319442278147,1.65661763637394));
#18686=CARTESIAN_POINT('Ctrl Pts',(15.5403101516429,-13.580206165741,1.67635067946095));
#18687=CARTESIAN_POINT('Ctrl Pts',(15.7828630482455,-13.6007284968042,1.68534124383068));
#18688=CARTESIAN_POINT('Ctrl Pts',(16.2544413111661,-13.7331901706492,1.70610369319571));
#18689=CARTESIAN_POINT('Ctrl Pts',(16.4782688030326,-13.8465841050468,1.71706332841971));
#18690=CARTESIAN_POINT('Ctrl Pts',(16.8727741026647,-14.1552977792804,1.73876098583554));
#18691=CARTESIAN_POINT('Ctrl Pts',(17.0386250139318,-14.3487777596965,1.74914032194625));
#18692=CARTESIAN_POINT('Ctrl Pts',(17.2803211699226,-14.7801802079204,1.76801182011877));
#18693=CARTESIAN_POINT('Ctrl Pts',(17.3573139006528,-15.0121012423612,1.77815709721592));
#18694=CARTESIAN_POINT('Ctrl Pts',(17.4215377922237,-15.5016183964856,1.79957079599651));
#18695=CARTESIAN_POINT('Ctrl Pts',(17.4045339268535,-15.7550815033061,1.81065842096679));
#18696=CARTESIAN_POINT('Ctrl Pts',(17.2742621948363,-16.2361710137032,1.83170345641724));
#18697=CARTESIAN_POINT('Ctrl Pts',(17.1640657129151,-16.4596003404794,1.84078070819265));
#18698=CARTESIAN_POINT('Ctrl Pts',(16.8656822982862,-16.8505361109838,1.86063527960074));
#18699=CARTESIAN_POINT('Ctrl Pts',(16.6808880142321,-17.0147683442417,1.87122813441674));
#18700=CARTESIAN_POINT('Ctrl Pts',(16.2508692359186,-17.2692093625704,1.89308411408813));
#18701=CARTESIAN_POINT('Ctrl Pts',(16.0078314830718,-17.3536533130298,1.90413830670727));
#18702=CARTESIAN_POINT('Ctrl Pts',(15.5157961733657,-17.4202150896715,1.92423436821581));
#18703=CARTESIAN_POINT('Ctrl Pts',(15.2722443557045,-17.4067271094536,1.93309049077355));
#18704=CARTESIAN_POINT('Ctrl Pts',(14.7972739297611,-17.2879096009912,1.95368301960753));
#18705=CARTESIAN_POINT('Ctrl Pts',(14.570890814878,-17.1814260816023,1.96458832530181));
#18706=CARTESIAN_POINT('Ctrl Pts',(14.1680048503673,-16.8850910700194,1.98633272538432));
#18707=CARTESIAN_POINT('Ctrl Pts',(13.9964409246613,-16.6966722393834,1.99695337863682));
#18708=CARTESIAN_POINT('Ctrl Pts',(13.7423247716212,-16.2732439435685,2.01584161975457));
#18709=CARTESIAN_POINT('Ctrl Pts',(13.6585371841348,-16.0444166518227,2.025684748389));
#18710=CARTESIAN_POINT('Ctrl Pts',(13.6032339797595,-15.7045935164027,2.04055015238812));
#18711=CARTESIAN_POINT('Ctrl Pts',(13.595,-15.6022612357987,2.04502663010489));
#18712=CARTESIAN_POINT('Ctrl Pts',(13.595,-15.5,2.04949999999985));
#18713=CARTESIAN_POINT('Ctrl Pts',(13.595,-15.5,2.1119999999999));
#18714=CARTESIAN_POINT('Ctrl Pts',(13.595,-15.5760950455545,2.10867125784966));
#18715=CARTESIAN_POINT('Ctrl Pts',(13.5995592844064,-15.6522763870644,2.10533874072324));
#18716=CARTESIAN_POINT('Ctrl Pts',(13.6377365927073,-15.9687770978132,2.09149356527491));
#18717=CARTESIAN_POINT('Ctrl Pts',(13.7124302046239,-16.201708256264,2.08130410077575));
#18718=CARTESIAN_POINT('Ctrl Pts',(13.9499183283314,-16.6357575783573,2.06231681634471));
#18719=CARTESIAN_POINT('Ctrl Pts',(14.1138443305959,-16.8309084290227,2.05206963293043));
#18720=CARTESIAN_POINT('Ctrl Pts',(14.5054536833703,-17.1437127897055,2.03039221262406));
#18721=CARTESIAN_POINT('Ctrl Pts',(14.7283790660537,-17.2594087386999,2.01941640251692));
#18722=CARTESIAN_POINT('Ctrl Pts',(15.1987964301296,-17.396436622578,1.99859805913941));
#18723=CARTESIAN_POINT('Ctrl Pts',(15.4410363979128,-17.4192983143245,1.9895465063196));
#18724=CARTESIAN_POINT('Ctrl Pts',(15.9324172665455,-17.3723715040461,1.96990469878203));
#18725=CARTESIAN_POINT('Ctrl Pts',(16.1764500136759,-17.2986537031364,1.95904741711863));
#18726=CARTESIAN_POINT('Ctrl Pts',(16.6158314577467,-17.0634689885345,1.93725792237594));
#18727=CARTESIAN_POINT('Ctrl Pts',(16.8081666912994,-16.9064950156484,1.92653814176603));
#18728=CARTESIAN_POINT('Ctrl Pts',(17.1215600504422,-16.5292396737189,1.90641415745458));
#18729=CARTESIAN_POINT('Ctrl Pts',(17.240114711357,-16.3128922721586,1.89755959195784));
#18730=CARTESIAN_POINT('Ctrl Pts',(17.391494001895,-15.8393168702794,1.87684325766741));
#18731=CARTESIAN_POINT('Ctrl Pts',(17.4197738124388,-15.585697583992,1.86574880069946));
#18732=CARTESIAN_POINT('Ctrl Pts',(17.3765599477362,-15.0917486228472,1.84414123459513));
#18733=CARTESIAN_POINT('Ctrl Pts',(17.3091861934115,-14.8557849173145,1.83381911274331));
#18734=CARTESIAN_POINT('Ctrl Pts',(17.0850557933772,-14.4135186118599,1.81447238022123));
#18735=CARTESIAN_POINT('Ctrl Pts',(16.9271628563678,-14.213112801465,1.80458598817505));
#18736=CARTESIAN_POINT('Ctrl Pts',(16.5447253469805,-13.887597868733,1.78297802383317));
#18737=CARTESIAN_POINT('Ctrl Pts',(16.3247639331751,-13.764760137355,1.7719582933915));
#18738=CARTESIAN_POINT('Ctrl Pts',(15.8580547995251,-13.6134845740593,1.75096880312173));
#18739=CARTESIAN_POINT('Ctrl Pts',(15.6167232944308,-13.5833630154329,1.74167645802588));
#18740=CARTESIAN_POINT('Ctrl Pts',(15.1243063238811,-13.6154313613421,1.72232038721637));
#18741=CARTESIAN_POINT('Ctrl Pts',(14.8781909936369,-13.6817382234719,1.71154630325674));
#18742=CARTESIAN_POINT('Ctrl Pts',(14.4312911303674,-13.9038391283785,1.68975815421944));
#18743=CARTESIAN_POINT('Ctrl Pts',(14.233801553833,-14.0554860364106,1.67895962209881));
#18744=CARTESIAN_POINT('Ctrl Pts',(13.9099371458213,-14.4230295546759,1.65865137346135));
#18745=CARTESIAN_POINT('Ctrl Pts',(13.7855910418598,-14.6345714678699,1.64985776605983));
#18746=CARTESIAN_POINT('Ctrl Pts',(13.6318995591178,-15.0683505290783,1.63088230406471));
#18747=CARTESIAN_POINT('Ctrl Pts',(13.595,-15.2835320441008,1.6214692894093));
#18748=CARTESIAN_POINT('Ctrl Pts',(13.595,-15.5,1.61199999999989));
#18749=CARTESIAN_POINT('Origin',(15.5,15.5,-1.713));
#18750=CARTESIAN_POINT('',(13.595,15.5,10.6744999999999));
#18751=CARTESIAN_POINT('',(13.5949999999998,15.5000000000002,10.737));
#18752=CARTESIAN_POINT('',(13.595,15.5,-1.713));
#18753=CARTESIAN_POINT('',(14.1407339385615,16.8346987578533,10.7369999999981));
#18754=CARTESIAN_POINT('Ctrl Pts',(13.595,15.5,10.6744999999999));
#18755=CARTESIAN_POINT('Ctrl Pts',(13.595,15.7209850684948,10.6828717709174));
#18756=CARTESIAN_POINT('Ctrl Pts',(13.6334494343469,15.9405414658973,10.6920303944907));
#18757=CARTESIAN_POINT('Ctrl Pts',(13.7553915464664,16.2771811332396,10.7074507601906));
#18758=CARTESIAN_POINT('Ctrl Pts',(13.8155629219042,16.4001887992413,10.7134268516752));
#18759=CARTESIAN_POINT('Ctrl Pts',(13.9608604619492,16.6307356506883,10.7253388464319));
#18760=CARTESIAN_POINT('Ctrl Pts',(14.0454618665887,16.7376730482912,10.7312404739585));
#18761=CARTESIAN_POINT('Ctrl Pts',(14.1407339385603,16.8346987578544,10.7369999999991));
#18762=CARTESIAN_POINT('Origin',(15.5,15.5,10.737));
#18763=CARTESIAN_POINT('Origin',(15.5,15.5,-1.713));
#18764=CARTESIAN_POINT('',(13.595,15.5,10.1744999999999));
#18765=CARTESIAN_POINT('',(13.595,15.5,10.2370000000001));
#18766=CARTESIAN_POINT('',(13.595,15.5,-1.713));
#18767=CARTESIAN_POINT('Ctrl Pts',(13.595,15.5,10.1744999999999));
#18768=CARTESIAN_POINT('Ctrl Pts',(13.595,15.5074209450671,10.1747811341621));
#18769=CARTESIAN_POINT('Ctrl Pts',(13.5950433625137,15.514843711189,10.1750632857494));
#18770=CARTESIAN_POINT('Ctrl Pts',(13.5980800374719,15.7746106576663,10.1849706834831));
#18771=CARTESIAN_POINT('Ctrl Pts',(13.6511424766741,16.0238416218886,10.1955731141929));
#18772=CARTESIAN_POINT('Ctrl Pts',(13.8495251796916,16.4830731774224,10.21730966471));
#18773=CARTESIAN_POINT('Ctrl Pts',(13.9913508552489,16.6893210098465,10.2282251809013));
#18774=CARTESIAN_POINT('Ctrl Pts',(14.3415677125539,17.0314906605524,10.248847929745));
#18775=CARTESIAN_POINT('Ctrl Pts',(14.5449657800694,17.1659329264404,10.2577224750685));
#18776=CARTESIAN_POINT('Ctrl Pts',(15.0033973280684,17.3567117327104,10.2777763485593));
#18777=CARTESIAN_POINT('Ctrl Pts',(15.2559823434613,17.4064182514367,10.2888255618311));
#18778=CARTESIAN_POINT('Ctrl Pts',(15.7558831752725,17.4035758694502,10.3106934897319));
#18779=CARTESIAN_POINT('Ctrl Pts',(15.998396076538,17.3549109351872,10.3213021030856));
#18780=CARTESIAN_POINT('Ctrl Pts',(16.4530034996812,17.1678069519007,10.3411886920245));
#18781=CARTESIAN_POINT('Ctrl Pts',(16.6605842725638,17.0306357150664,10.3502315276944));
#18782=CARTESIAN_POINT('Ctrl Pts',(17.0156818941415,16.6811397631114,10.3712385786));
#18783=CARTESIAN_POINT('Ctrl Pts',(17.1583113324512,16.4707625120934,10.3823281132857));
#18784=CARTESIAN_POINT('Ctrl Pts',(17.3498707313289,16.0154567071911,10.40376670003));
#18785=CARTESIAN_POINT('Ctrl Pts',(17.4003765835231,15.7762422294572,10.4139337490575));
#18786=CARTESIAN_POINT('Ctrl Pts',(17.4091960808239,15.2816903031459,10.4328621952661));
#18787=CARTESIAN_POINT('Ctrl Pts',(17.3635304005437,15.030965887023,10.4431758642524));
#18788=CARTESIAN_POINT('Ctrl Pts',(17.178463764648,14.5653277698759,10.4648638675931));
#18789=CARTESIAN_POINT('Ctrl Pts',(17.042265077244,14.3544540576283,10.4758315550602));
#18790=CARTESIAN_POINT('Ctrl Pts',(16.7017070840868,14.0022956793364,10.4966214543749));
#18791=CARTESIAN_POINT('Ctrl Pts',(16.5026187900325,13.8623302617467,10.5056409103224));
#18792=CARTESIAN_POINT('Ctrl Pts',(16.0525428529262,13.6594950881445,10.5253292715256));
#18793=CARTESIAN_POINT('Ctrl Pts',(15.8040539415988,13.6025560456482,10.5361993026423));
#18794=CARTESIAN_POINT('Ctrl Pts',(15.3059850971027,13.5890276321658,10.5579870911154));
#18795=CARTESIAN_POINT('Ctrl Pts',(15.0612475636335,13.6299820743873,10.5686930199636));
#18796=CARTESIAN_POINT('Ctrl Pts',(14.6019183707757,13.8022488761935,10.5887861605086));
#18797=CARTESIAN_POINT('Ctrl Pts',(14.3915034254768,13.931514419436,10.5976583521008));
#18798=CARTESIAN_POINT('Ctrl Pts',(14.025272378736,14.2679294749982,10.6184133611866));
#18799=CARTESIAN_POINT('Ctrl Pts',(13.8750960478184,14.4740872298914,10.6295081126469));
#18800=CARTESIAN_POINT('Ctrl Pts',(13.6678872424595,14.9242804268043,10.6510953019652));
#18801=CARTESIAN_POINT('Ctrl Pts',(13.6094446156002,15.1624912483007,10.6613979238507));
#18802=CARTESIAN_POINT('Ctrl Pts',(13.5957842176475,15.4368541821284,10.6720906390531));
#18803=CARTESIAN_POINT('Ctrl Pts',(13.595,15.468441018576,10.6733044234631));
#18804=CARTESIAN_POINT('Ctrl Pts',(13.595,15.5,10.6744999999999));
#18805=CARTESIAN_POINT('Ctrl Pts',(13.595,15.5000000000014,10.7370000000001));
#18806=CARTESIAN_POINT('Ctrl Pts',(13.5949999999998,15.2615050818091,10.7279648881091));
#18807=CARTESIAN_POINT('Ctrl Pts',(13.639785942239,15.0250626381517,10.7180279618685));
#18808=CARTESIAN_POINT('Ctrl Pts',(13.8168676826068,14.574636639808,10.6970909003079));
#18809=CARTESIAN_POINT('Ctrl Pts',(13.9499258686807,14.3657577230364,10.6862674733056));
#18810=CARTESIAN_POINT('Ctrl Pts',(14.2901813294418,14.0076280664949,10.6652579758955));
#18811=CARTESIAN_POINT('Ctrl Pts',(14.4950326130465,13.8626655490992,10.6559618279509));
#18812=CARTESIAN_POINT('Ctrl Pts',(14.9449917262885,13.6613318768111,10.6362785771528));
#18813=CARTESIAN_POINT('Ctrl Pts',(15.1851520886087,13.6053793669476,10.6257728745141));
#18814=CARTESIAN_POINT('Ctrl Pts',(15.68313769875,13.5868855646606,10.6039887270888));
#18815=CARTESIAN_POINT('Ctrl Pts',(15.9363279765729,13.6283219440909,10.5929130368953));
#18816=CARTESIAN_POINT('Ctrl Pts',(16.4007383128052,13.803977489042,10.5725976241117));
#18817=CARTESIAN_POINT('Ctrl Pts',(16.6090638072585,13.9322622441969,10.5638009107335));
#18818=CARTESIAN_POINT('Ctrl Pts',(16.9699032308363,14.2632679249879,10.5433687567462));
#18819=CARTESIAN_POINT('Ctrl Pts',(17.117795172942,14.4642146921968,10.5325213824564));
#18820=CARTESIAN_POINT('Ctrl Pts',(17.330768674431,14.9160524890345,10.5107458023516));
#18821=CARTESIAN_POINT('Ctrl Pts',(17.391950434512,15.1634645000593,10.5000346926933));
#18822=CARTESIAN_POINT('Ctrl Pts',(17.413810480885,15.6565045081774,10.4808782974484));
#18823=CARTESIAN_POINT('Ctrl Pts',(17.3786636876491,15.8972629623921,10.4713741043925));
#18824=CARTESIAN_POINT('Ctrl Pts',(17.2174690866306,16.3613107883679,10.4502684829413));
#18825=CARTESIAN_POINT('Ctrl Pts',(17.0897011795524,16.5790769712636,10.4392240822409));
#18826=CARTESIAN_POINT('Ctrl Pts',(16.7567467648068,16.9534780470537,10.4177578508231));
#18827=CARTESIAN_POINT('Ctrl Pts',(16.5545706118485,17.1061977053063,10.4081316978063));
#18828=CARTESIAN_POINT('Ctrl Pts',(16.1092301033711,17.3213262050678,10.388650485712));
#18829=CARTESIAN_POINT('Ctrl Pts',(15.8715479691291,17.3842299432809,10.3782531920006));
#18830=CARTESIAN_POINT('Ctrl Pts',(15.3758649154132,17.4177404610146,10.3565697688284));
#18831=CARTESIAN_POINT('Ctrl Pts',(15.1223361573197,17.3842822988696,10.345479271974));
#18832=CARTESIAN_POINT('Ctrl Pts',(14.6523183795208,17.2233098897233,10.3249185642837));
#18833=CARTESIAN_POINT('Ctrl Pts',(14.4391556307392,17.1009279013749,10.3161129504634));
#18834=CARTESIAN_POINT('Ctrl Pts',(14.0682979998266,16.7806204218859,10.2958669649115));
#18835=CARTESIAN_POINT('Ctrl Pts',(13.9148176649309,16.5848707484272,10.2850942458631));
#18836=CARTESIAN_POINT('Ctrl Pts',(13.6882320520984,16.1404884866467,10.2633033826038));
#18837=CARTESIAN_POINT('Ctrl Pts',(13.619393625544,15.8950567334125,10.2524998241403));
#18838=CARTESIAN_POINT('Ctrl Pts',(13.5967962139983,15.5955738319869,10.2406599944637));
#18839=CARTESIAN_POINT('Ctrl Pts',(13.595,15.5477624964957,10.2388094284915));
#18840=CARTESIAN_POINT('Ctrl Pts',(13.595,15.5000000000001,10.2370000000001));
#18841=CARTESIAN_POINT('Origin',(15.5,15.5,-1.713));
#18842=CARTESIAN_POINT('',(13.595,15.5,9.6744999999999));
#18843=CARTESIAN_POINT('',(13.595,15.5,9.73700000000006));
#18844=CARTESIAN_POINT('',(13.595,15.5,-1.713));
#18845=CARTESIAN_POINT('Ctrl Pts',(13.595,15.5000000000001,9.6744999999999));
#18846=CARTESIAN_POINT('Ctrl Pts',(13.595,15.5467420728766,9.67627077088952));
#18847=CARTESIAN_POINT('Ctrl Pts',(13.5967202853277,15.5935315793058,9.67808096528403));
#18848=CARTESIAN_POINT('Ctrl Pts',(13.6187597648754,15.8920261509568,9.68987114996099));
#18849=CARTESIAN_POINT('Ctrl Pts',(13.6872020874657,16.1375667551881,9.70067016843079));
#18850=CARTESIAN_POINT('Ctrl Pts',(13.9130870394511,16.582346386742,9.72246076055695));
#18851=CARTESIAN_POINT('Ctrl Pts',(14.0662814409298,16.7783697126165,9.73323759260773));
#18852=CARTESIAN_POINT('Ctrl Pts',(14.4366202357196,17.0992349697923,9.75349336081863));
#18853=CARTESIAN_POINT('Ctrl Pts',(14.6495282078216,17.2219253191499,9.76229650952821));
#18854=CARTESIAN_POINT('Ctrl Pts',(15.1192565164498,17.3836681050642,9.7828445545251));
#18855=CARTESIAN_POINT('Ctrl Pts',(15.3727735533347,17.4175433890708,9.79393453864082));
#18856=CARTESIAN_POINT('Ctrl Pts',(15.8685880727844,17.3848159770126,9.81562371272001));
#18857=CARTESIAN_POINT('Ctrl Pts',(16.1064048590934,17.3222737366833,9.82602689672305));
#18858=CARTESIAN_POINT('Ctrl Pts',(16.5519903024088,17.1078685429527,9.84551882337728));
#18859=CARTESIAN_POINT('Ctrl Pts',(16.7543077408873,16.955560712628,9.8551256043988));
#18860=CARTESIAN_POINT('Ctrl Pts',(17.0878528289383,16.5818048170048,9.87658031325489));
#18861=CARTESIAN_POINT('Ctrl Pts',(17.2160137186657,16.3642189675569,9.8876264776464));
#18862=CARTESIAN_POINT('Ctrl Pts',(17.3780022600017,15.900387077464,9.90874128388326));
#18863=CARTESIAN_POINT('Ctrl Pts',(17.4135504472185,15.6596724374698,9.91826397153366));
#18864=CARTESIAN_POINT('Ctrl Pts',(17.392502729278,15.1665858676451,9.93740436325299));
#18865=CARTESIAN_POINT('Ctrl Pts',(17.3317298104215,14.9190754039315,9.94811026039677));
#18866=CARTESIAN_POINT('Ctrl Pts',(17.1194871886625,14.4668527863303,9.9698844330078));
#18867=CARTESIAN_POINT('Ctrl Pts',(16.9718972706699,14.2656339594174,9.9807355080219));
#18868=CARTESIAN_POINT('Ctrl Pts',(16.6115925344041,13.9340618991594,10.0011774238356));
#18869=CARTESIAN_POINT('Ctrl Pts',(16.403519949665,13.805464868694,10.0099759427094));
#18870=CARTESIAN_POINT('Ctrl Pts',(15.9394099046984,13.6290372471708,10.0302782193921));
#18871=CARTESIAN_POINT('Ctrl Pts',(15.686244186523,13.5871798170603,10.0413528352353));
#18872=CARTESIAN_POINT('Ctrl Pts',(15.1881494751231,13.6048788651152,10.063141755244));
#18873=CARTESIAN_POINT('Ctrl Pts',(14.9478640205276,13.6604623627683,10.0736529299857));
#18874=CARTESIAN_POINT('Ctrl Pts',(14.4976649285535,13.8610700940611,10.0933466785409));
#18875=CARTESIAN_POINT('Ctrl Pts',(14.2926738275613,14.0056300238769,10.1026277657149));
#18876=CARTESIAN_POINT('Ctrl Pts',(13.9480585027388,14.3670999545861,10.1238591657634));
#18877=CARTESIAN_POINT('Ctrl Pts',(13.8124947693485,14.5811379852324,10.1349328419931));
#18878=CARTESIAN_POINT('Ctrl Pts',(13.6381189944803,15.033858197244,10.1558976316625));
#18879=CARTESIAN_POINT('Ctrl Pts',(13.595,15.2659883514768,10.1656347317408));
#18880=CARTESIAN_POINT('Ctrl Pts',(13.595,15.5,10.1744999999999));
#18881=CARTESIAN_POINT('Ctrl Pts',(13.595,15.5000000000001,10.2370000000001));
#18882=CARTESIAN_POINT('Ctrl Pts',(13.595,15.3073914717115,10.2297032424111));
#18883=CARTESIAN_POINT('Ctrl Pts',(13.6242072503768,15.1156254204738,10.2217995723699));
#18884=CARTESIAN_POINT('Ctrl Pts',(13.7563026575638,14.6933503455336,10.2029129299431));
#18885=CARTESIAN_POINT('Ctrl Pts',(13.876702471396,14.4723487585835,10.191907116492));
#18886=CARTESIAN_POINT('Ctrl Pts',(14.1985172362278,14.0859758557941,10.1702309952512));
#18887=CARTESIAN_POINT('Ctrl Pts',(14.3980477346431,13.9255193647073,10.1602043860612));
#18888=CARTESIAN_POINT('Ctrl Pts',(14.8387924057178,13.6969847837616,10.1409242167228));
#18889=CARTESIAN_POINT('Ctrl Pts',(15.0738870635064,13.6274442067412,10.1306401109577));
#18890=CARTESIAN_POINT('Ctrl Pts',(15.56692222814,13.5795131523613,10.1090725184541));
#18891=CARTESIAN_POINT('Ctrl Pts',(15.8205486951867,13.6052689140877,10.0979777473671));
#18892=CARTESIAN_POINT('Ctrl Pts',(16.295833937723,13.7519510936001,10.0771866168975));
#18893=CARTESIAN_POINT('Ctrl Pts',(16.5137486247078,13.8686392930067,10.0682959537461));
#18894=CARTESIAN_POINT('Ctrl Pts',(16.8940946558731,14.1786684817262,10.0482318168726));
#18895=CARTESIAN_POINT('Ctrl Pts',(17.0527343919501,14.3693281260121,10.0375390800631));
#18896=CARTESIAN_POINT('Ctrl Pts',(17.2920447174216,14.8062273800874,10.01575338384));
#18897=CARTESIAN_POINT('Ctrl Pts',(17.3681155553099,15.0495466867222,10.0048716638172));
#18898=CARTESIAN_POINT('Ctrl Pts',(17.4197882995062,15.5405632028496,9.98513985503588));
#18899=CARTESIAN_POINT('Ctrl Pts',(17.3992342413671,15.7831117902299,9.97614851785801));
#18900=CARTESIAN_POINT('Ctrl Pts',(17.2667107289173,16.2546744188013,9.95538530823236));
#18901=CARTESIAN_POINT('Ctrl Pts',(17.153285580449,16.4784898498698,9.9444254471957));
#18902=CARTESIAN_POINT('Ctrl Pts',(16.844516347237,16.8729562072233,9.9227280498636));
#18903=CARTESIAN_POINT('Ctrl Pts',(16.6510136236391,17.0387811643789,9.91235055221528));
#18904=CARTESIAN_POINT('Ctrl Pts',(16.2195750707347,17.2804205377355,9.89347747466042));
#18905=CARTESIAN_POINT('Ctrl Pts',(15.9876402100024,17.3573822248701,9.88333159273864));
#18906=CARTESIAN_POINT('Ctrl Pts',(15.4981071703884,17.4215380171854,9.86191719905476));
#18907=CARTESIAN_POINT('Ctrl Pts',(15.2446427666752,17.4044974603097,9.85082951735254));
#18908=CARTESIAN_POINT('Ctrl Pts',(14.7635771823721,17.2741564925379,9.8297855285379));
#18909=CARTESIAN_POINT('Ctrl Pts',(14.5401712432681,17.1639326964274,9.8207092566462));
#18910=CARTESIAN_POINT('Ctrl Pts',(14.1492794869322,16.8655004954172,9.8008537997105));
#18911=CARTESIAN_POINT('Ctrl Pts',(13.9850701162271,16.6806814457249,9.79026050673195));
#18912=CARTESIAN_POINT('Ctrl Pts',(13.7306849843362,16.2506215088065,9.76840419017609));
#18913=CARTESIAN_POINT('Ctrl Pts',(13.64627406536,16.0075682104305,9.75735013110541));
#18914=CARTESIAN_POINT('Ctrl Pts',(13.6007088250896,15.6703770935448,9.74357940961421));
#18915=CARTESIAN_POINT('Ctrl Pts',(13.595,15.5851515525511,9.74022587085224));
#18916=CARTESIAN_POINT('Ctrl Pts',(13.595,15.5,9.73700000000006));
#18917=CARTESIAN_POINT('Origin',(15.5,15.5,-1.713));
#18918=CARTESIAN_POINT('',(13.595,15.5,9.17449999999989));
#18919=CARTESIAN_POINT('',(13.595,15.5,9.23700000000004));
#18920=CARTESIAN_POINT('',(13.595,15.5,-1.713));
#18921=CARTESIAN_POINT('Ctrl Pts',(13.595,15.5,9.17449999999989));
#18922=CARTESIAN_POINT('Ctrl Pts',(13.595,15.5841182662493,9.17768672596201));
#18923=CARTESIAN_POINT('Ctrl Pts',(13.6005711245743,15.6683109452453,9.18099812408572));
#18924=CARTESIAN_POINT('Ctrl Pts',(13.6454546573156,16.0045874721858,9.1947192868765));
#18925=CARTESIAN_POINT('Ctrl Pts',(13.7294915060449,16.2478164334572,9.20577181897456));
#18926=CARTESIAN_POINT('Ctrl Pts',(13.9832436140053,16.6783417574239,9.22763192052782));
#18927=CARTESIAN_POINT('Ctrl Pts',(14.1471939492586,16.86344093734,9.2382301602327));
#18928=CARTESIAN_POINT('Ctrl Pts',(14.5375874579699,17.1624251842472,9.25809563300211));
#18929=CARTESIAN_POINT('Ctrl Pts',(14.7607289180441,17.2729579775885,9.26716093254761));
#18930=CARTESIAN_POINT('Ctrl Pts',(15.241523528774,17.4040821001499,9.28819306775017));
#18931=CARTESIAN_POINT('Ctrl Pts',(15.4950022472308,17.4215378340722,9.29928137564419));
#18932=CARTESIAN_POINT('Ctrl Pts',(15.9847143678794,17.3581527301986,9.32070360314416));
#18933=CARTESIAN_POINT('Ctrl Pts',(16.2168053712309,17.28154242915,9.33085631545177));
#18934=CARTESIAN_POINT('Ctrl Pts',(16.6486518981535,17.040545852793,9.34974723963913));
#18935=CARTESIAN_POINT('Ctrl Pts',(16.8424117059181,16.8750147420928,9.36010403130906));
#18936=CARTESIAN_POINT('Ctrl Pts',(17.1518091946145,16.4809894807787,9.38179845958465));
#18937=CARTESIAN_POINT('Ctrl Pts',(17.2655874061658,16.2573107967103,9.39276086240461));
#18938=CARTESIAN_POINT('Ctrl Pts',(17.3988105199629,15.7859252111179,9.41353266682281));
#18939=CARTESIAN_POINT('Ctrl Pts',(17.4197234276662,15.5434252388177,9.42253284891444));
#18940=CARTESIAN_POINT('Ctrl Pts',(17.3687893392891,15.0523509285774,9.44225069108431));
#18941=CARTESIAN_POINT('Ctrl Pts',(17.2930842421058,14.8089190591844,9.4531286758427));
#18942=CARTESIAN_POINT('Ctrl Pts',(17.0544142628338,14.3716309506468,9.4749150975576));
#18943=CARTESIAN_POINT('Ctrl Pts',(16.8960326259638,14.1807096144753,9.48561210305558));
#18944=CARTESIAN_POINT('Ctrl Pts',(16.5161672691566,13.8701561909454,9.5056855865382));
#18945=CARTESIAN_POINT('Ctrl Pts',(16.2984975738922,13.7531769261292,9.51457009738001));
#18946=CARTESIAN_POINT('Ctrl Pts',(15.8234778340686,13.6057615265908,9.53534961355776));
#18947=CARTESIAN_POINT('Ctrl Pts',(15.5698508909803,13.5796122840123,9.54644440546888));
#18948=CARTESIAN_POINT('Ctrl Pts',(15.0766703107743,13.6268085008889,9.56801835910867));
#18949=CARTESIAN_POINT('Ctrl Pts',(14.8414388165919,13.696011803256,9.57830845071767));
#18950=CARTESIAN_POINT('Ctrl Pts',(14.4004559035201,13.9238590409404,9.59759904184063));
#18951=CARTESIAN_POINT('Ctrl Pts',(14.2007883583779,14.0839140324855,9.60760321080475));
#18952=CARTESIAN_POINT('Ctrl Pts',(13.878393475411,14.4696726411921,9.62926874870289));
#18953=CARTESIAN_POINT('Ctrl Pts',(13.757612094652,14.6905133848896,9.64027681452144));
#18954=CARTESIAN_POINT('Ctrl Pts',(13.6245198828295,15.1135898960811,9.65921562083584));
#18955=CARTESIAN_POINT('Ctrl Pts',(13.595,15.3063635593616,9.66716430110702));
#18956=CARTESIAN_POINT('Ctrl Pts',(13.595,15.5000000000001,9.6744999999999));
#18957=CARTESIAN_POINT('Ctrl Pts',(13.595,15.5,9.73700000000006));
#18958=CARTESIAN_POINT('Ctrl Pts',(13.595,15.3443757211123,9.73110434912681));
#18959=CARTESIAN_POINT('Ctrl Pts',(13.6140670739429,15.1890304985196,9.72480222987521));
#18960=CARTESIAN_POINT('Ctrl Pts',(13.7121890711489,14.7970217199471,9.70780526752377));
#18961=CARTESIAN_POINT('Ctrl Pts',(13.8187062227913,14.5706504960066,9.69689967669088));
#18962=CARTESIAN_POINT('Ctrl Pts',(14.1151014095004,14.1678047697919,9.6751554848246));
#18963=CARTESIAN_POINT('Ctrl Pts',(14.3035448501051,13.996268204494,9.66453532981459));
#18964=CARTESIAN_POINT('Ctrl Pts',(14.7270117474889,13.7422119691238,9.64564851430658));
#18965=CARTESIAN_POINT('Ctrl Pts',(14.9558538037295,13.6584568971322,9.63580342065923));
#18966=CARTESIAN_POINT('Ctrl Pts',(15.4418092917676,13.5794459199939,9.61454552529446));
#18967=CARTESIAN_POINT('Ctrl Pts',(15.6948672237038,13.5884707586786,9.60347562450985));
#18968=CARTESIAN_POINT('Ctrl Pts',(16.1810763955832,13.7035882433432,9.5822066318642));
#18969=CARTESIAN_POINT('Ctrl Pts',(16.4096474213849,13.807815216395,9.57287713472466));
#18970=CARTESIAN_POINT('Ctrl Pts',(16.8100863417348,14.095589413607,9.55321662617198));
#18971=CARTESIAN_POINT('Ctrl Pts',(16.9791766790479,14.274963944393,9.54272283487236));
#18972=CARTESIAN_POINT('Ctrl Pts',(17.2455523762227,14.6959189485245,9.52094918762759));
#18973=CARTESIAN_POINT('Ctrl Pts',(17.3370759939428,14.9354953543987,9.50987127588242));
#18974=CARTESIAN_POINT('Ctrl Pts',(17.418928531162,15.4252402763329,9.48952753955791));
#18975=CARTESIAN_POINT('Ctrl Pts',(17.4128512668343,15.6699345949103,9.48073394388639));
#18976=CARTESIAN_POINT('Ctrl Pts',(17.3082478230082,16.1483207371468,9.46032290828238));
#18977=CARTESIAN_POINT('Ctrl Pts',(17.2090037796179,16.3771410728329,9.44948361496211));
#18978=CARTESIAN_POINT('Ctrl Pts',(16.9256979682556,16.7884472787197,9.42770520163259));
#18979=CARTESIAN_POINT('Ctrl Pts',(16.7426508099571,16.9657945748251,9.41698294253947));
#18980=CARTESIAN_POINT('Ctrl Pts',(16.3275606187935,17.2327132985125,9.39779206366632));
#18981=CARTESIAN_POINT('Ctrl Pts',(16.1018343834856,17.3234518195672,9.38832696340719));
#18982=CARTESIAN_POINT('Ctrl Pts',(15.6198137161474,17.4175910477827,9.36724119493223));
#18983=CARTESIAN_POINT('Ctrl Pts',(15.3674280476353,17.4167513457427,9.35620070199646));
#18984=CARTESIAN_POINT('Ctrl Pts',(14.8761442854853,17.3174043597842,9.33470972377469));
#18985=CARTESIAN_POINT('Ctrl Pts',(14.6421797559789,17.2193827662245,9.32504107753166));
#18986=CARTESIAN_POINT('Ctrl Pts',(14.2321180998651,16.9425072991653,9.30558298408394));
#18987=CARTESIAN_POINT('Ctrl Pts',(14.0582734913165,16.7687616740425,9.29519845086315));
#18988=CARTESIAN_POINT('Ctrl Pts',(13.7800955960699,16.3573337764091,9.27352758652369));
#18989=CARTESIAN_POINT('Ctrl Pts',(13.6815178799167,16.1214713095999,9.26243608406818));
#18990=CARTESIAN_POINT('Ctrl Pts',(13.6073102174294,15.7500590608669,9.24674245878719));
#18991=CARTESIAN_POINT('Ctrl Pts',(13.595,15.6250436923898,9.24173713972851));
#18992=CARTESIAN_POINT('Ctrl Pts',(13.595,15.5,9.23700000000004));
#18993=CARTESIAN_POINT('Origin',(15.5,15.5,-1.713));
#18994=CARTESIAN_POINT('',(13.595,15.5,8.67449999999988));
#18995=CARTESIAN_POINT('',(13.595,15.5,8.73700000000004));
#18996=CARTESIAN_POINT('',(13.595,15.5,-1.713));
#18997=CARTESIAN_POINT('Ctrl Pts',(13.595,15.5,8.67449999999988));
#18998=CARTESIAN_POINT('Ctrl Pts',(13.595,15.6239845320393,8.67919701462902));
#18999=CARTESIAN_POINT('Ctrl Pts',(13.6071025749427,15.7479460830675,8.68415786938632));
#19000=CARTESIAN_POINT('Ctrl Pts',(13.6804921932185,16.1184792978077,8.699800300972));
#19001=CARTESIAN_POINT('Ctrl Pts',(13.7787009766107,16.3545427883822,8.71089134959139));
#19002=CARTESIAN_POINT('Ctrl Pts',(14.0562639047011,16.7664816532921,8.73256812062653));
#19003=CARTESIAN_POINT('Ctrl Pts',(14.2298620747682,16.9405275247559,8.74295863817442));
#19004=CARTESIAN_POINT('Ctrl Pts',(14.6394162455077,17.2179817661285,8.76242755798135));
#19005=CARTESIAN_POINT('Ctrl Pts',(14.8730916348169,17.3163350292274,8.77207618699962));
#19006=CARTESIAN_POINT('Ctrl Pts',(15.3641109252586,17.4165246373014,8.79355559603034));
#19007=CARTESIAN_POINT('Ctrl Pts',(15.6165388243955,17.4177984219125,8.80459793632506));
#19008=CARTESIAN_POINT('Ctrl Pts',(16.0987721583091,17.3244613816136,8.82569300779987));
#19009=CARTESIAN_POINT('Ctrl Pts',(16.3246621616815,17.2340962369326,8.83517627677367));
#19010=CARTESIAN_POINT('Ctrl Pts',(16.7402045072762,16.9678646173124,8.85435101512362));
#19011=CARTESIAN_POINT('Ctrl Pts',(16.9235456499428,16.7908244365945,8.86506806959983));
#19012=CARTESIAN_POINT('Ctrl Pts',(17.2075592835694,16.3799609992319,8.88684519081839));
#19013=CARTESIAN_POINT('Ctrl Pts',(17.3071944815201,16.1512661741415,8.89768828474744));
#19014=CARTESIAN_POINT('Ctrl Pts',(17.4125643059193,15.6730612014238,8.91810921942767));
#19015=CARTESIAN_POINT('Ctrl Pts',(17.419043547601,15.4284311150773,8.92690414254867));
#19016=CARTESIAN_POINT('Ctrl Pts',(17.3380201613409,14.9385575085308,8.94723461853481));
#19017=CARTESIAN_POINT('Ctrl Pts',(17.2468774984138,14.6987881849774,8.95831150640485));
#19018=CARTESIAN_POINT('Ctrl Pts',(16.9811417597461,14.2773329934121,8.98009010534563));
#19019=CARTESIAN_POINT('Ctrl Pts',(16.8123106690072,14.0976610775107,8.99058949243603));
#19020=CARTESIAN_POINT('Ctrl Pts',(16.4123868281412,13.8093079629692,9.01026066666552));
#19021=CARTESIAN_POINT('Ctrl Pts',(16.1840991925207,13.7047535905898,9.01957440102707));
#19022=CARTESIAN_POINT('Ctrl Pts',(15.6981649699483,13.5888041447591,9.04083136614396));
#19023=CARTESIAN_POINT('Ctrl Pts',(15.4450785930213,13.57934404525,9.05190251124137));
#19024=CARTESIAN_POINT('Ctrl Pts',(14.9589183093013,13.6575501242183,9.07316936529735));
#19025=CARTESIAN_POINT('Ctrl Pts',(14.7299088508642,13.7409368965763,9.08303684340075));
#19026=CARTESIAN_POINT('Ctrl Pts',(14.3060049856638,13.9943144509653,9.1019075053189));
#19027=CARTESIAN_POINT('Ctrl Pts',(14.1172831377335,14.1655409239974,9.11252200223102));
#19028=CARTESIAN_POINT('Ctrl Pts',(13.8202068842977,14.5679303467204,9.13426380402496));
#19029=CARTESIAN_POINT('Ctrl Pts',(13.713308951115,14.7941665723081,9.14517260915209));
#19030=CARTESIAN_POINT('Ctrl Pts',(13.6143140137655,15.1870326885528,9.16222114395649));
#19031=CARTESIAN_POINT('Ctrl Pts',(13.595,15.3433711822066,9.16856629329937));
#19032=CARTESIAN_POINT('Ctrl Pts',(13.595,15.5,9.17449999999989));
#19033=CARTESIAN_POINT('Ctrl Pts',(13.595,15.5,9.23700000000004));
#19034=CARTESIAN_POINT('Ctrl Pts',(13.595,15.3824179949987,9.23254553791084));
#19035=CARTESIAN_POINT('Ctrl Pts',(13.6058849666647,15.2648292060637,9.2278527399341));
#19036=CARTESIAN_POINT('Ctrl Pts',(13.6730917558932,14.9065985535113,9.2128116095693));
#19037=CARTESIAN_POINT('Ctrl Pts',(13.7650585684708,14.6755697303343,9.20204781971074));
#19038=CARTESIAN_POINT('Ctrl Pts',(14.0351170833788,14.2562762872752,9.18025656727049));
#19039=CARTESIAN_POINT('Ctrl Pts',(14.2126179528575,14.0733257609175,9.16944334600184));
#19040=CARTESIAN_POINT('Ctrl Pts',(14.6192545459505,13.7937119274237,9.14995642650917));
#19041=CARTESIAN_POINT('Ctrl Pts',(14.8420067964181,13.6960615850448,9.14078360470611));
#19042=CARTESIAN_POINT('Ctrl Pts',(15.3200515847365,13.587216811041,9.11987175919784));
#19043=CARTESIAN_POINT('Ctrl Pts',(15.5715317297405,13.5801037207342,9.10887087796406));
#19044=CARTESIAN_POINT('Ctrl Pts',(16.0675652845523,13.6638775132778,9.08717212228549));
#19045=CARTESIAN_POINT('Ctrl Pts',(16.3068900679662,13.7557611321738,9.07709668135702));
#19046=CARTESIAN_POINT('Ctrl Pts',(16.7262000522004,14.0220092773353,9.05783891016115));
#19047=CARTESIAN_POINT('Ctrl Pts',(16.9044493669819,14.1902202450991,9.04756771030684));
#19048=CARTESIAN_POINT('Ctrl Pts',(17.1936824006456,14.5921752325474,9.02601391559381));
#19049=CARTESIAN_POINT('Ctrl Pts',(17.2989194857813,14.8242757180613,9.0149192760814));
#19050=CARTESIAN_POINT('Ctrl Pts',(17.4111778468184,15.3089311471049,8.99410330520862));
#19051=CARTESIAN_POINT('Ctrl Pts',(17.4198837561645,15.5561383958149,8.98519880145138));
#19052=CARTESIAN_POINT('Ctrl Pts',(17.3430511693906,16.0408717039469,8.96515472217364));
#19053=CARTESIAN_POINT('Ctrl Pts',(17.2580169539502,16.2737842435358,8.95447120144469));
#19054=CARTESIAN_POINT('Ctrl Pts',(17.0007148280792,16.7002505185199,8.93268722546357));
#19055=CARTESIAN_POINT('Ctrl Pts',(16.8286313095095,16.8883458080266,8.92179759036604));
#19056=CARTESIAN_POINT('Ctrl Pts',(16.4301342785154,17.1799114619574,8.90203592025793));
#19057=CARTESIAN_POINT('Ctrl Pts',(16.2100973155903,17.2841031152121,8.89306287469785));
#19058=CARTESIAN_POINT('Ctrl Pts',(15.73587152622,17.4066006102442,8.87231808951107));
#19059=CARTESIAN_POINT('Ctrl Pts',(15.4854552195119,17.421079061893,8.86136374538563));
#19060=CARTESIAN_POINT('Ctrl Pts',(14.9893112781569,17.3525458909645,8.83966016089943));
#19061=CARTESIAN_POINT('Ctrl Pts',(14.7486837279404,17.2686711336872,8.82923779513071));
#19062=CARTESIAN_POINT('Ctrl Pts',(14.322947778983,17.0172987846112,8.81040302633861));
#19063=CARTESIAN_POINT('Ctrl Pts',(14.1398474340529,16.8555841798672,8.80027183087332));
#19064=CARTESIAN_POINT('Ctrl Pts',(13.8382875093919,16.464872698706,8.77887436671905));
#19065=CARTESIAN_POINT('Ctrl Pts',(13.7255605297403,16.2373180714138,8.76778812097058));
#19066=CARTESIAN_POINT('Ctrl Pts',(13.6168584404567,15.8328625954923,8.75008821889316));
#19067=CARTESIAN_POINT('Ctrl Pts',(13.595,15.6666266500849,8.74331246333868));
#19068=CARTESIAN_POINT('Ctrl Pts',(13.595,15.4999999999999,8.73700000000004));
#19069=CARTESIAN_POINT('Origin',(15.5,15.5,-1.713));
#19070=CARTESIAN_POINT('',(13.595,15.5,8.17449999999987));
#19071=CARTESIAN_POINT('',(13.595,15.5,8.23700000000003));
#19072=CARTESIAN_POINT('',(13.595,15.5,-1.713));
#19073=CARTESIAN_POINT('Ctrl Pts',(13.595,15.4999999999999,8.17449999999987));
#19074=CARTESIAN_POINT('Ctrl Pts',(13.595,15.6655706799604,8.18077245909731));
#19075=CARTESIAN_POINT('Ctrl Pts',(13.6165822658861,15.8307639689365,8.18750267422103));
#19076=CARTESIAN_POINT('Ctrl Pts',(13.7243523871219,16.234417933857,8.20515182770209));
#19077=CARTESIAN_POINT('Ctrl Pts',(13.8367284095049,16.4621933127477,8.21623876014598));
#19078=CARTESIAN_POINT('Ctrl Pts',(14.1377133670211,16.8534461367269,8.23764415663007));
#19079=CARTESIAN_POINT('Ctrl Pts',(14.3205889440629,17.0154718238113,8.24778222091711));
#19080=CARTESIAN_POINT('Ctrl Pts',(14.7459749943083,17.2675188424774,8.26663489573058));
#19081=CARTESIAN_POINT('Ctrl Pts',(14.9864779484859,17.3517629615954,8.27703621821872));
#19082=CARTESIAN_POINT('Ctrl Pts',(15.4825564974726,17.421059699816,8.29873694214642));
#19083=CARTESIAN_POINT('Ctrl Pts',(15.7330319879065,17.4069545259146,8.3096938752363));
#19084=CARTESIAN_POINT('Ctrl Pts',(16.2074545486742,17.28515014628,8.3304472680958));
#19085=CARTESIAN_POINT('Ctrl Pts',(16.4276283590798,17.1812936902314,8.33942874595681));
#19086=CARTESIAN_POINT('Ctrl Pts',(16.8265456288579,16.890338562991,8.35917647852205));
#19087=CARTESIAN_POINT('Ctrl Pts',(16.9989104159136,16.7025028612466,8.37006243140816));
#19088=CARTESIAN_POINT('Ctrl Pts',(17.2568706598939,16.2763945983601,8.39184723903779));
#19089=CARTESIAN_POINT('Ctrl Pts',(17.3422608012701,16.0435736064316,8.4025350764933));
#19090=CARTESIAN_POINT('Ctrl Pts',(17.4197882054961,15.5589940023013,8.42258853009988));
#19091=CARTESIAN_POINT('Ctrl Pts',(17.4114577837839,15.3118539019019,8.43148645707275));
#19092=CARTESIAN_POINT('Ctrl Pts',(17.2999686011362,14.8270604670506,8.45229083246616));
#19093=CARTESIAN_POINT('Ctrl Pts',(17.1950719271862,14.5947614328546,8.46338554820822));
#19094=CARTESIAN_POINT('Ctrl Pts',(16.9064018859139,14.1923105216186,8.48494581651717));
#19095=CARTESIAN_POINT('Ctrl Pts',(16.7283756870393,14.0238112481951,8.49522305845685));
#19096=CARTESIAN_POINT('Ctrl Pts',(16.3095426905112,13.7570112404865,8.514491303543));
#19097=CARTESIAN_POINT('Ctrl Pts',(16.0704985648374,13.664806527007,8.52454380731241));
#19098=CARTESIAN_POINT('Ctrl Pts',(15.5747065379353,13.5802193514064,8.54623199746559));
#19099=CARTESIAN_POINT('Ctrl Pts',(15.323173313475,13.5869204313355,8.55723520063533));
#19100=CARTESIAN_POINT('Ctrl Pts',(14.8449188118345,13.6950026924642,8.57815621995466));
#19101=CARTESIAN_POINT('Ctrl Pts',(14.6220136440858,13.7922913682329,8.58734226249266));
#19102=CARTESIAN_POINT('Ctrl Pts',(14.2149308751917,14.0712423419691,8.60681382916423));
#19103=CARTESIAN_POINT('Ctrl Pts',(14.0371350730656,14.2539037389004,8.61762254793483));
#19104=CARTESIAN_POINT('Ctrl Pts',(13.7663770367188,14.6727893773774,8.63941365127579));
#19105=CARTESIAN_POINT('Ctrl Pts',(13.6740279732215,14.9037081281676,8.65018163185947));
#19106=CARTESIAN_POINT('Ctrl Pts',(13.6060693707565,15.2628498531252,8.66527372103727));
#19107=CARTESIAN_POINT('Ctrl Pts',(13.595,15.3814261510959,8.67000796301933));
#19108=CARTESIAN_POINT('Ctrl Pts',(13.595,15.5,8.67449999999988));
#19109=CARTESIAN_POINT('Ctrl Pts',(13.595,15.4999999999999,8.73700000000004));
#19110=CARTESIAN_POINT('Ctrl Pts',(13.595,15.4206038404396,8.73399216574185));
#19111=CARTESIAN_POINT('Ctrl Pts',(13.5999632283935,15.3411272724663,8.73087272824994));
#19112=CARTESIAN_POINT('Ctrl Pts',(13.6405135877242,15.0190534423791,8.71778439498593));
#19113=CARTESIAN_POINT('Ctrl Pts',(13.7176717851386,14.7842563785789,8.70720174753657));
#19114=CARTESIAN_POINT('Ctrl Pts',(13.9613838186573,14.3482523216224,8.68535368952092));
#19115=CARTESIAN_POINT('Ctrl Pts',(14.1289432061782,14.1531212076419,8.67429646311949));
#19116=CARTESIAN_POINT('Ctrl Pts',(14.520751534431,13.8481574518962,8.65417351806977));
#19117=CARTESIAN_POINT('Ctrl Pts',(14.738122479254,13.7373148446311,8.64532797553569));
#19118=CARTESIAN_POINT('Ctrl Pts',(15.2084251123979,13.6012137520089,8.62475480698168));
#19119=CARTESIAN_POINT('Ctrl Pts',(15.4575681112309,13.5794278792961,8.61385616311321));
#19120=CARTESIAN_POINT('Ctrl Pts',(15.9547523726961,13.632945839073,8.5921070703107));
#19121=CARTESIAN_POINT('Ctrl Pts',(16.1978028064333,13.7095285676326,8.58147494285063));
#19122=CARTESIAN_POINT('Ctrl Pts',(16.6303417949376,13.9477019847125,8.56255372725551));
#19123=CARTESIAN_POINT('Ctrl Pts',(16.8177988743282,14.103306736907,8.5527555734894));
#19124=CARTESIAN_POINT('Ctrl Pts',(17.1304673813216,14.4834153029675,8.53151681898803));
#19125=CARTESIAN_POINT('Ctrl Pts',(17.2499517200763,14.706564354543,8.5204496747679));
#19126=CARTESIAN_POINT('Ctrl Pts',(17.395189508853,15.1848113261174,8.49915514628783));
#19127=CARTESIAN_POINT('Ctrl Pts',(17.4201184911673,15.4350477316951,8.4897913193337));
#19128=CARTESIAN_POINT('Ctrl Pts',(17.3727336093045,15.9260574676149,8.47015355267829));
#19129=CARTESIAN_POINT('Ctrl Pts',(17.3027597345931,16.1623404818524,8.4596717490839));
#19130=CARTESIAN_POINT('Ctrl Pts',(17.0729933111687,16.6041489389338,8.43790881998719));
#19131=CARTESIAN_POINT('Ctrl Pts',(16.9120375361652,16.8036935141921,8.42682883053564));
#19132=CARTESIAN_POINT('Ctrl Pts',(16.5299526739395,17.1208420183918,8.40645695422237));
#19133=CARTESIAN_POINT('Ctrl Pts',(16.3153110648192,17.2387354398894,8.39766540091083));
#19134=CARTESIAN_POINT('Ctrl Pts',(15.8491966228593,17.3889415479785,8.37727544281987));
#19135=CARTESIAN_POINT('Ctrl Pts',(15.6015970664843,17.4182561416708,8.36644431611931));
#19136=CARTESIAN_POINT('Ctrl Pts',(15.1036844451788,17.3803317435638,8.34466336155654));
#19137=CARTESIAN_POINT('Ctrl Pts',(14.8583231569413,17.3113496979315,8.333930146848));
#19138=CARTESIAN_POINT('Ctrl Pts',(14.4188371634068,17.0868927869893,8.3147050377695));
#19139=CARTESIAN_POINT('Ctrl Pts',(14.2268788412801,16.9374741445605,8.30527771422209));
#19140=CARTESIAN_POINT('Ctrl Pts',(13.9030946233503,16.56834393363,8.28421173657838));
#19141=CARTESIAN_POINT('Ctrl Pts',(13.7768778801302,16.3498915663607,8.27317526802272));
#19142=CARTESIAN_POINT('Ctrl Pts',(13.6291678335146,15.9155216662343,8.25348889919258));
#19143=CARTESIAN_POINT('Ctrl Pts',(13.595,15.7083210063564,8.24489200715868));
#19144=CARTESIAN_POINT('Ctrl Pts',(13.595,15.4999999999999,8.23700000000003));
#19145=CARTESIAN_POINT('Origin',(15.5,15.5,-1.713));
#19146=CARTESIAN_POINT('',(13.595,15.5,7.67449999999987));
#19147=CARTESIAN_POINT('',(13.595,15.5000000314704,7.73700000238446));
#19148=CARTESIAN_POINT('',(13.595,15.5,-1.713));
#19149=CARTESIAN_POINT('Ctrl Pts',(13.595,15.4999999999999,7.67449999999987));
#19150=CARTESIAN_POINT('Ctrl Pts',(13.595,15.7072119682429,7.68234999249621));
#19151=CARTESIAN_POINT('Ctrl Pts',(13.6288049256949,15.9133285386797,7.69089787740364));
#19152=CARTESIAN_POINT('Ctrl Pts',(13.7754232237215,16.3469484282891,7.71053195391287));
#19153=CARTESIAN_POINT('Ctrl Pts',(13.9012906536843,16.5656523838065,7.72157031333401));
#19154=CARTESIAN_POINT('Ctrl Pts',(14.2244947448307,16.9353609163451,7.74264551135446));
#19155=CARTESIAN_POINT('Ctrl Pts',(14.4162139638687,17.0851038136441,7.75209028713306));
#19156=CARTESIAN_POINT('Ctrl Pts',(14.8553358061007,17.3102883722132,7.7712994665833));
#19157=CARTESIAN_POINT('Ctrl Pts',(15.1005808635409,17.379674633204,7.78202759683005));
#19158=CARTESIAN_POINT('Ctrl Pts',(15.598467221476,17.4184244187749,7.80380740251403));
#19159=CARTESIAN_POINT('Ctrl Pts',(15.8461540690323,17.3895065864025,7.81464234772649));
#19160=CARTESIAN_POINT('Ctrl Pts',(16.3124930652495,17.2400465688875,7.83504212883837));
#19161=CARTESIAN_POINT('Ctrl Pts',(16.5272782908419,17.1225302803764,7.84383450149611));
#19162=CARTESIAN_POINT('Ctrl Pts',(16.9098853806253,16.8060290372117,7.86419327935274));
#19163=CARTESIAN_POINT('Ctrl Pts',(17.0711961872398,16.6067145422958,7.875272317815));
#19164=CARTESIAN_POINT('Ctrl Pts',(17.3017098565452,16.1652048743794,7.89704027158077));
#19165=CARTESIAN_POINT('Ctrl Pts',(17.3720675968037,15.9289956883797,7.90752767428474));
#19166=CARTESIAN_POINT('Ctrl Pts',(17.4202052599821,15.4381406590471,7.92717604508821));
#19167=CARTESIAN_POINT('Ctrl Pts',(17.3956990415148,15.1879857265255,7.93652374306273));
#19168=CARTESIAN_POINT('Ctrl Pts',(17.2513132939779,14.7095606372835,7.95780638325783));
#19169=CARTESIAN_POINT('Ctrl Pts',(17.1321881203751,14.4861698317101,7.96887483030069));
#19170=CARTESIAN_POINT('Ctrl Pts',(16.8201091168,14.1054851539516,7.99012251637059));
#19171=CARTESIAN_POINT('Ctrl Pts',(16.6328861955586,13.9495538297391,7.99994242364131));
#19172=CARTESIAN_POINT('Ctrl Pts',(16.2007137166297,13.7106660880922,8.0188476064466));
#19173=CARTESIAN_POINT('Ctrl Pts',(15.9577905429681,13.6336887948883,8.02947416697423));
#19174=CARTESIAN_POINT('Ctrl Pts',(15.4606577648512,13.5793570642748,8.05122100766174));
#19175=CARTESIAN_POINT('Ctrl Pts',(15.2114403555342,13.6007481227263,8.06212290658198));
#19176=CARTESIAN_POINT('Ctrl Pts',(14.7409222498438,13.7361122958494,8.08270550088162));
#19177=CARTESIAN_POINT('Ctrl Pts',(14.5234077996986,13.8465909841975,8.09155607566125));
#19178=CARTESIAN_POINT('Ctrl Pts',(14.1310999921285,14.1509212443981,8.11166594618874));
#19179=CARTESIAN_POINT('Ctrl Pts',(13.9632019341827,14.3458182397711,8.12272171075946));
#19180=CARTESIAN_POINT('Ctrl Pts',(13.7187719777927,14.7815102938362,8.1445736514962));
#19181=CARTESIAN_POINT('Ctrl Pts',(13.6412427536576,15.0162246109299,8.1551612793747));
#19182=CARTESIAN_POINT('Ctrl Pts',(13.6000829545093,15.3392233658662,8.1682979822067));
#19183=CARTESIAN_POINT('Ctrl Pts',(13.595,15.4196518696993,8.17145610140027));
#19184=CARTESIAN_POINT('Ctrl Pts',(13.595,15.4999999999999,8.17449999999987));
#19185=CARTESIAN_POINT('Ctrl Pts',(13.595,15.4999999999999,8.23700000000003));
#19186=CARTESIAN_POINT('Ctrl Pts',(13.595,15.4574945914102,8.23538973037462));
#19187=CARTESIAN_POINT('Ctrl Pts',(13.596422573169,15.4149448812192,8.23374666753423));
#19188=CARTESIAN_POINT('Ctrl Pts',(13.6155835759862,15.1294756706011,8.22251289282721));
#19189=CARTESIAN_POINT('Ctrl Pts',(13.6783172687067,14.8919169134681,8.21214111833337));
#19190=CARTESIAN_POINT('Ctrl Pts',(13.8939452341179,14.4447108048819,8.19048294539069));
#19191=CARTESIAN_POINT('Ctrl Pts',(14.0481586353087,14.2409467922808,8.17939057829159));
#19192=CARTESIAN_POINT('Ctrl Pts',(14.4203292232219,13.9116631203642,8.1587758224347));
#19193=CARTESIAN_POINT('Ctrl Pts',(14.6322997021123,13.786641160677,8.14995714338966));
#19194=CARTESIAN_POINT('Ctrl Pts',(15.0941629204617,13.6225082001164,8.12975315308563));
#19195=CARTESIAN_POINT('Ctrl Pts',(15.3400184947618,13.585823183673,8.11899831606461));
#19196=CARTESIAN_POINT('Ctrl Pts',(15.8381693806136,13.6083409191706,8.09720693873075));
#19197=CARTESIAN_POINT('Ctrl Pts',(16.0855752145909,13.669739009931,8.08638428632579));
#19198=CARTESIAN_POINT('Ctrl Pts',(16.5317875257589,13.8805701034552,8.06686493763077));
#19199=CARTESIAN_POINT('Ctrl Pts',(16.7282327266091,14.0239920966143,8.05771933408628));
#19200=CARTESIAN_POINT('Ctrl Pts',(17.0626902307113,14.3823785727111,8.03682692180615));
#19201=CARTESIAN_POINT('Ctrl Pts',(17.1952868030276,14.5960761529612,8.0258310416932));
#19202=CARTESIAN_POINT('Ctrl Pts',(17.3724973279344,15.067120882404,8.00411004587214));
#19203=CARTESIAN_POINT('Ctrl Pts',(17.4134713806441,15.3204986080025,7.9939854967544));
#19204=CARTESIAN_POINT('Ctrl Pts',(17.3940618301428,15.8170445447974,7.97474988123996));
#19205=CARTESIAN_POINT('Ctrl Pts',(17.3382739969744,16.0556202551099,7.96449150230556));
#19206=CARTESIAN_POINT('Ctrl Pts',(17.1362886591698,16.507583009347,7.94295152436876));
#19207=CARTESIAN_POINT('Ctrl Pts',(16.9886251887867,16.7151821216971,7.9318571306553));
#19208=CARTESIAN_POINT('Ctrl Pts',(16.6260958189486,17.0559878548847,7.9110167497448));
#19209=CARTESIAN_POINT('Ctrl Pts',(16.4166341910597,17.1878887790938,7.90209773364225));
#19210=CARTESIAN_POINT('Ctrl Pts',(15.9588791758701,17.3651469763034,7.88207345476258));
#19211=CARTESIAN_POINT('Ctrl Pts',(15.7148635545466,17.4087070536214,7.87139910562334));
#19212=CARTESIAN_POINT('Ctrl Pts',(15.216925645497,17.4006884912397,7.84961704486003));
#19213=CARTESIAN_POINT('Ctrl Pts',(14.9678130316258,17.346494933789,7.83871973016752));
#19214=CARTESIAN_POINT('Ctrl Pts',(14.5153907472423,17.1485805966075,7.81892872910089));
#19215=CARTESIAN_POINT('Ctrl Pts',(14.3146715051907,17.0107213240227,7.80997282577612));
#19216=CARTESIAN_POINT('Ctrl Pts',(13.9704168011547,16.6623674964646,7.7892462021458));
#19217=CARTESIAN_POINT('Ctrl Pts',(13.8320529297719,16.4532420018724,7.77829738645955));
#19218=CARTESIAN_POINT('Ctrl Pts',(13.6434492900726,15.9938293223661,7.75676786453815));
#19219=CARTESIAN_POINT('Ctrl Pts',(13.5950000041037,15.7480519480125,7.74639716931276));
#19220=CARTESIAN_POINT('Ctrl Pts',(13.595,15.5000000315158,7.73700000119396));
#19221=CARTESIAN_POINT('Origin',(15.5,15.5,-1.713));
#19222=CARTESIAN_POINT('',(13.595,15.5000000468491,7.17450000354951));
#19223=CARTESIAN_POINT('',(13.595,15.5,7.23700000000002));
#19224=CARTESIAN_POINT('',(13.595,15.5,-1.713));
#19225=CARTESIAN_POINT('Ctrl Pts',(13.595,15.5000000469168,7.17450000177725));
#19226=CARTESIAN_POINT('Ctrl Pts',(13.5950000060854,15.7470883071305,7.1838606629043));
#19227=CARTESIAN_POINT('Ctrl Pts',(13.6430734174731,15.9919359338936,7.1941879144583));
#19228=CARTESIAN_POINT('Ctrl Pts',(13.8306451460201,16.4507838931113,7.21567347235114));
#19229=CARTESIAN_POINT('Ctrl Pts',(13.9687228558569,16.6601426812252,7.22662486709875));
#19230=CARTESIAN_POINT('Ctrl Pts',(14.3124876181408,17.00900205961,7.24735992681755));
#19231=CARTESIAN_POINT('Ctrl Pts',(14.5129894026531,17.1471409984407,7.25632368340536));
#19232=CARTESIAN_POINT('Ctrl Pts',(14.9651005289506,17.3457108331891,7.27610107300719));
#19233=CARTESIAN_POINT('Ctrl Pts',(15.2141319420346,17.4002701330433,7.28699483560931));
#19234=CARTESIAN_POINT('Ctrl Pts',(15.7120908062108,17.4090216060289,7.30877781304487));
#19235=CARTESIAN_POINT('Ctrl Pts',(15.9562040613889,17.3658076341079,7.31945643313142));
#19236=CARTESIAN_POINT('Ctrl Pts',(16.4141694099564,17.1892137068839,7.33948991294629));
#19237=CARTESIAN_POINT('Ctrl Pts',(16.623757886392,17.0576649028473,7.34840208078488));
#19238=CARTESIAN_POINT('Ctrl Pts',(16.9867824147931,16.7174440987839,7.36923113255287));
#19239=CARTESIAN_POINT('Ctrl Pts',(17.1347818420411,16.5100355588719,7.38032565478166));
#19240=CARTESIAN_POINT('Ctrl Pts',(17.3374647859651,16.0583054532881,7.4018720773124));
#19241=CARTESIAN_POINT('Ctrl Pts',(17.3936068432643,15.8197767308892,7.41213642384694));
#19242=CARTESIAN_POINT('Ctrl Pts',(17.4137194975374,15.3233648227343,7.43138234030978));
#19243=CARTESIAN_POINT('Ctrl Pts',(17.3731570345151,15.0700682684394,7.44148395818749));
#19244=CARTESIAN_POINT('Ctrl Pts',(17.1967570875381,14.5988280085548,7.4631946322835));
#19245=CARTESIAN_POINT('Ctrl Pts',(17.0644839078362,14.3848819424175,7.47419285267569));
#19246=CARTESIAN_POINT('Ctrl Pts',(16.7305712796223,14.0259422626678,7.49509430478401));
#19247=CARTESIAN_POINT('Ctrl Pts',(16.5343592960234,13.8822126282349,7.50425243674433));
#19248=CARTESIAN_POINT('Ctrl Pts',(16.0884914737045,13.6706748179657,7.52375671593588));
#19249=CARTESIAN_POINT('Ctrl Pts',(15.8411855178205,13.6088828336564,7.53457499922039));
#19250=CARTESIAN_POINT('Ctrl Pts',(15.3430352235694,13.5855685820084,7.55636635067493));
#19251=CARTESIAN_POINT('Ctrl Pts',(15.0970841547928,13.6218741990355,7.56712536505709));
#19252=CARTESIAN_POINT('Ctrl Pts',(14.6349984075474,13.7852868598577,7.58733908978345));
#19253=CARTESIAN_POINT('Ctrl Pts',(14.4228899770894,13.9099360093728,7.59615438328633));
#19254=CARTESIAN_POINT('Ctrl Pts',(14.0501988550116,14.2385896315513,7.61675665567874));
#19255=CARTESIAN_POINT('Ctrl Pts',(13.8956314460231,14.4421390723225,7.62784863691793));
#19256=CARTESIAN_POINT('Ctrl Pts',(13.6792635784448,14.8890746339752,7.64951274383108));
#19257=CARTESIAN_POINT('Ctrl Pts',(13.6161520545551,15.1265722793911,7.65989046720001));
#19258=CARTESIAN_POINT('Ctrl Pts',(13.5964878424717,15.4130150531057,7.67117213057748));
#19259=CARTESIAN_POINT('Ctrl Pts',(13.595,15.4565304058035,7.67285320328655));
#19260=CARTESIAN_POINT('Ctrl Pts',(13.595,15.4999999999999,7.67449999999987));
#19261=CARTESIAN_POINT('Ctrl Pts',(13.595,15.5000000315158,7.73700000119396));
#19262=CARTESIAN_POINT('Ctrl Pts',(13.5949999999314,15.4958528079258,7.73684288828852));
#19263=CARTESIAN_POINT('Ctrl Pts',(13.5950135427448,15.4917049707995,7.73668545593254));
#19264=CARTESIAN_POINT('Ctrl Pts',(13.596621664402,15.2455180119549,7.72732376646322));
#19265=CARTESIAN_POINT('Ctrl Pts',(13.6443166811126,15.0060107870849,7.71720710638086));
#19266=CARTESIAN_POINT('Ctrl Pts',(13.8303098215743,14.5490220554584,7.69582651053382));
#19267=CARTESIAN_POINT('Ctrl Pts',(13.9702417349155,14.3372148383134,7.68474180417234));
#19268=CARTESIAN_POINT('Ctrl Pts',(14.3213455669013,13.9831176615365,7.6636477942646));
#19269=CARTESIAN_POINT('Ctrl Pts',(14.5279317852933,13.8431252163888,7.65452266905979));
#19270=CARTESIAN_POINT('Ctrl Pts',(14.9808551793442,13.6508243675268,7.63470974718525));
#19271=CARTESIAN_POINT('Ctrl Pts',(15.2225333764069,13.5994849650689,7.6241376475762));
#19272=CARTESIAN_POINT('Ctrl Pts',(15.7217895293589,13.5909093754666,7.60229792085037));
#19273=CARTESIAN_POINT('Ctrl Pts',(15.9746259000064,13.6375917998351,7.59123771216063));
#19274=CARTESIAN_POINT('Ctrl Pts',(16.4352634071348,13.8228499867134,7.57108734002026));
#19275=CARTESIAN_POINT('Ctrl Pts',(16.6404537600255,13.9550341255943,7.56225165420826));
#19276=CARTESIAN_POINT('Ctrl Pts',(16.9945851294045,14.2931114083031,7.54169832087678));
#19277=CARTESIAN_POINT('Ctrl Pts',(17.1386620530399,14.4974314044083,7.53080659870066));
#19278=CARTESIAN_POINT('Ctrl Pts',(17.3424379649764,14.9540000621413,7.5090529673736));
#19279=CARTESIAN_POINT('Ctrl Pts',(17.3984912162882,15.2025942427762,7.49840924465625));
#19280=CARTESIAN_POINT('Ctrl Pts',(17.4101799511541,15.6961858964362,7.47945442057061));
#19281=CARTESIAN_POINT('Ctrl Pts',(17.369989509654,15.9364146114939,7.46970116424717));
#19282=CARTESIAN_POINT('Ctrl Pts',(17.1988041419557,16.3977127086814,7.44848119247419));
#19283=CARTESIAN_POINT('Ctrl Pts',(17.0661099487767,16.6131602536261,7.43741688172641));
#19284=CARTESIAN_POINT('Ctrl Pts',(16.7257736644268,16.9794228970614,7.41609750745491));
#19285=CARTESIAN_POINT('Ctrl Pts',(16.5218223593459,17.1269843255975,7.40669914082883));
#19286=CARTESIAN_POINT('Ctrl Pts',(16.0734117987848,17.3329803183507,7.38708363074307));
#19287=CARTESIAN_POINT('Ctrl Pts',(15.8340676287476,17.3912953159661,7.37661363205379));
#19288=CARTESIAN_POINT('Ctrl Pts',(15.3368116312762,17.414883025994,7.3548614011933));
#19289=CARTESIAN_POINT('Ctrl Pts',(15.0834797431034,17.3761481699676,7.34377951632137));
#19290=CARTESIAN_POINT('Ctrl Pts',(14.6171531313432,17.2054527007769,7.3233802769618));
#19291=CARTESIAN_POINT('Ctrl Pts',(14.4071993495888,17.0791692941371,7.31458969380564));
#19292=CARTESIAN_POINT('Ctrl Pts',(14.0429440084805,16.7517930749219,7.29422032403357));
#19293=CARTESIAN_POINT('Ctrl Pts',(13.8931313169624,16.5525972484919,7.28339727102502));
#19294=CARTESIAN_POINT('Ctrl Pts',(13.6754984349704,16.103249384372,7.26161410801274));
#19295=CARTESIAN_POINT('Ctrl Pts',(13.6117049129581,15.8564836530191,7.2508703567817));
#19296=CARTESIAN_POINT('Ctrl Pts',(13.5959534549509,15.5696266820693,7.23965858280537));
#19297=CARTESIAN_POINT('Ctrl Pts',(13.595,15.5347980724284,7.23831828585853));
#19298=CARTESIAN_POINT('Ctrl Pts',(13.595,15.5,7.23700000000002));
#19299=CARTESIAN_POINT('Origin',(15.5,15.5,-1.713));
#19300=CARTESIAN_POINT('',(13.595,15.5,6.67449999999986));
#19301=CARTESIAN_POINT('',(13.595,15.5,6.73700000000002));
#19302=CARTESIAN_POINT('',(13.595,15.5,-1.713));
#19303=CARTESIAN_POINT('Ctrl Pts',(13.595,15.5,6.67449999999986));
#19304=CARTESIAN_POINT('Ctrl Pts',(13.595,15.5337860699612,6.67577994728247));
#19305=CARTESIAN_POINT('Ctrl Pts',(13.5958988051172,15.5676012636805,6.67708065679041));
#19306=CARTESIAN_POINT('Ctrl Pts',(13.6111380804091,15.8534666090834,6.68824366155095));
#19307=CARTESIAN_POINT('Ctrl Pts',(13.6745367085023,16.1003319863785,6.69898255053165));
#19308=CARTESIAN_POINT('Ctrl Pts',(13.8914661703111,16.5500598413007,6.72076472367497));
#19309=CARTESIAN_POINT('Ctrl Pts',(14.0409894081154,16.7495218496875,6.73159152967911));
#19310=CARTESIAN_POINT('Ctrl Pts',(14.4047282234883,17.0774481133631,6.75197043967901));
#19311=CARTESIAN_POINT('Ctrl Pts',(14.614434389684,17.2040348641911,6.76076134688004));
#19312=CARTESIAN_POINT('Ctrl Pts',(15.0804714953236,17.3754834245413,6.78114792192992));
#19313=CARTESIAN_POINT('Ctrl Pts',(15.3337836813351,17.4146280576722,6.79222894494007));
#19314=CARTESIAN_POINT('Ctrl Pts',(15.8311536453238,17.3918124142706,6.81398616121256));
#19315=CARTESIAN_POINT('Ctrl Pts',(16.0706231306758,17.3338551940679,6.82446164176166));
#19316=CARTESIAN_POINT('Ctrl Pts',(16.5192695723309,17.1285669310391,6.84408747035551));
#19317=CARTESIAN_POINT('Ctrl Pts',(16.723357731448,16.9814015000744,6.85346970837494));
#19318=CARTESIAN_POINT('Ctrl Pts',(17.0642592513022,16.6157687823903,6.87477758159879));
#19319=CARTESIAN_POINT('Ctrl Pts',(17.1973319398078,16.4005046466869,6.88584322264411));
#19320=CARTESIAN_POINT('Ctrl Pts',(17.3692884929086,15.9394217717019,6.90707190853817));
#19321=CARTESIAN_POINT('Ctrl Pts',(17.4098676563665,15.699232024322,6.91684585203433));
#19322=CARTESIAN_POINT('Ctrl Pts',(17.3989594809284,15.2056008222122,6.93578510176519));
#19323=CARTESIAN_POINT('Ctrl Pts',(17.3433005725257,14.9569204724809,6.94642346372892));
#19324=CARTESIAN_POINT('Ctrl Pts',(17.1402345257407,14.4999966777563,6.96817502266233));
#19325=CARTESIAN_POINT('Ctrl Pts',(16.9964533203441,14.295420842877,6.97906996897484));
#19326=CARTESIAN_POINT('Ctrl Pts',(16.6428379287255,13.9568026893442,6.99963250698671));
#19327=CARTESIAN_POINT('Ctrl Pts',(16.4378853679788,13.8243202013929,7.00847264357042));
#19328=CARTESIAN_POINT('Ctrl Pts',(15.9775384842111,13.6383308597002,7.02861030252789));
#19329=CARTESIAN_POINT('Ctrl Pts',(15.7247333891731,13.5912482315457,7.03966914308073));
#19330=CARTESIAN_POINT('Ctrl Pts',(15.2253882367842,13.5990657619463,7.06151276304523));
#19331=CARTESIAN_POINT('Ctrl Pts',(14.9835978859395,13.6500518687448,7.07208976876896));
#19332=CARTESIAN_POINT('Ctrl Pts',(14.5304506110992,13.8416645991434,7.09191248420376));
#19333=CARTESIAN_POINT('Ctrl Pts',(14.3237325854823,13.9812818988211,7.10102603895217));
#19334=CARTESIAN_POINT('Ctrl Pts',(13.972097067769,14.334769301076,7.12210857740915));
#19335=CARTESIAN_POINT('Ctrl Pts',(13.8318063975557,14.5463886664587,7.13319401404347));
#19336=CARTESIAN_POINT('Ctrl Pts',(13.6450737883124,15.0031578759162,7.1545824673977));
#19337=CARTESIAN_POINT('Ctrl Pts',(13.5970057201001,15.2426281300911,7.16470588636848));
#19338=CARTESIAN_POINT('Ctrl Pts',(13.5950204734553,15.4898007705079,7.17411316585421));
#19339=CARTESIAN_POINT('Ctrl Pts',(13.5949999998744,15.4949008690299,7.17430682515208));
#19340=CARTESIAN_POINT('Ctrl Pts',(13.595,15.5000000469168,7.17450000177725));
#19341=CARTESIAN_POINT('Ctrl Pts',(13.595,15.5,7.23700000000002));
#19342=CARTESIAN_POINT('Ctrl Pts',(13.595,15.2942576541637,7.22920568249658));
#19343=CARTESIAN_POINT('Ctrl Pts',(13.628327246639,15.0896374680993,7.22072493435236));
#19344=CARTESIAN_POINT('Ctrl Pts',(13.7733657429176,14.6572925777788,7.20117371360197));
#19345=CARTESIAN_POINT('Ctrl Pts',(13.8986221191241,14.4383926325365,7.19014129446066));
#19346=CARTESIAN_POINT('Ctrl Pts',(14.2277936453813,14.059884404928,7.16860220855603));
#19347=CARTESIAN_POINT('Ctrl Pts',(14.429067625472,13.9045310289345,7.15884743545613));
#19348=CARTESIAN_POINT('Ctrl Pts',(14.8728424555568,13.6848003334792,7.13943471323016));
#19349=CARTESIAN_POINT('Ctrl Pts',(15.1096558493003,13.6196045289078,7.12907542216525));
#19350=CARTESIAN_POINT('Ctrl Pts',(15.6044749214628,13.581123133793,7.10742979346171));
#19351=CARTESIAN_POINT('Ctrl Pts',(15.8580627362377,13.6119307905017,7.09633671320034));
#19352=CARTESIAN_POINT('Ctrl Pts',(16.3299097903082,13.7679999989471,7.07569598467581));
#19353=CARTESIAN_POINT('Ctrl Pts',(16.5446974999677,13.8884229991925,7.06686954824442));
#19354=CARTESIAN_POINT('Ctrl Pts',(16.9188396017716,14.2051892618886,7.04668587888927));
#19355=CARTESIAN_POINT('Ctrl Pts',(17.0741210324274,14.3991952212007,7.03593982444579));
#19356=CARTESIAN_POINT('Ctrl Pts',(17.3051308825832,14.8410333985517,7.01414857286987));
#19357=CARTESIAN_POINT('Ctrl Pts',(17.3764755515413,15.0857600434564,7.00331690944251));
#19358=CARTESIAN_POINT('Ctrl Pts',(17.418630387735,15.5774907630638,6.98376622208042));
#19359=CARTESIAN_POINT('Ctrl Pts',(17.3934433069012,15.8194293865979,6.97464600568416));
#19360=CARTESIAN_POINT('Ctrl Pts',(17.2518638159962,16.2886764165972,6.95377244513816));
#19361=CARTESIAN_POINT('Ctrl Pts',(17.1338792671752,16.5106793888636,6.94278152264873));
#19362=CARTESIAN_POINT('Ctrl Pts',(16.8157454348218,16.9009266926162,6.9210391344167));
#19363=CARTESIAN_POINT('Ctrl Pts',(16.6170831517666,17.0639271109788,6.91086627960484));
#19364=CARTESIAN_POINT('Ctrl Pts',(16.1778473847405,17.2967960249788,6.89165211656785));
#19365=CARTESIAN_POINT('Ctrl Pts',(15.9436257910071,17.3684557001225,6.88140620258127));
#19366=CARTESIAN_POINT('Ctrl Pts',(15.4515313244385,17.4210087460935,6.85987976047418));
#19367=CARTESIAN_POINT('Ctrl Pts',(15.1979214060386,17.3977303546936,6.8487857133001));
#19368=CARTESIAN_POINT('Ctrl Pts',(14.720973480494,17.2556731756669,6.82792184954051));
#19369=CARTESIAN_POINT('Ctrl Pts',(14.5015106013679,17.140818696364,6.81898801289335));
#19370=CARTESIAN_POINT('Ctrl Pts',(14.1181476122605,16.834088526908,6.79898286794978));
#19371=CARTESIAN_POINT('Ctrl Pts',(13.9578961778042,16.6450805307376,6.78831745047689));
#19372=CARTESIAN_POINT('Ctrl Pts',(13.7145778437055,16.2106454797413,6.76653744358683));
#19373=CARTESIAN_POINT('Ctrl Pts',(13.6362134003717,15.9680461672624,6.75563283338496));
#19374=CARTESIAN_POINT('Ctrl Pts',(13.5991327778437,15.644972943146,6.74258253020773));
#19375=CARTESIAN_POINT('Ctrl Pts',(13.595,15.5724496349748,6.73974467298265));
#19376=CARTESIAN_POINT('Ctrl Pts',(13.595,15.5000000000001,6.73700000000002));
#19377=CARTESIAN_POINT('Origin',(15.5,15.5,-1.713));
#19378=CARTESIAN_POINT('',(13.595,15.5,6.17449999999985));
#19379=CARTESIAN_POINT('',(13.595,15.5,6.237));
#19380=CARTESIAN_POINT('',(13.595,15.5,-1.713));
#19381=CARTESIAN_POINT('Ctrl Pts',(13.595,15.5000000000001,6.17449999999985));
#19382=CARTESIAN_POINT('Ctrl Pts',(13.595,15.5715577417839,6.1772108846115));
#19383=CARTESIAN_POINT('Ctrl Pts',(13.5990316560547,15.643188728214,6.18001272546772));
#19384=CARTESIAN_POINT('Ctrl Pts',(13.6355563128653,15.9654212002569,6.19301901746765));
#19385=CARTESIAN_POINT('Ctrl Pts',(13.7135786375042,16.2081294563647,6.20392027196532));
#19386=CARTESIAN_POINT('Ctrl Pts',(13.9562999717204,16.6429348882667,6.22570125257942));
#19387=CARTESIAN_POINT('Ctrl Pts',(14.1163117558812,16.8321904053189,6.23637080540767));
#19388=CARTESIAN_POINT('Ctrl Pts',(14.4992244320732,17.139413936818,6.2563847914538));
#19389=CARTESIAN_POINT('Ctrl Pts',(14.7184550745985,17.2545428804559,6.26531168305308));
#19390=CARTESIAN_POINT('Ctrl Pts',(15.19515525073,17.397292910129,6.2861647091306));
#19391=CARTESIAN_POINT('Ctrl Pts',(15.4487691333913,17.4209419080911,6.29725892971948));
#19392=CARTESIAN_POINT('Ctrl Pts',(15.941007088933,17.3690797945405,6.31879164868458));
#19393=CARTESIAN_POINT('Ctrl Pts',(16.1753605576116,17.2977366465769,6.32904333147894));
#19394=CARTESIAN_POINT('Ctrl Pts',(16.6148230416808,17.0655168979927,6.3482674121469));
#19395=CARTESIAN_POINT('Ctrl Pts',(16.8136158148582,16.9028988231385,6.35841784285429));
#19396=CARTESIAN_POINT('Ctrl Pts',(17.1323034625999,16.5132318636455,6.38015035859392));
#19397=CARTESIAN_POINT('Ctrl Pts',(17.2506507476386,16.2913774471692,6.3911435870773));
#19398=CARTESIAN_POINT('Ctrl Pts',(17.3929528169657,15.8223174322594,6.41202586719434));
#19399=CARTESIAN_POINT('Ctrl Pts',(17.4185084978342,15.5804256811536,6.42115770201604));
#19400=CARTESIAN_POINT('Ctrl Pts',(17.3771090366558,15.0886410810562,6.44069390881674));
#19401=CARTESIAN_POINT('Ctrl Pts',(17.3061406522188,14.8438067616542,6.45152142117628));
#19402=CARTESIAN_POINT('Ctrl Pts',(17.0757940579712,14.4015833220502,6.47331276106997));
#19403=CARTESIAN_POINT('Ctrl Pts',(16.920782151046,14.2073142095694,6.48406288968071));
#19404=CARTESIAN_POINT('Ctrl Pts',(16.5471333786859,13.890014926918,6.50425596166491));
#19405=CARTESIAN_POINT('Ctrl Pts',(16.3325910784869,13.769296908048,6.51307869297957));
#19406=CARTESIAN_POINT('Ctrl Pts',(15.8610184152089,13.6124883201033,6.53370741840729));
#19407=CARTESIAN_POINT('Ctrl Pts',(15.6074377895398,13.5812814714514,6.54480018418459));
#19408=CARTESIAN_POINT('Ctrl Pts',(15.1124854292573,13.6190147779313,6.5664516435145));
#19409=CARTESIAN_POINT('Ctrl Pts',(14.8755397433854,13.6838659268469,6.57681672163662));
#19410=CARTESIAN_POINT('Ctrl Pts',(14.4315280685365,13.9029027899722,6.59623980452585));
#19411=CARTESIAN_POINT('Ctrl Pts',(14.2301177041952,14.0578576203021,6.60597459366607));
#19412=CARTESIAN_POINT('Ctrl Pts',(13.9003731317584,14.4357464363045,6.62750274767666));
#19413=CARTESIAN_POINT('Ctrl Pts',(13.7747368954394,14.6544769786506,6.63853705758105));
#19414=CARTESIAN_POINT('Ctrl Pts',(13.6286625233942,15.0875972864192,6.65814031110006));
#19415=CARTESIAN_POINT('Ctrl Pts',(13.595,15.2932256254231,6.66666658524766));
#19416=CARTESIAN_POINT('Ctrl Pts',(13.595,15.5,6.67449999999986));
#19417=CARTESIAN_POINT('Ctrl Pts',(13.595,15.5000000000001,6.73700000000002));
#19418=CARTESIAN_POINT('Ctrl Pts',(13.595,15.3319584802696,6.73063393591528));
#19419=CARTESIAN_POINT('Ctrl Pts',(13.6172311655285,15.1643504197289,6.72379804697953));
#19420=CARTESIAN_POINT('Ctrl Pts',(13.7263421054778,14.7618781860687,6.70616433531536));
#19421=CARTESIAN_POINT('Ctrl Pts',(13.8375522583477,14.5372185214291,6.69522093841164));
#19422=CARTESIAN_POINT('Ctrl Pts',(14.1423728428836,14.1400106685456,6.67350604849701));
#19423=CARTESIAN_POINT('Ctrl Pts',(14.3342559177248,13.9723538283477,6.66299492923329));
#19424=CARTESIAN_POINT('Ctrl Pts',(14.7631181034437,13.726703827452,6.644234553655));
#19425=CARTESIAN_POINT('Ctrl Pts',(14.9940630811368,13.6475482050451,6.6341319737034));
#19426=CARTESIAN_POINT('Ctrl Pts',(15.4824475728478,13.5785748586731,6.6127678227099));
#19427=CARTESIAN_POINT('Ctrl Pts',(15.7358073629665,13.5930174114947,6.60168471728038));
#19428=CARTESIAN_POINT('Ctrl Pts',(16.2185584714547,13.718446186762,6.58056699599917));
#19429=CARTESIAN_POINT('Ctrl Pts',(16.4436261482446,13.826733204793,6.57141725624811));
#19430=CARTESIAN_POINT('Ctrl Pts',(16.8376270305051,14.1217112584022,6.55162465217484));
#19431=CARTESIAN_POINT('Ctrl Pts',(17.0034432989467,14.3047731521569,6.54106278057916));
#19432=CARTESIAN_POINT('Ctrl Pts',(17.2617626336329,14.7319068969529,6.51923126959273));
#19433=CARTESIAN_POINT('Ctrl Pts',(17.3485015451824,14.97385099212,6.50816831296608));
#19434=CARTESIAN_POINT('Ctrl Pts',(17.4199935020024,15.465166709918,6.48799167817601));
#19435=CARTESIAN_POINT('Ctrl Pts',(17.4088947887542,15.7090770775306,6.47916453779018));
#19436=CARTESIAN_POINT('Ctrl Pts',(17.2946791504231,16.1851663182313,6.45863027724424));
#19437=CARTESIAN_POINT('Ctrl Pts',(17.1905355878056,16.4123637607824,6.4477453018185));
#19438=CARTESIAN_POINT('Ctrl Pts',(16.8983953461694,16.8180237191349,6.42598756122144));
#19439=CARTESIAN_POINT('Ctrl Pts',(16.7116966296892,16.9914800033301,6.41533284088903));
#19440=CARTESIAN_POINT('Ctrl Pts',(16.2909568390832,17.2497545968349,6.39634586562964));
#19441=CARTESIAN_POINT('Ctrl Pts',(16.0631484549132,17.3357989702144,6.38663466556925));
#19442=CARTESIAN_POINT('Ctrl Pts',(15.5784723919421,17.4197976388017,6.36543273805523));
#19443=CARTESIAN_POINT('Ctrl Pts',(15.3256071822455,17.4134707300782,6.3543712678148));
#19444=CARTESIAN_POINT('Ctrl Pts',(14.8377051185746,17.3035246283544,6.33302822041015));
#19445=CARTESIAN_POINT('Ctrl Pts',(14.6073698852201,17.2013323949424,6.32359588875386));
#19446=CARTESIAN_POINT('Ctrl Pts',(14.2037461977663,16.9171476811232,6.30400170567155));
#19447=CARTESIAN_POINT('Ctrl Pts',(14.0330635436095,16.7396208715381,6.29354308563515));
#19448=CARTESIAN_POINT('Ctrl Pts',(13.7627491799401,16.3217808344018,6.27180129785241));
#19449=CARTESIAN_POINT('Ctrl Pts',(13.6688775154418,16.0834106034676,6.26071772358537));
#19450=CARTESIAN_POINT('Ctrl Pts',(13.6048088999498,15.7232646950227,6.24567267487459));
#19451=CARTESIAN_POINT('Ctrl Pts',(13.595,15.6116185684224,6.24122854399773));
#19452=CARTESIAN_POINT('Ctrl Pts',(13.595,15.5,6.23700000000001));
#19453=CARTESIAN_POINT('Origin',(15.5,15.5,-1.713));
#19454=CARTESIAN_POINT('',(13.595,15.5,5.67449999999984));
#19455=CARTESIAN_POINT('',(13.595,15.5,5.73700000000001));
#19456=CARTESIAN_POINT('',(13.595,15.5,-1.713));
#19457=CARTESIAN_POINT('Ctrl Pts',(13.595,15.5,5.67449999999984));
#19458=CARTESIAN_POINT('Ctrl Pts',(13.595,15.6185870823364,5.67899253831409));
#19459=CARTESIAN_POINT('Ctrl Pts',(13.6060718415959,15.7371765549238,5.68372733344444));
#19460=CARTESIAN_POINT('Ctrl Pts',(13.6740404949213,16.0963304252555,5.69882010257118));
#19461=CARTESIAN_POINT('Ctrl Pts',(13.7663946575648,16.3272477032882,5.70958813889097));
#19462=CARTESIAN_POINT('Ctrl Pts',(14.0371620226424,16.7461278929931,5.73137923985182));
#19463=CARTESIAN_POINT('Ctrl Pts',(14.2149617564259,16.9287854291272,5.74218789835473));
#19464=CARTESIAN_POINT('Ctrl Pts',(14.6220504754878,17.2077275576028,5.76165926007725));
#19465=CARTESIAN_POINT('Ctrl Pts',(14.84495768549,17.3050114079439,5.77084548055492));
#19466=CARTESIAN_POINT('Ctrl Pts',(15.3232149840341,17.4130834901566,5.79176662222354));
#19467=CARTESIAN_POINT('Ctrl Pts',(15.5747489125264,17.4197790697252,5.80276985619085));
#19468=CARTESIAN_POINT('Ctrl Pts',(16.070537711592,17.3351810404709,5.82445790514388));
#19469=CARTESIAN_POINT('Ctrl Pts',(16.309578092675,17.2429720428253,5.83451010407533));
#19470=CARTESIAN_POINT('Ctrl Pts',(16.7284047199156,16.9761646688132,5.85377848891489));
#19471=CARTESIAN_POINT('Ctrl Pts',(16.9064279364666,16.8076615476523,5.86405581139163));
#19472=CARTESIAN_POINT('Ctrl Pts',(17.1950904546403,16.4052040196009,5.88561616582402));
#19473=CARTESIAN_POINT('Ctrl Pts',(17.2999825807302,16.1729023374491,5.89671088240892));
#19474=CARTESIAN_POINT('Ctrl Pts',(17.4114614926336,15.6881070632203,5.91751510284064));
#19475=CARTESIAN_POINT('Ctrl Pts',(17.4197869012108,15.440967858228,5.92641294329876));
#19476=CARTESIAN_POINT('Ctrl Pts',(17.3422502165789,14.9563903088349,5.94646652204742));
#19477=CARTESIAN_POINT('Ctrl Pts',(17.2568553212246,14.7235705434374,5.95715441701744));
#19478=CARTESIAN_POINT('Ctrl Pts',(16.9988862893144,14.2974670698628,5.97893923542126));
#19479=CARTESIAN_POINT('Ctrl Pts',(16.8265177477385,14.1096348386612,5.98982513894961));
#19480=CARTESIAN_POINT('Ctrl Pts',(16.4275948667997,13.8186878681828,6.00957268523384));
#19481=CARTESIAN_POINT('Ctrl Pts',(16.2074192267811,13.7148358895865,6.01855427704374));
#19482=CARTESIAN_POINT('Ctrl Pts',(15.7329940381332,13.5930407731274,6.03930778485859));
#19483=CARTESIAN_POINT('Ctrl Pts',(15.4825177602965,13.5789405886467,6.05026475235153));
#19484=CARTESIAN_POINT('Ctrl Pts',(14.9967865899441,13.6468020229089,6.07151283504417));
#19485=CARTESIAN_POINT('Ctrl Pts',(14.7656927933891,13.725631450455,6.08162192504857));
#19486=CARTESIAN_POINT('Ctrl Pts',(14.3364443687422,13.970685449457,6.10039919646789));
#19487=CARTESIAN_POINT('Ctrl Pts',(14.1443188999266,14.1380702221899,6.11088997219073));
#19488=CARTESIAN_POINT('Ctrl Pts',(13.8389083728738,14.5348718312672,6.13260237539498));
#19489=CARTESIAN_POINT('Ctrl Pts',(13.7273677282824,14.7594070229154,6.14354828538213));
#19490=CARTESIAN_POINT('Ctrl Pts',(13.617463969655,15.1626075070602,6.16122692673826));
#19491=CARTESIAN_POINT('Ctrl Pts',(13.595,15.331080930445,6.16810069092643));
#19492=CARTESIAN_POINT('Ctrl Pts',(13.595,15.5000000000001,6.17449999999985));
#19493=CARTESIAN_POINT('Ctrl Pts',(13.595,15.5,6.23700000000001));
#19494=CARTESIAN_POINT('Ctrl Pts',(13.595,15.36977425128,6.23206654389246));
#19495=CARTESIAN_POINT('Ctrl Pts',(13.6083515816957,15.2396084108537,6.22684332799736));
#19496=CARTESIAN_POINT('Ctrl Pts',(13.6853629128828,14.8698795142821,6.21115215203331));
#19497=CARTESIAN_POINT('Ctrl Pts',(13.7821919173308,14.6402997106635,6.20033690949815));
#19498=CARTESIAN_POINT('Ctrl Pts',(14.0611179371588,14.2262903224373,6.17855188510953));
#19499=CARTESIAN_POINT('Ctrl Pts',(14.2423406160885,14.04706032314,6.16779820742024));
#19500=CARTESIAN_POINT('Ctrl Pts',(14.6546344062719,13.7759103546784,6.14850819622096));
#19501=CARTESIAN_POINT('Ctrl Pts',(14.8793586066212,13.6828711974297,6.13914966725177));
#19502=CARTESIAN_POINT('Ctrl Pts',(15.3600638250521,13.5838064298187,6.11812144247349));
#19503=CARTESIAN_POINT('Ctrl Pts',(15.6121739396263,13.5819811503158,6.10709300351574));
#19504=CARTESIAN_POINT('Ctrl Pts',(16.1050697123474,13.6761386719974,6.08553150864603));
#19505=CARTESIAN_POINT('Ctrl Pts',(16.340817115604,13.7721168422437,6.07573500226256));
#19506=CARTESIAN_POINT('Ctrl Pts',(16.7615603791949,14.0504456667631,6.05598821904094));
#19507=CARTESIAN_POINT('Ctrl Pts',(16.9423029071645,14.2301645816036,6.04522652131986));
#19508=CARTESIAN_POINT('Ctrl Pts',(17.2200799494863,14.644872787505,6.02344015375077));
#19509=CARTESIAN_POINT('Ctrl Pts',(17.3162769006898,14.8746469811613,6.01263137140422));
#19510=CARTESIAN_POINT('Ctrl Pts',(17.4149152048833,15.3544317846958,5.99229782020969));
#19511=CARTESIAN_POINT('Ctrl Pts',(17.4178535000102,15.5996361896873,5.98350653012241));
#19512=CARTESIAN_POINT('Ctrl Pts',(17.3295289414075,16.0883584972103,5.96305997662234));
#19513=CARTESIAN_POINT('Ctrl Pts',(17.2350439049634,16.3264087530365,5.95197510841829));
#19514=CARTESIAN_POINT('Ctrl Pts',(16.9637023080458,16.7434259265959,5.93024202597844));
#19515=CARTESIAN_POINT('Ctrl Pts',(16.7926052916268,16.9204658432537,5.91979278829171));
#19516=CARTESIAN_POINT('Ctrl Pts',(16.3881467431463,17.2037067413353,5.90021610030532));
#19517=CARTESIAN_POINT('Ctrl Pts',(16.1573456231628,17.3053625544976,5.89075527660389));
#19518=CARTESIAN_POINT('Ctrl Pts',(15.6690018842731,17.4139452013283,5.86939290832352));
#19519=CARTESIAN_POINT('Ctrl Pts',(15.4161920266675,17.4195630080999,5.8583338594344));
#19520=CARTESIAN_POINT('Ctrl Pts',(14.9318550990572,17.3342537273976,5.83714676723799));
#19521=CARTESIAN_POINT('Ctrl Pts',(14.7043172849098,17.2476057238062,5.82746936111434));
#19522=CARTESIAN_POINT('Ctrl Pts',(14.2842996795786,16.9882190243175,5.80845605079822));
#19523=CARTESIAN_POINT('Ctrl Pts',(14.0980650179494,16.8142588725985,5.79779239194216));
#19524=CARTESIAN_POINT('Ctrl Pts',(13.8070527298312,16.4078633395944,5.77603145582555));
#19525=CARTESIAN_POINT('Ctrl Pts',(13.7035368615051,16.1804517914393,5.76515209834613));
#19526=CARTESIAN_POINT('Ctrl Pts',(13.6121804111135,15.7952504451143,5.74856100575271));
#19527=CARTESIAN_POINT('Ctrl Pts',(13.595,15.6477240375953,5.74259635911231));
#19528=CARTESIAN_POINT('Ctrl Pts',(13.595,15.5,5.737));
#19529=CARTESIAN_POINT('Origin',(15.5,15.5,-1.713));
#19530=CARTESIAN_POINT('',(13.595,15.5,5.17449999999983));
#19531=CARTESIAN_POINT('',(13.595,15.5,5.23699999999999));
#19532=CARTESIAN_POINT('',(13.595,15.5,-1.713));
#19533=CARTESIAN_POINT('Ctrl Pts',(13.595,15.5,5.17449999999983));
#19534=CARTESIAN_POINT('Ctrl Pts',(13.595,15.6566421856364,5.18043421312606));
#19535=CARTESIAN_POINT('Ctrl Pts',(13.6143173106204,15.8129938957689,5.18677993526994));
#19536=CARTESIAN_POINT('Ctrl Pts',(13.7133238837561,16.2058714082875,5.20382915631037));
#19537=CARTESIAN_POINT('Ctrl Pts',(13.8202268828639,16.4321058332676,5.21473800402677));
#19538=CARTESIAN_POINT('Ctrl Pts',(14.1173121943619,16.8344891762869,5.23647977361834));
#19539=CARTESIAN_POINT('Ctrl Pts',(14.3060377434444,17.0057115198797,5.24709419504389));
#19540=CARTESIAN_POINT('Ctrl Pts',(14.7299474211406,17.2590800413806,5.26596464189374));
#19541=CARTESIAN_POINT('Ctrl Pts',(14.9589591096765,17.3424619118548,5.2758324194957));
#19542=CARTESIAN_POINT('Ctrl Pts',(15.4451221171311,17.4206572734562,5.29709939270021));
#19543=CARTESIAN_POINT('Ctrl Pts',(15.6982088678367,17.4111913786412,5.30817055414842));
#19544=CARTESIAN_POINT('Ctrl Pts',(16.1841394261652,17.2952308599276,5.32942735897471));
#19545=CARTESIAN_POINT('Ctrl Pts',(16.4124232908667,17.1906721299216,5.33874088501521));
#19546=CARTESIAN_POINT('Ctrl Pts',(16.8123402712279,16.9023113076282,5.35841220118947));
#19547=CARTESIAN_POINT('Ctrl Pts',(16.9811679057763,16.7226354335115,5.36891166263772));
#19548=CARTESIAN_POINT('Ctrl Pts',(17.2468951151508,16.3011735866021,5.39069032715379));
#19549=CARTESIAN_POINT('Ctrl Pts',(17.3380327017994,16.0614016975905,5.40176720118363));
#19550=CARTESIAN_POINT('Ctrl Pts',(17.4190450446205,15.5715263806302,5.42209750042186));
#19551=CARTESIAN_POINT('Ctrl Pts',(17.4125604492154,15.3268971480608,5.43089244281013));
#19552=CARTESIAN_POINT('Ctrl Pts',(17.3071804140669,14.8486945914045,5.45131350929278));
#19553=CARTESIAN_POINT('Ctrl Pts',(17.2075400051757,14.6200014430832,5.46215665367438));
#19554=CARTESIAN_POINT('Ctrl Pts',(16.9235169449159,14.2091439135888,5.48393375726179));
#19555=CARTESIAN_POINT('Ctrl Pts',(16.740171888673,14.0321078283592,5.49465074218377));
#19556=CARTESIAN_POINT('Ctrl Pts',(16.3246235208931,13.7658853657224,5.5138252653505));
#19557=CARTESIAN_POINT('Ctrl Pts',(16.0987313329976,13.675525196633,5.5233087780841));
#19558=CARTESIAN_POINT('Ctrl Pts',(15.6164951667096,13.5821988514804,5.54440397345977));
#19559=CARTESIAN_POINT('Ctrl Pts',(15.3640667095275,13.583478423546,5.55544633816588));
#19560=CARTESIAN_POINT('Ctrl Pts',(14.8730509487618,13.6836792610265,5.57692559279253));
#19561=CARTESIAN_POINT('Ctrl Pts',(14.6393794120696,13.7820369440063,5.58657395646151));
#19562=CARTESIAN_POINT('Ctrl Pts',(14.2298320094521,14.0594989012133,5.60604302053995));
#19563=CARTESIAN_POINT('Ctrl Pts',(14.0562371293134,14.233548774446,5.61643361773215));
#19564=CARTESIAN_POINT('Ctrl Pts',(13.7786824085209,14.6454944475955,5.63811046717757));
#19565=CARTESIAN_POINT('Ctrl Pts',(13.6804785478273,14.8815606152973,5.64920150954635));
#19566=CARTESIAN_POINT('Ctrl Pts',(13.6070998178414,15.2520820958729,5.66484325844481));
#19567=CARTESIAN_POINT('Ctrl Pts',(13.595,15.3760295924857,5.66980352046244));
#19568=CARTESIAN_POINT('Ctrl Pts',(13.595,15.5,5.67449999999984));
#19569=CARTESIAN_POINT('Ctrl Pts',(13.595,15.5,5.73700000000001));
#19570=CARTESIAN_POINT('Ctrl Pts',(13.595,15.4066866192903,5.73346492746249));
#19571=CARTESIAN_POINT('Ctrl Pts',(13.6018555842158,15.3133058701765,5.72977735558749));
#19572=CARTESIAN_POINT('Ctrl Pts',(13.6529137828576,14.9689371987211,5.71561457706302));
#19573=CARTESIAN_POINT('Ctrl Pts',(13.7402672426745,14.7272905418752,5.70454944698966));
#19574=CARTESIAN_POINT('Ctrl Pts',(13.9996235813187,14.3009379189473,5.68272484630075));
#19575=CARTESIAN_POINT('Ctrl Pts',(14.1658625390628,14.1183438769257,5.67217145356922));
#19576=CARTESIAN_POINT('Ctrl Pts',(14.5606866342577,13.8242830841638,5.65239559335981));
#19577=CARTESIAN_POINT('Ctrl Pts',(14.7861975769119,13.7165114108178,5.64322495289096));
#19578=CARTESIAN_POINT('Ctrl Pts',(15.2693933527132,13.5923905631024,5.62208777984625));
#19579=CARTESIAN_POINT('Ctrl Pts',(15.5227209974273,13.5786379454799,5.61100608060241));
#19580=CARTESIAN_POINT('Ctrl Pts',(16.0107923698647,13.6488891805299,5.58965562686497));
#19581=CARTESIAN_POINT('Ctrl Pts',(16.2414707537612,13.7286260121631,5.57956470893425));
#19582=CARTESIAN_POINT('Ctrl Pts',(16.6696419804527,13.9753377070707,5.56083455903523));
#19583=CARTESIAN_POINT('Ctrl Pts',(16.86109178745,14.1434790644713,5.55028677590578));
#19584=CARTESIAN_POINT('Ctrl Pts',(17.1648587298731,14.5414095863163,5.52856755403043));
#19585=CARTESIAN_POINT('Ctrl Pts',(17.2754789966671,14.7662901237697,5.5176286917536));
#19586=CARTESIAN_POINT('Ctrl Pts',(17.4024536246495,15.2392462161482,5.49693405899484));
#19587=CARTESIAN_POINT('Ctrl Pts',(17.4201554501318,15.4821893016267,5.48800622232349));
#19588=CARTESIAN_POINT('Ctrl Pts',(17.3626040078135,15.9727313988826,5.46816380591895));
#19589=CARTESIAN_POINT('Ctrl Pts',(17.2836290157076,16.2151349357133,5.45725325837236));
#19590=CARTESIAN_POINT('Ctrl Pts',(17.0392460050135,16.6489065389848,5.43547509856397));
#19591=CARTESIAN_POINT('Ctrl Pts',(16.8785675462961,16.8374717941287,5.42481711384901));
#19592=CARTESIAN_POINT('Ctrl Pts',(16.4944006491489,17.1433203750861,5.40482778360432));
#19593=CARTESIAN_POINT('Ctrl Pts',(16.2745221682787,17.2576841962038,5.39588110972356));
#19594=CARTESIAN_POINT('Ctrl Pts',(15.797132339406,17.3985022762211,5.37499791510973));
#19595=CARTESIAN_POINT('Ctrl Pts',(15.5435308112421,17.4211183361773,5.36390423496259));
#19596=CARTESIAN_POINT('Ctrl Pts',(15.0516952055145,17.3673309276156,5.34238911660183));
#19597=CARTESIAN_POINT('Ctrl Pts',(14.8177104042985,17.2951059930202,5.33215356099309));
#19598=CARTESIAN_POINT('Ctrl Pts',(14.3788806946875,17.0610762316894,5.31295716074765));
#19599=CARTESIAN_POINT('Ctrl Pts',(14.1804521716289,16.8973909286625,5.30274375017752));
#19600=CARTESIAN_POINT('Ctrl Pts',(13.8633108982278,16.506105803706,5.28098375476911));
#19601=CARTESIAN_POINT('Ctrl Pts',(13.7459758639615,16.2838384426846,5.26999702256394));
#19602=CARTESIAN_POINT('Ctrl Pts',(13.6217634454933,15.8680622081078,5.25152900022502));
#19603=CARTESIAN_POINT('Ctrl Pts',(13.595,15.6843757766305,5.24398486904657));
#19604=CARTESIAN_POINT('Ctrl Pts',(13.595,15.4999999999999,5.23699999999999));
#19605=CARTESIAN_POINT('Origin',(15.5,15.5,-1.713));
#19606=CARTESIAN_POINT('',(13.595,15.4999999999999,4.67449999999982));
#19607=CARTESIAN_POINT('',(13.595,15.5,4.73699999999999));
#19608=CARTESIAN_POINT('',(13.595,15.5,-1.713));
#19609=CARTESIAN_POINT('Ctrl Pts',(13.595,15.4999999999999,4.67449999999982));
#19610=CARTESIAN_POINT('Ctrl Pts',(13.595,15.693650091279,4.68183621603188));
#19611=CARTESIAN_POINT('Ctrl Pts',(13.6245240457925,15.8864371338263,4.6897854942148));
#19612=CARTESIAN_POINT('Ctrl Pts',(13.7576295137902,16.309524273011,4.70872499310137));
#19613=CARTESIAN_POINT('Ctrl Pts',(13.8784159600935,16.5303628765405,4.71973308863698));
#19614=CARTESIAN_POINT('Ctrl Pts',(14.2008185419825,16.9161133260124,4.74139848582457));
#19615=CARTESIAN_POINT('Ctrl Pts',(14.4004879063477,17.076162988088,4.75140235810768));
#19616=CARTESIAN_POINT('Ctrl Pts',(14.8414739820042,17.3040010959973,4.77069308757649));
#19617=CARTESIAN_POINT('Ctrl Pts',(15.0767072907508,17.3731999162084,4.7809832585628));
#19618=CARTESIAN_POINT('Ctrl Pts',(15.5698897955118,17.420386369048,4.80255729639139));
#19619=CARTESIAN_POINT('Ctrl Pts',(15.8235167409559,17.3942318988719,4.81365208840559));
#19620=CARTESIAN_POINT('Ctrl Pts',(16.298532950826,17.246806760591,4.83443145016721));
#19621=CARTESIAN_POINT('Ctrl Pts',(16.5161993929083,17.1298236291038,4.84331588057563));
#19622=CARTESIAN_POINT('Ctrl Pts',(16.8960583609061,16.8192632403375,4.86338948819069));
#19623=CARTESIAN_POINT('Ctrl Pts',(17.0544365648767,16.6283384286404,4.87408655026979));
#19624=CARTESIAN_POINT('Ctrl Pts',(17.2930980298608,16.1910451586717,4.89587298129296));
#19625=CARTESIAN_POINT('Ctrl Pts',(17.3687982653089,15.9476117971498,4.90675091624183));
#19626=CARTESIAN_POINT('Ctrl Pts',(17.4197225373191,15.4565367215639,4.92646857269976));
#19627=CARTESIAN_POINT('Ctrl Pts',(17.39880485994,15.2140373938938,4.93546887364174));
#19628=CARTESIAN_POINT('Ctrl Pts',(17.2655724451835,14.7426541640862,4.95624079224673));
#19629=CARTESIAN_POINT('Ctrl Pts',(17.15178954068,14.5189773017227,4.96720322869893));
#19630=CARTESIAN_POINT('Ctrl Pts',(16.8423837032947,14.1249579111728,4.98889761717191));
#19631=CARTESIAN_POINT('Ctrl Pts',(16.6486204803811,13.9594307097668,4.99925413471649));
#19632=CARTESIAN_POINT('Ctrl Pts',(16.2167685356687,13.7184426840639,5.0181452959025));
#19633=CARTESIAN_POINT('Ctrl Pts',(15.9846754599108,13.6418370567856,5.02829809886653));
#19634=CARTESIAN_POINT('Ctrl Pts',(15.4949609663296,13.5784622021334,5.04972043016928));
#19635=CARTESIAN_POINT('Ctrl Pts',(15.2414820619885,13.5959234565942,5.06080874619469));
#19636=CARTESIAN_POINT('Ctrl Pts',(14.7606910573368,13.7270579892792,5.08184072365098));
#19637=CARTESIAN_POINT('Ctrl Pts',(14.5375531120099,13.8375948904197,5.09090587872771));
#19638=CARTESIAN_POINT('Ctrl Pts',(14.1471662310465,14.1365864779329,5.11077148462383));
#19639=CARTESIAN_POINT('Ctrl Pts',(13.983219344328,14.3216893814352,5.1213697899653));
#19640=CARTESIAN_POINT('Ctrl Pts',(13.7294756616269,14.7522208894023,5.14322994151294));
#19641=CARTESIAN_POINT('Ctrl Pts',(13.645443790657,14.9954521834583,5.15428245311104));
#19642=CARTESIAN_POINT('Ctrl Pts',(13.6005693043702,15.3317165368294,5.16800295685337));
#19643=CARTESIAN_POINT('Ctrl Pts',(13.595,15.4158954773162,5.17131379469724));
#19644=CARTESIAN_POINT('Ctrl Pts',(13.595,15.4999999999999,5.17449999999983));
#19645=CARTESIAN_POINT('Ctrl Pts',(13.595,15.4999999999999,5.23699999999999));
#19646=CARTESIAN_POINT('Ctrl Pts',(13.595,15.4440288618566,5.23487959634685));
#19647=CARTESIAN_POINT('Ctrl Pts',(13.5974666521958,15.3879982888102,5.23270298979645));
#19648=CARTESIAN_POINT('Ctrl Pts',(13.6246703649183,15.0806012568895,5.22046259193762));
#19649=CARTESIAN_POINT('Ctrl Pts',(13.696688705695,14.8360689879445,5.2096235574958));
#19650=CARTESIAN_POINT('Ctrl Pts',(13.9288851203419,14.3949234747567,5.18783259386893));
#19651=CARTESIAN_POINT('Ctrl Pts',(14.0846482983729,14.2013898445396,5.17709389617555));
#19652=CARTESIAN_POINT('Ctrl Pts',(14.4596738194808,13.8855790715094,5.15692710209035));
#19653=CARTESIAN_POINT('Ctrl Pts',(14.6749021791709,13.7656850727794,5.14809351797152));
#19654=CARTESIAN_POINT('Ctrl Pts',(15.1472402509199,13.6109424793995,5.12743131010844));
#19655=CARTESIAN_POINT('Ctrl Pts',(15.4008394411745,13.58085061349,5.11633773223203));
#19656=CARTESIAN_POINT('Ctrl Pts',(15.8954167028646,13.6206728956279,5.09470268141442));
#19657=CARTESIAN_POINT('Ctrl Pts',(16.1319915940397,13.6864862114627,5.08435382353274));
#19658=CARTESIAN_POINT('Ctrl Pts',(16.5753408034579,13.9074616597123,5.06495971988364));
#19659=CARTESIAN_POINT('Ctrl Pts',(16.7763697576834,14.0635313609246,5.05516856755623));
#19660=CARTESIAN_POINT('Ctrl Pts',(17.1045107759233,14.443150998749,5.03360991667034));
#19661=CARTESIAN_POINT('Ctrl Pts',(17.2290846024511,14.6623534917871,5.02258096475398));
#19662=CARTESIAN_POINT('Ctrl Pts',(17.3838445618186,15.1281353737474,5.00155039073458));
#19663=CARTESIAN_POINT('Ctrl Pts',(17.4157337528869,15.3692601144926,4.99218770509971));
#19664=CARTESIAN_POINT('Ctrl Pts',(17.3872640267862,15.8619047995735,4.97290171755076));
#19665=CARTESIAN_POINT('Ctrl Pts',(17.3227610517695,16.1084897777251,4.9621492966068));
#19666=CARTESIAN_POINT('Ctrl Pts',(17.1038653885543,16.5571518054196,4.94036449584985));
#19667=CARTESIAN_POINT('Ctrl Pts',(16.9535335352168,16.7558681228355,4.92954825325593));
#19668=CARTESIAN_POINT('Ctrl Pts',(16.5883501587876,17.0822549849342,4.90919606593078));
#19669=CARTESIAN_POINT('Ctrl Pts',(16.3779502270845,17.2079927184403,4.90040552174481));
#19670=CARTESIAN_POINT('Ctrl Pts',(15.9111037107944,17.3773323556364,4.87998353940493));
#19671=CARTESIAN_POINT('Ctrl Pts',(15.6577379712513,17.415329839683,4.86890017372065));
#19672=CARTESIAN_POINT('Ctrl Pts',(15.1606900201998,17.3903533744672,4.84715704375341));
#19673=CARTESIAN_POINT('Ctrl Pts',(14.921572710822,17.3313950924429,4.83669696897749));
#19674=CARTESIAN_POINT('Ctrl Pts',(14.4735875094848,17.1241250736244,4.81710006603188));
#19675=CARTESIAN_POINT('Ctrl Pts',(14.2698827973726,16.9758494372357,4.80767211301389));
#19676=CARTESIAN_POINT('Ctrl Pts',(13.9305664816617,16.6084525263448,4.78633207732014));
#19677=CARTESIAN_POINT('Ctrl Pts',(13.7985548407317,16.3926761471158,4.77527023801942));
#19678=CARTESIAN_POINT('Ctrl Pts',(13.6345793555488,15.9468176951894,4.75479287631985));
#19679=CARTESIAN_POINT('Ctrl Pts',(13.595,15.7242052404364,4.74549376351178));
#19680=CARTESIAN_POINT('Ctrl Pts',(13.595,15.5,4.73699999999999));
#19681=CARTESIAN_POINT('Origin',(15.5,15.5,-1.713));
#19682=CARTESIAN_POINT('',(13.595,15.5,4.17449999999982));
#19683=CARTESIAN_POINT('',(13.595,15.5,4.23699999999999));
#19684=CARTESIAN_POINT('',(13.595,15.5,-1.713));
#19685=CARTESIAN_POINT('Ctrl Pts',(13.595,15.5,4.17449999999982));
#19686=CARTESIAN_POINT('Ctrl Pts',(13.595,15.734025771486,4.18336580329146));
#19687=CARTESIAN_POINT('Ctrl Pts',(13.6381242017143,15.9661696128238,4.19310353578431));
#19688=CARTESIAN_POINT('Ctrl Pts',(13.812515122304,16.4188995454661,4.21406902498013));
#19689=CARTESIAN_POINT('Ctrl Pts',(13.9480839527807,16.6329350332865,4.22514271636255));
#19690=CARTESIAN_POINT('Ctrl Pts',(14.2927068659157,16.9943964157289,4.24637395854319));
#19691=CARTESIAN_POINT('Ctrl Pts',(14.4976998188631,17.1389510152929,4.25565484771903));
#19692=CARTESIAN_POINT('Ctrl Pts',(14.9479020883219,17.3395491284113,4.27534873527192));
#19693=CARTESIAN_POINT('Ctrl Pts',(15.1881891966758,17.3951277348535,4.28585998235654));
#19694=CARTESIAN_POINT('Ctrl Pts',(15.6862853454185,17.4128162501582,4.3076489652412));
#19695=CARTESIAN_POINT('Ctrl Pts',(15.9394507336502,17.3709532407305,4.31872356665118));
#19696=CARTESIAN_POINT('Ctrl Pts',(16.4035567965287,17.1945153901765,4.33902566913932));
#19697=CARTESIAN_POINT('Ctrl Pts',(16.6116260315229,17.0659142210648,4.34782421348068));
#19698=CARTESIAN_POINT('Ctrl Pts',(16.9719236784538,16.7343346544246,4.36826625860546));
#19699=CARTESIAN_POINT('Ctrl Pts',(17.1195095894967,16.5331122239924,4.3791173824938));
#19700=CARTESIAN_POINT('Ctrl Pts',(17.3317425178926,16.0808845130844,4.40089153604325));
#19701=CARTESIAN_POINT('Ctrl Pts',(17.3925100159836,15.8333727489235,4.41159736388861));
#19702=CARTESIAN_POINT('Ctrl Pts',(17.4135469652281,15.3402855648001,4.43073754334417));
#19703=CARTESIAN_POINT('Ctrl Pts',(17.3779934553216,15.0995715038687,4.44026047779474));
#19704=CARTESIAN_POINT('Ctrl Pts',(17.2159943844446,14.635742480553,4.46137540573186));
#19705=CARTESIAN_POINT('Ctrl Pts',(17.0878282845223,14.41815902733,4.47242159330383));
#19706=CARTESIAN_POINT('Ctrl Pts',(16.7542753674769,14.0444116901943,4.49387614916905));
#19707=CARTESIAN_POINT('Ctrl Pts',(16.5519560555435,13.8921093194543,4.50348267473561));
#19708=CARTESIAN_POINT('Ctrl Pts',(16.1063673649305,13.6777137212781,4.52297474344133));
#19709=CARTESIAN_POINT('Ctrl Pts',(15.8685487957529,13.6151762789497,4.5333780054351));
#19710=CARTESIAN_POINT('Ctrl Pts',(15.3727325401662,13.5824592590899,4.55506725546075));
#19711=CARTESIAN_POINT('Ctrl Pts',(15.1192156632405,13.6163400777149,4.56615723257909));
#19712=CARTESIAN_POINT('Ctrl Pts',(14.6494911983603,13.778093083205,4.58670510943296));
#19713=CARTESIAN_POINT('Ctrl Pts',(14.4365866050679,13.9007875242667,4.59550822692166));
#19714=CARTESIAN_POINT('Ctrl Pts',(14.0662546981211,14.2216601832908,4.61576412489049));
#19715=CARTESIAN_POINT('Ctrl Pts',(13.9130640951453,14.4176871387399,4.62654101136175));
#19716=CARTESIAN_POINT('Ctrl Pts',(13.6871884480189,14.8624720373025,4.64833159950425));
#19717=CARTESIAN_POINT('Ctrl Pts',(13.6187513842615,15.1080140819445,4.65913055751981));
#19718=CARTESIAN_POINT('Ctrl Pts',(13.5967192885175,15.4064955285285,4.67092008346784));
#19719=CARTESIAN_POINT('Ctrl Pts',(13.595,15.4532714716672,4.67272974223003));
#19720=CARTESIAN_POINT('Ctrl Pts',(13.595,15.4999999999999,4.67449999999982));
#19721=CARTESIAN_POINT('Ctrl Pts',(13.595,15.5,4.73699999999999));
#19722=CARTESIAN_POINT('Ctrl Pts',(13.595,15.4831619553197,4.7363621096044));
#19723=CARTESIAN_POINT('Ctrl Pts',(13.5952232431582,15.4663152912995,4.7357190098412));
#19724=CARTESIAN_POINT('Ctrl Pts',(13.6023655458863,15.1971724622401,4.72536661795248));
#19725=CARTESIAN_POINT('Ctrl Pts',(13.6591298149792,14.9487353487148,4.71471329397599));
#19726=CARTESIAN_POINT('Ctrl Pts',(13.8641846941326,14.492810121388,4.69295606437544));
#19727=CARTESIAN_POINT('Ctrl Pts',(14.0087939561605,14.2889526851148,4.68207022231169));
#19728=CARTESIAN_POINT('Ctrl Pts',(14.3638555614543,13.9518516272429,4.66153352579343));
#19729=CARTESIAN_POINT('Ctrl Pts',(14.5694758198165,13.8202059240749,4.65270534471494));
#19730=CARTESIAN_POINT('Ctrl Pts',(15.0306371499171,13.6362685867437,4.63253205818381));
#19731=CARTESIAN_POINT('Ctrl Pts',(15.2835284644135,13.5903088851982,4.62146944600111));
#19732=CARTESIAN_POINT('Ctrl Pts',(15.7826210477588,13.6002529304787,4.59963687455116));
#19733=CARTESIAN_POINT('Ctrl Pts',(16.0240954015147,13.6522298508273,4.58907369197216));
#19734=CARTESIAN_POINT('Ctrl Pts',(16.4766136948028,13.8457736790557,4.56927849104091));
#19735=CARTESIAN_POINT('Ctrl Pts',(16.6829617157418,13.9864450034406,4.56013194309592));
#19736=CARTESIAN_POINT('Ctrl Pts',(17.0331029063219,14.3416440342871,4.5390172458342));
#19737=CARTESIAN_POINT('Ctrl Pts',(17.1723855710743,14.5537894077969,4.52793392933678));
#19738=CARTESIAN_POINT('Ctrl Pts',(17.3570411132624,15.0111720821459,4.50656766571775));
#19739=CARTESIAN_POINT('Ctrl Pts',(17.4040616127429,15.250744692468,4.4964632818013));
#19740=CARTESIAN_POINT('Ctrl Pts',(17.4059498803602,15.7449854401353,4.47769822594508));
#19741=CARTESIAN_POINT('Ctrl Pts',(17.3567950913128,15.9950099762399,4.46719275289177));
#19742=CARTESIAN_POINT('Ctrl Pts',(17.1653922803363,16.4576815526093,4.44547854710732));
#19743=CARTESIAN_POINT('Ctrl Pts',(17.0265119247938,16.6663842353441,4.43453445249414));
#19744=CARTESIAN_POINT('Ctrl Pts',(16.6813718542421,17.0138234716047,4.41382311215519));
#19745=CARTESIAN_POINT('Ctrl Pts',(16.4802586289945,17.1511769420762,4.40488095489924));
#19746=CARTESIAN_POINT('Ctrl Pts',(16.0272739253252,17.3479041534575,4.38506535106421));
#19747=CARTESIAN_POINT('Ctrl Pts',(15.7780157251603,17.4014353388329,4.37416166776742));
#19748=CARTESIAN_POINT('Ctrl Pts',(15.2801185049117,17.4081274237639,4.35238138691667));
#19749=CARTESIAN_POINT('Ctrl Pts',(15.0362808427617,17.3639413217721,4.34171482251817));
#19750=CARTESIAN_POINT('Ctrl Pts',(14.5789072455624,17.1854806004968,4.32170722858996));
#19751=CARTESIAN_POINT('Ctrl Pts',(14.3696752470818,17.0529411363222,4.31277533237892));
#19752=CARTESIAN_POINT('Ctrl Pts',(14.0080442480033,16.7110760491522,4.29191446843773));
#19753=CARTESIAN_POINT('Ctrl Pts',(13.8609901516845,16.5031329336648,4.28082037094368));
#19754=CARTESIAN_POINT('Ctrl Pts',(13.6602695809877,16.0507512667193,4.25929218629232));
#19755=CARTESIAN_POINT('Ctrl Pts',(13.6051237015921,15.8120917324614,4.24904467276561));
#19756=CARTESIAN_POINT('Ctrl Pts',(13.5954220493531,15.5463200269535,4.23876401333006));
#19757=CARTESIAN_POINT('Ctrl Pts',(13.595,15.5231518125555,4.23787708039442));
#19758=CARTESIAN_POINT('Ctrl Pts',(13.595,15.5,4.23699999999999));
#19759=CARTESIAN_POINT('Origin',(15.5,15.5,-1.713));
#19760=CARTESIAN_POINT('',(13.595,15.5,3.67449999999982));
#19761=CARTESIAN_POINT('',(13.595,15.5000000000001,3.73699999999998));
#19762=CARTESIAN_POINT('',(13.595,15.5,-1.713));
#19763=CARTESIAN_POINT('Ctrl Pts',(13.595,15.5000000000001,3.67449999999982));
#19764=CARTESIAN_POINT('Ctrl Pts',(13.595,15.5315708493142,3.67569602613827));
#19765=CARTESIAN_POINT('Ctrl Pts',(13.5957848075677,15.5631695708928,3.67691027370593));
#19766=CARTESIAN_POINT('Ctrl Pts',(13.6094509573792,15.8375445965614,3.68760357280036));
#19767=CARTESIAN_POINT('Ctrl Pts',(13.6678982376643,16.0757547526509,3.69790627125859));
#19768=CARTESIAN_POINT('Ctrl Pts',(13.8751161890635,16.5259447952251,3.71949354112295));
#19769=CARTESIAN_POINT('Ctrl Pts',(14.0252969144295,16.7320999971229,3.73058829198247));
#19770=CARTESIAN_POINT('Ctrl Pts',(14.3915344309247,17.0685073425307,3.75134315048599));
#19771=CARTESIAN_POINT('Ctrl Pts',(14.601951052826,17.1977682735184,3.76021526915221));
#19772=CARTESIAN_POINT('Ctrl Pts',(15.0612830005563,17.3700262996204,3.7803085302078));
#19773=CARTESIAN_POINT('Ctrl Pts',(15.3060217793934,17.4109761507869,3.79101451353403));
#19774=CARTESIAN_POINT('Ctrl Pts',(15.804090800173,17.3974380449954,3.81280230971864));
#19775=CARTESIAN_POINT('Ctrl Pts',(16.0525785874332,17.340494181246,3.82367229166355));
#19776=CARTESIAN_POINT('Ctrl Pts',(16.5026503825806,17.1376503654255,3.84336047167876));
#19777=CARTESIAN_POINT('Ctrl Pts',(16.7017358152984,16.9976812351531,3.85238004861031));
#19778=CARTESIAN_POINT('Ctrl Pts',(17.0422872779096,16.6455161561091,3.8731700589377));
#19779=CARTESIAN_POINT('Ctrl Pts',(17.1784821282183,16.4346393801006,3.88413777854603));
#19780=CARTESIAN_POINT('Ctrl Pts',(17.3635397218247,15.9689971022106,3.90582574173643));
#19781=CARTESIAN_POINT('Ctrl Pts',(17.4092004324088,15.7182717232893,3.91613914814077));
#19782=CARTESIAN_POINT('Ctrl Pts',(17.4003710694834,15.2237194221972,3.93506782433103));
#19783=CARTESIAN_POINT('Ctrl Pts',(17.3498602599869,14.9845054896736,3.94523496113124));
#19784=CARTESIAN_POINT('Ctrl Pts',(17.1582910552894,14.5292027117347,3.96667364767794));
#19785=CARTESIAN_POINT('Ctrl Pts',(17.015656870939,14.3188280123367,3.97776318950503));
#19786=CARTESIAN_POINT('Ctrl Pts',(16.660552230454,13.9693401892086,3.99877008597855));
#19787=CARTESIAN_POINT('Ctrl Pts',(16.4529697003171,13.8321739172205,4.00781278651278));
#19788=CARTESIAN_POINT('Ctrl Pts',(15.9983593128666,13.6450791244421,4.0276995051239));
#19789=CARTESIAN_POINT('Ctrl Pts',(15.7558449606823,13.5964189325426,4.03830818194736));
#19790=CARTESIAN_POINT('Ctrl Pts',(15.2559430449784,13.5935867057772,4.06017615726248));
#19791=CARTESIAN_POINT('Ctrl Pts',(15.0033585050623,13.6432985756689,4.07122534973473));
#19792=CARTESIAN_POINT('Ctrl Pts',(14.5449308807844,13.8340871424297,4.09127905158412));
#19793=CARTESIAN_POINT('Ctrl Pts',(14.3415359755962,13.9685334120202,4.10015367637626));
#19794=CARTESIAN_POINT('Ctrl Pts',(13.9913260773587,14.3107103153903,4.12077654776842));
#19795=CARTESIAN_POINT('Ctrl Pts',(13.8495044196596,14.5169615480573,4.13169210489444));
#19796=CARTESIAN_POINT('Ctrl Pts',(13.6511313198597,14.9761977731424,4.15342862226806));
#19797=CARTESIAN_POINT('Ctrl Pts',(13.5980741954768,15.2254298346918,4.16403097830177));
#19798=CARTESIAN_POINT('Ctrl Pts',(13.5950432048621,15.4851832998888,4.17393774098282));
#19799=CARTESIAN_POINT('Ctrl Pts',(13.595,15.4925925572656,4.1742193773583));
#19800=CARTESIAN_POINT('Ctrl Pts',(13.595,15.5,4.17449999999982));
#19801=CARTESIAN_POINT('Ctrl Pts',(13.595,15.5,4.23699999999999));
#19802=CARTESIAN_POINT('Ctrl Pts',(13.595,15.2691971061883,4.22825629180628));
#19803=CARTESIAN_POINT('Ctrl Pts',(13.6369428485792,15.0400926775705,4.21865954291788));
#19804=CARTESIAN_POINT('Ctrl Pts',(13.8073918288257,14.5910901252192,4.19792148050212));
#19805=CARTESIAN_POINT('Ctrl Pts',(13.9405739255903,14.377844531064,4.18692991662784));
#19806=CARTESIAN_POINT('Ctrl Pts',(14.2760191032244,14.0204621113541,4.16605393923708));
#19807=CARTESIAN_POINT('Ctrl Pts',(14.4728882249431,13.8775982084076,4.15693052384329));
#19808=CARTESIAN_POINT('Ctrl Pts',(14.9197252436716,13.6680512453625,4.1373838476084));
#19809=CARTESIAN_POINT('Ctrl Pts',(15.1673108338374,13.6073689833216,4.1265533318531));
#19810=CARTESIAN_POINT('Ctrl Pts',(15.6654595231384,13.5862977508088,4.10476205060632));
#19811=CARTESIAN_POINT('Ctrl Pts',(15.911140189458,13.6236713128153,4.09401486485305));
#19812=CARTESIAN_POINT('Ctrl Pts',(16.372598461827,13.7891125043602,4.07382858872142));
#19813=CARTESIAN_POINT('Ctrl Pts',(16.584318487475,13.9148128026822,4.06500319942661));
#19814=CARTESIAN_POINT('Ctrl Pts',(16.9555414155677,14.2452414189295,4.04436579610842));
#19815=CARTESIAN_POINT('Ctrl Pts',(17.1091103920882,14.449394084336,4.03327280036245));
#19816=CARTESIAN_POINT('Ctrl Pts',(17.3233921437259,14.8970890954297,4.01162555064358));
#19817=CARTESIAN_POINT('Ctrl Pts',(17.3854386913095,15.1347574577275,4.00126465330248));
#19818=CARTESIAN_POINT('Ctrl Pts',(17.4172331534591,15.628903797461,3.98184905774384));
#19819=CARTESIAN_POINT('Ctrl Pts',(17.3834448089266,15.8808663522567,3.9720998454925));
#19820=CARTESIAN_POINT('Ctrl Pts',(17.2204610163731,16.3552431693938,3.95056378814853));
#19821=CARTESIAN_POINT('Ctrl Pts',(17.0936095846538,16.5732361235507,3.93953084186659));
#19822=CARTESIAN_POINT('Ctrl Pts',(16.7687702371492,16.9413129963823,3.91848169067809));
#19823=CARTESIAN_POINT('Ctrl Pts',(16.5763758116767,17.0901414674553,3.90908555606629));
#19824=CARTESIAN_POINT('Ctrl Pts',(16.1362270921317,17.3132715624607,3.88983145634868));
#19825=CARTESIAN_POINT('Ctrl Pts',(15.890655702729,17.381516306028,3.87908905086301));
#19826=CARTESIAN_POINT('Ctrl Pts',(15.3926987432721,17.4179362844291,3.85730615674856));
#19827=CARTESIAN_POINT('Ctrl Pts',(15.1452598980358,17.387899019869,3.84648206028155));
#19828=CARTESIAN_POINT('Ctrl Pts',(14.6795555871987,17.2363330912826,3.82611004318458));
#19829=CARTESIAN_POINT('Ctrl Pts',(14.4651755424473,17.1177510719111,3.81731939179786));
#19830=CARTESIAN_POINT('Ctrl Pts',(14.084044801387,16.7994221119836,3.79692366403812));
#19831=CARTESIAN_POINT('Ctrl Pts',(13.9237377365017,16.5994592092857,3.78584201548196));
#19832=CARTESIAN_POINT('Ctrl Pts',(13.6953359488009,16.1571086298419,3.76408839636438));
#19833=CARTESIAN_POINT('Ctrl Pts',(13.6260627817449,15.9206924627447,3.75361687448774));
#19834=CARTESIAN_POINT('Ctrl Pts',(13.597760005866,15.618479508341,3.74154883057672));
#19835=CARTESIAN_POINT('Ctrl Pts',(13.595,15.5592060680503,3.73924295533636));
#19836=CARTESIAN_POINT('Ctrl Pts',(13.595,15.5000000000001,3.73699999999998));
#19837=CARTESIAN_POINT('Origin',(15.5,15.5,-1.713));
#19838=CARTESIAN_POINT('',(13.595,15.5000000000001,3.17449999999981));
#19839=CARTESIAN_POINT('',(13.595,15.5,3.23699999999997));
#19840=CARTESIAN_POINT('',(13.595,15.5,-1.713));
#19841=CARTESIAN_POINT('Ctrl Pts',(13.595,15.5000000000001,3.17449999999981));
#19842=CARTESIAN_POINT('Ctrl Pts',(13.595,15.568249989465,3.177085574133));
#19843=CARTESIAN_POINT('Ctrl Pts',(13.5986675612602,15.6365760475214,3.17975424791452));
#19844=CARTESIAN_POINT('Ctrl Pts',(13.6322958131998,15.947741225573,3.19227791698431));
#19845=CARTESIAN_POINT('Ctrl Pts',(13.705104464663,16.1834642537271,3.20280050912647));
#19846=CARTESIAN_POINT('Ctrl Pts',(13.9403835379756,16.6230360937529,3.2245992806447));
#19847=CARTESIAN_POINT('Ctrl Pts',(14.1039553317352,16.8208663486228,3.23567154325336));
#19848=CARTESIAN_POINT('Ctrl Pts',(14.4898892604546,17.1332251253252,3.25594615393048));
#19849=CARTESIAN_POINT('Ctrl Pts',(14.7055970842692,17.2483348778709,3.26474921628444));
#19850=CARTESIAN_POINT('Ctrl Pts',(15.1733677361523,17.3930116831415,3.28521162450332));
#19851=CARTESIAN_POINT('Ctrl Pts',(15.4215992597164,17.4193817462098,3.29607039631279));
#19852=CARTESIAN_POINT('Ctrl Pts',(15.9192846661276,17.3753414100464,3.31784141146642));
#19853=CARTESIAN_POINT('Ctrl Pts',(16.1637685524579,17.3033692592156,3.32853624463924));
#19854=CARTESIAN_POINT('Ctrl Pts',(16.6005469044634,17.0735253401857,3.34764290920643));
#19855=CARTESIAN_POINT('Ctrl Pts',(16.7907360361107,16.9216959633891,3.35720530171909));
#19856=CARTESIAN_POINT('Ctrl Pts',(17.1102003271643,16.5482733681289,3.37833940492863));
#19857=CARTESIAN_POINT('Ctrl Pts',(17.2338102066998,16.3279646081025,3.38938918282134));
#19858=CARTESIAN_POINT('Ctrl Pts',(17.3889206611445,15.8518324907181,3.410819529997));
#19859=CARTESIAN_POINT('Ctrl Pts',(17.4187651327053,15.6006421711202,3.42038620983217));
#19860=CARTESIAN_POINT('Ctrl Pts',(17.3800740437233,15.1078674697106,3.43990068727113));
#19861=CARTESIAN_POINT('Ctrl Pts',(17.3145265316614,14.8707782405648,3.45031621882997));
#19862=CARTESIAN_POINT('Ctrl Pts',(17.093393792891,14.4256163350543,3.47201735130392));
#19863=CARTESIAN_POINT('Ctrl Pts',(16.9365496772127,14.2234651246719,3.48310615889079));
#19864=CARTESIAN_POINT('Ctrl Pts',(16.5605112283184,13.8988819668973,3.50362743993718));
#19865=CARTESIAN_POINT('Ctrl Pts',(16.3475097391379,13.7766339740126,3.51242608315226));
#19866=CARTESIAN_POINT('Ctrl Pts',(15.8839911682231,13.6178819280046,3.53270248607941));
#19867=CARTESIAN_POINT('Ctrl Pts',(15.637436117626,13.584036105808,3.54348792136362));
#19868=CARTESIAN_POINT('Ctrl Pts',(15.1393205736819,13.6125053812221,3.56527775268223));
#19869=CARTESIAN_POINT('Ctrl Pts',(14.8926763909184,13.6768418688357,3.57606708701133));
#19870=CARTESIAN_POINT('Ctrl Pts',(14.4490466142148,13.8929471500693,3.59547346394495));
#19871=CARTESIAN_POINT('Ctrl Pts',(14.2543404899168,14.0386737560065,3.60471802731944));
#19872=CARTESIAN_POINT('Ctrl Pts',(13.9239720590515,14.4011994334501,3.62567781129242));
#19873=CARTESIAN_POINT('Ctrl Pts',(13.7938087002647,14.6167467537565,3.63669054683468));
#19874=CARTESIAN_POINT('Ctrl Pts',(13.6334446299582,15.0594857800668,3.6569707427745));
#19875=CARTESIAN_POINT('Ctrl Pts',(13.595,15.2790287344985,3.66612875199322));
#19876=CARTESIAN_POINT('Ctrl Pts',(13.595,15.5000000000001,3.67449999999982));
#19877=CARTESIAN_POINT('Ctrl Pts',(13.595,15.5000000000001,3.73699999999998));
#19878=CARTESIAN_POINT('Ctrl Pts',(13.595,15.3107417523562,3.7298301640273));
#19879=CARTESIAN_POINT('Ctrl Pts',(13.6231998597127,15.1222187510603,3.72207138720419));
#19880=CARTESIAN_POINT('Ctrl Pts',(13.7525493543417,14.7010956562945,3.70328844558116));
#19881=CARTESIAN_POINT('Ctrl Pts',(13.8726887488314,14.4783897716366,3.69222376268828));
#19882=CARTESIAN_POINT('Ctrl Pts',(14.1864332416871,14.0993343465173,3.67100137099868));
#19883=CARTESIAN_POINT('Ctrl Pts',(14.3743188608229,13.9443260371385,3.66124239453956));
#19884=CARTESIAN_POINT('Ctrl Pts',(14.8075273411798,13.707459792369,3.64229189233668));
#19885=CARTESIAN_POINT('Ctrl Pts',(15.0508088855582,13.6315994557552,3.63164965504977));
#19886=CARTESIAN_POINT('Ctrl Pts',(15.5480838732381,13.5795702874817,3.60989659347145));
#19887=CARTESIAN_POINT('Ctrl Pts',(15.7970891607354,13.6020779774247,3.59900397372091));
#19888=CARTESIAN_POINT('Ctrl Pts',(16.266996803239,13.7395269848502,3.5784480838476));
#19889=CARTESIAN_POINT('Ctrl Pts',(16.4841055119923,13.8510363568198,3.56961118324191));
#19890=CARTESIAN_POINT('Ctrl Pts',(16.8749980751583,14.1571596683536,3.54946433958215));
#19891=CARTESIAN_POINT('Ctrl Pts',(17.0419363550534,14.3527181428317,3.53840450813985));
#19892=CARTESIAN_POINT('Ctrl Pts',(17.2843324468652,14.7892907094982,3.51656369539994));
#19893=CARTESIAN_POINT('Ctrl Pts',(17.3608108597669,15.0242378422134,3.5059902311861));
#19894=CARTESIAN_POINT('Ctrl Pts',(17.4209317256358,15.5125897526223,3.48617458843306));
#19895=CARTESIAN_POINT('Ctrl Pts',(17.4030963877,15.7614744775627,3.47705269701819));
#19896=CARTESIAN_POINT('Ctrl Pts',(17.2722116836178,16.2426311732042,3.45596187139847));
#19897=CARTESIAN_POINT('Ctrl Pts',(17.1588421845852,16.4697796343246,3.4448769594441));
#19898=CARTESIAN_POINT('Ctrl Pts',(16.8562303219055,16.8594962581601,3.42349417607325));
#19899=CARTESIAN_POINT('Ctrl Pts',(16.6727191440018,17.0206396007897,3.41337563638298));
#19900=CARTESIAN_POINT('Ctrl Pts',(16.2463442487807,17.2707735006488,3.39457380964476));
#19901=CARTESIAN_POINT('Ctrl Pts',(16.0054895868111,17.3539704573083,3.38411240537228));
#19902=CARTESIAN_POINT('Ctrl Pts',(15.5092285939096,17.4211032108309,3.36240370052097));
#19903=CARTESIAN_POINT('Ctrl Pts',(15.2589222384643,17.4059405573717,3.35145416616205));
#19904=CARTESIAN_POINT('Ctrl Pts',(14.7850580275298,17.2821722166527,3.3307251980547));
#19905=CARTESIAN_POINT('Ctrl Pts',(14.5652717116774,17.1773650722673,3.32176713122677));
#19906=CARTESIAN_POINT('Ctrl Pts',(14.167547187961,16.8846789705213,3.30197991069725));
#19907=CARTESIAN_POINT('Ctrl Pts',(13.9959811186205,16.6961082057814,3.29108358054212));
#19908=CARTESIAN_POINT('Ctrl Pts',(13.7398885692823,16.2689872877109,3.26930126032312));
#19909=CARTESIAN_POINT('Ctrl Pts',(13.6555080384971,16.0359080603258,3.25862572237898));
#19910=CARTESIAN_POINT('Ctrl Pts',(13.6025563404818,15.6959986001898,3.24459046094099));
#19911=CARTESIAN_POINT('Ctrl Pts',(13.595,15.5979667544917,3.2407113603725));
#19912=CARTESIAN_POINT('Ctrl Pts',(13.595,15.5,3.23699999999997));
#19913=CARTESIAN_POINT('Origin',(15.5,15.5,-1.713));
#19914=CARTESIAN_POINT('',(13.595,15.5,2.6744999999998));
#19915=CARTESIAN_POINT('',(13.595,15.5,2.73699999999996));
#19916=CARTESIAN_POINT('',(13.595,15.5,-1.713));
#19917=CARTESIAN_POINT('Ctrl Pts',(13.595,15.5,2.6744999999998));
#19918=CARTESIAN_POINT('Ctrl Pts',(13.595,15.6063456034545,2.67852878364688));
#19919=CARTESIAN_POINT('Ctrl Pts',(13.6039040754401,15.712737450423,2.68275407148365));
#19920=CARTESIAN_POINT('Ctrl Pts',(13.6628013387962,16.0605419293528,2.69721846982053));
#19921=CARTESIAN_POINT('Ctrl Pts',(13.7504283648582,16.2927748267109,2.70793295371105));
#19922=CARTESIAN_POINT('Ctrl Pts',(14.0125168018968,16.7166077868478,2.72972185699009));
#19923=CARTESIAN_POINT('Ctrl Pts',(14.1866415324471,16.9028008162696,2.74058407303392));
#19924=CARTESIAN_POINT('Ctrl Pts',(14.5881938303327,17.1899115237428,2.76024379811324));
#19925=CARTESIAN_POINT('Ctrl Pts',(14.809233833783,17.2916600718789,2.76928275738304));
#19926=CARTESIAN_POINT('Ctrl Pts',(15.2848913317403,17.4090895189284,2.79009017199187));
#19927=CARTESIAN_POINT('Ctrl Pts',(15.5357276212959,17.4208368072303,2.80106288807043));
#19928=CARTESIAN_POINT('Ctrl Pts',(16.0313680146098,17.3467242333267,2.82274444508332));
#19929=CARTESIAN_POINT('Ctrl Pts',(16.2710725586215,17.2601539276952,2.83301698439854));
#19930=CARTESIAN_POINT('Ctrl Pts',(16.6942270056888,17.0038614551219,2.85198168324288));
#19931=CARTESIAN_POINT('Ctrl Pts',(16.8756725561019,16.8398802310465,2.86216255292791));
#19932=CARTESIAN_POINT('Ctrl Pts',(17.1730083799238,16.4452310737242,2.88361680086033));
#19933=CARTESIAN_POINT('Ctrl Pts',(17.2831607273355,16.216074965942,2.89470740385587));
#19934=CARTESIAN_POINT('Ctrl Pts',(17.4066174506574,15.7334864081388,2.91569000719336));
#19935=CARTESIAN_POINT('Ctrl Pts',(17.420802952878,15.4852819804533,2.92471192923798));
#19936=CARTESIAN_POINT('Ctrl Pts',(17.35404340675,14.9983496347111,2.94461899635966));
#19937=CARTESIAN_POINT('Ctrl Pts',(17.2741679649323,14.7641723259516,2.95523759737822));
#19938=CARTESIAN_POINT('Ctrl Pts',(17.0252033879657,14.3304812783692,2.97711291466097));
#19939=CARTESIAN_POINT('Ctrl Pts',(16.8551691352643,14.1370789335407,2.98815877949576));
#19940=CARTESIAN_POINT('Ctrl Pts',(16.4597082538015,13.8367647917469,3.00818546876262));
#19941=CARTESIAN_POINT('Ctrl Pts',(16.2412799892886,13.7285875958632,3.01707305383682));
#19942=CARTESIAN_POINT('Ctrl Pts',(15.769401181861,13.5979038735229,3.03771517139708));
#19943=CARTESIAN_POINT('Ctrl Pts',(15.5197256729543,13.5790233888131,3.04863710966946));
#19944=CARTESIAN_POINT('Ctrl Pts',(15.0229509050475,13.6385205832759,3.07036828936789));
#19945=CARTESIAN_POINT('Ctrl Pts',(14.780850944374,13.7179975568388,3.08095883882865));
#19946=CARTESIAN_POINT('Ctrl Pts',(14.3510143352543,13.9614169703243,3.09976184010243));
#19947=CARTESIAN_POINT('Ctrl Pts',(14.1652766286123,14.1194307028667,3.10972544193732));
#19948=CARTESIAN_POINT('Ctrl Pts',(13.8569625944506,14.5037801398521,3.13102961487869));
#19949=CARTESIAN_POINT('Ctrl Pts',(13.7401357188322,14.7286974836181,3.14210562412025));
#19950=CARTESIAN_POINT('Ctrl Pts',(13.6202437330165,15.1424359669405,3.16040195089137));
#19951=CARTESIAN_POINT('Ctrl Pts',(13.595,15.3209351345322,3.16771632885281));
#19952=CARTESIAN_POINT('Ctrl Pts',(13.595,15.5000000000001,3.17449999999981));
#19953=CARTESIAN_POINT('Ctrl Pts',(13.595,15.5,3.23699999999997));
#19954=CARTESIAN_POINT('Ctrl Pts',(13.595,15.3537934880559,3.23146113064115));
#19955=CARTESIAN_POINT('Ctrl Pts',(13.6118292995507,15.2077601688887,3.22556072758023));
#19956=CARTESIAN_POINT('Ctrl Pts',(13.703020040462,14.8191615490059,3.20884455753866));
#19957=CARTESIAN_POINT('Ctrl Pts',(13.8088818890257,14.5874272503676,3.19775012561254));
#19958=CARTESIAN_POINT('Ctrl Pts',(14.0991475865153,14.186385786418,3.17620835201251));
#19959=CARTESIAN_POINT('Ctrl Pts',(14.2778058056202,14.0187054927708,3.16594831248646));
#19960=CARTESIAN_POINT('Ctrl Pts',(14.6979924612101,13.7534727151105,3.14670983255795));
#19961=CARTESIAN_POINT('Ctrl Pts',(14.9378342582387,13.6621805869591,3.13659167724224));
#19962=CARTESIAN_POINT('Ctrl Pts',(15.4343106839288,13.5799046605583,3.11487354838438));
#19963=CARTESIAN_POINT('Ctrl Pts',(15.6856914399172,13.587775485027,3.10387701487657));
#19964=CARTESIAN_POINT('Ctrl Pts',(16.1633494669556,13.6980228775345,3.08298208805948));
#19965=CARTESIAN_POINT('Ctrl Pts',(16.3858207901989,13.7963394742754,3.07383302272958));
#19966=CARTESIAN_POINT('Ctrl Pts',(16.7916343681647,14.0771739162689,3.05431786306173));
#19967=CARTESIAN_POINT('Ctrl Pts',(16.9685906134332,14.2606558327297,3.04349642284193));
#19968=CARTESIAN_POINT('Ctrl Pts',(17.2373587916645,14.6806975070553,3.02170504708823));
#19969=CARTESIAN_POINT('Ctrl Pts',(17.3286210834497,14.911927493209,3.01094904586258));
#19970=CARTESIAN_POINT('Ctrl Pts',(17.4176138080143,15.3939327184791,2.99074234716955));
#19971=CARTESIAN_POINT('Ctrl Pts',(17.415435860485,15.6399968762604,2.98192463162497));
#19972=CARTESIAN_POINT('Ctrl Pts',(17.3165773094733,16.1269857163728,2.96131334630555));
#19973=CARTESIAN_POINT('Ctrl Pts',(17.2173200906876,16.3624759378803,2.95022108368259));
#19974=CARTESIAN_POINT('Ctrl Pts',(16.9380102219418,16.7729589921194,2.92856125484767));
#19975=CARTESIAN_POINT('Ctrl Pts',(16.7637123739558,16.9461498976184,2.91818782318278));
#19976=CARTESIAN_POINT('Ctrl Pts',(16.3527147432174,17.2219567273831,2.89874974197185));
#19977=CARTESIAN_POINT('Ctrl Pts',(16.1182155734959,17.3193652589469,2.88904355089655));
#19978=CARTESIAN_POINT('Ctrl Pts',(15.626445026524,17.4171549396238,2.86753127850061));
#19979=CARTESIAN_POINT('Ctrl Pts',(15.3741392554428,17.4171933827677,2.85649428064055));
#19980=CARTESIAN_POINT('Ctrl Pts',(14.8925123198339,17.3215733653222,2.83542573577579));
#19981=CARTESIAN_POINT('Ctrl Pts',(14.6670879670194,17.2301446596474,2.82599357878335));
#19982=CARTESIAN_POINT('Ctrl Pts',(14.2528348239649,16.9619561037788,2.80677290188424));
#19983=CARTESIAN_POINT('Ctrl Pts',(14.0703326623383,16.7840422422845,2.79604109941036));
#19984=CARTESIAN_POINT('Ctrl Pts',(13.7883374842567,16.3719205442741,2.77426045859807));
#19985=CARTESIAN_POINT('Ctrl Pts',(13.6898170858119,16.1428698537008,2.76342826629651));
#19986=CARTESIAN_POINT('Ctrl Pts',(13.6092718154206,15.7691888526544,2.74751007403869));
#19987=CARTESIAN_POINT('Ctrl Pts',(13.595,15.6346391293541,2.74210065207189));
#19988=CARTESIAN_POINT('Ctrl Pts',(13.595,15.5,2.73699999999996));
#19989=CARTESIAN_POINT('Origin',(15.5,15.5,-1.713));
#19990=CARTESIAN_POINT('',(13.595,15.5,2.1744999999998));
#19991=CARTESIAN_POINT('',(13.595,15.5,2.23699999999995));
#19992=CARTESIAN_POINT('',(13.595,15.5,-1.713));
#19993=CARTESIAN_POINT('Ctrl Pts',(13.595,15.5,2.1744999999998));
#19994=CARTESIAN_POINT('Ctrl Pts',(13.595,15.6438717177873,2.17995041830644));
#19995=CARTESIAN_POINT('Ctrl Pts',(13.6112960890959,15.7875810170524,2.18575111596478));
#19996=CARTESIAN_POINT('Ctrl Pts',(13.6994181942645,16.1694219103305,2.20214415911293));
#19997=CARTESIAN_POINT('Ctrl Pts',(13.8014664402575,16.39732693886,2.21301011131559));
#19998=CARTESIAN_POINT('Ctrl Pts',(14.0898370033197,16.805428282584,2.23477788964081));
#19999=CARTESIAN_POINT('Ctrl Pts',(14.2749823259478,16.9805603547105,2.24546211907182));
#20000=CARTESIAN_POINT('Ctrl Pts',(14.6933096159863,17.2425418310181,2.26453675856539));
#20001=CARTESIAN_POINT('Ctrl Pts',(14.9202192490859,17.3305984944438,2.2741377624269));
#20002=CARTESIAN_POINT('Ctrl Pts',(15.4037619976461,17.4189587852763,2.29529011363254));
#20003=CARTESIAN_POINT('Ctrl Pts',(15.6564353891663,17.4149918847535,2.30634319287666));
#20004=CARTESIAN_POINT('Ctrl Pts',(16.1458020926397,17.3095906453332,2.32775031026398));
#20005=CARTESIAN_POINT('Ctrl Pts',(16.3776914452839,17.2091865162443,2.33727982413664));
#20006=CARTESIAN_POINT('Ctrl Pts',(16.7840902788011,16.9281437430753,2.35681567706199));
#20007=CARTESIAN_POINT('Ctrl Pts',(16.9561453578496,16.7522394033176,2.36724284969501));
#20008=CARTESIAN_POINT('Ctrl Pts',(17.2298657636766,16.3371446453742,2.38895513352139));
#20009=CARTESIAN_POINT('Ctrl Pts',(17.3257728014476,16.0998440762515,2.40004270307863));
#20010=CARTESIAN_POINT('Ctrl Pts',(17.4172222954957,15.6116271944855,2.42053845851129));
#20011=CARTESIAN_POINT('Ctrl Pts',(17.4158006733317,15.3661710612252,2.42933372371272));
#20012=CARTESIAN_POINT('Ctrl Pts',(17.320031940749,14.8857206145777,2.44962972801491));
#20013=CARTESIAN_POINT('Ctrl Pts',(17.2253022083536,14.6555021357188,2.46042325020695));
#20014=CARTESIAN_POINT('Ctrl Pts',(16.9501966716434,14.2391854988472,2.48221211949409));
#20015=CARTESIAN_POINT('Ctrl Pts',(16.7705729717939,14.0583377226447,2.49299211154719));
#20016=CARTESIAN_POINT('Ctrl Pts',(16.3607170029023,13.7835246991033,2.51236757279492));
#20017=CARTESIAN_POINT('Ctrl Pts',(16.1368514548924,13.6884915883818,2.52164123119447));
#20018=CARTESIAN_POINT('Ctrl Pts',(15.6572929705878,13.585182428074,2.5426192926251));
#20019=CARTESIAN_POINT('Ctrl Pts',(15.4054427164359,13.5810615146841,2.55363636411031));
#20020=CARTESIAN_POINT('Ctrl Pts',(14.9111746682304,13.67072563478,2.57525788852872));
#20021=CARTESIAN_POINT('Ctrl Pts',(14.6738807357029,13.7649330778004,2.58517137358941));
#20022=CARTESIAN_POINT('Ctrl Pts',(14.2580399017547,14.0351855492971,2.60450496600958));
#20023=CARTESIAN_POINT('Ctrl Pts',(14.0814234721209,14.205486405278,2.61481962403155));
#20024=CARTESIAN_POINT('Ctrl Pts',(13.7963031328522,14.6110302058985,2.63641942295186));
#20025=CARTESIAN_POINT('Ctrl Pts',(13.6935495615298,14.8445635980581,2.64751402644718));
#20026=CARTESIAN_POINT('Ctrl Pts',(13.6098017218543,15.2258696997939,2.66379113452061));
#20027=CARTESIAN_POINT('Ctrl Pts',(13.595,15.3628839986378,2.66930551441603));
#20028=CARTESIAN_POINT('Ctrl Pts',(13.595,15.5,2.6744999999998));
#20029=CARTESIAN_POINT('Ctrl Pts',(13.595,15.5,2.73699999999997));
#20030=CARTESIAN_POINT('Ctrl Pts',(13.595,15.3930282082835,2.73294749391445));
#20031=CARTESIAN_POINT('Ctrl Pts',(13.6040092351669,15.2860150896782,2.7286963698185));
#20032=CARTESIAN_POINT('Ctrl Pts',(13.6646854787885,14.9298303122742,2.71387558296442));
#20033=CARTESIAN_POINT('Ctrl Pts',(13.7569133947645,14.6906125998951,2.70279585532033));
#20034=CARTESIAN_POINT('Ctrl Pts',(14.0244715433773,14.2705861319543,2.68103152173303));
#20035=CARTESIAN_POINT('Ctrl Pts',(14.1940405065733,14.0917631521739,2.67054815669065));
#20036=CARTESIAN_POINT('Ctrl Pts',(14.5954328728501,13.8050617550424,2.65090743594019));
#20037=CARTESIAN_POINT('Ctrl Pts',(14.8245298971626,13.7014420434005,2.64154812348355));
#20038=CARTESIAN_POINT('Ctrl Pts',(15.3112471846211,13.5878678116446,2.6202569035597));
#20039=CARTESIAN_POINT('Ctrl Pts',(15.5642504683678,13.5796494726171,2.60918939333455));
#20040=CARTESIAN_POINT('Ctrl Pts',(16.0498253014062,13.6601516696882,2.58794814954459));
#20041=CARTESIAN_POINT('Ctrl Pts',(16.2783576488718,13.7445899106109,2.57814395918767));
#20042=CARTESIAN_POINT('Ctrl Pts',(16.7010127006999,13.9999050425915,2.55922720869861));
#20043=CARTESIAN_POINT('Ctrl Pts',(16.8889380307444,14.1720159053704,2.54859662932607));
#20044=CARTESIAN_POINT('Ctrl Pts',(17.1840673178039,14.5757054590094,2.52684815810019));
#20045=CARTESIAN_POINT('Ctrl Pts',(17.2898773392592,14.802325578808,2.51594860466704));
#20046=CARTESIAN_POINT('Ctrl Pts',(17.407369479363,15.2776195184105,2.495372808691));
#20047=CARTESIAN_POINT('Ctrl Pts',(17.4201702625757,15.5212734828779,2.4865258860317));
#20048=CARTESIAN_POINT('Ctrl Pts',(17.35219055494,16.0131036479769,2.4664065828322));
#20049=CARTESIAN_POINT('Ctrl Pts',(17.2670854108525,16.2558290618805,2.45534976101996));
#20050=CARTESIAN_POINT('Ctrl Pts',(17.011526099875,16.685021789749,2.43350061574692));
#20051=CARTESIAN_POINT('Ctrl Pts',(16.8468366025359,16.8693193346392,2.42291657793418));
#20052=CARTESIAN_POINT('Ctrl Pts',(16.4550191957345,17.1667248449986,2.40307976994657));
#20053=CARTESIAN_POINT('Ctrl Pts',(16.2311205707705,17.2763735831971,2.39398252715528));
#20054=CARTESIAN_POINT('Ctrl Pts',(15.7495521891942,17.4052566407165,2.37291654370927));
#20055=CARTESIAN_POINT('Ctrl Pts',(15.4961161692798,17.4215250171174,2.36183010364304));
#20056=CARTESIAN_POINT('Ctrl Pts',(15.0069194685944,17.3559364307211,2.34043042294816));
#20057=CARTESIAN_POINT('Ctrl Pts',(14.7752765137846,17.2783217792191,2.33029731031432));
#20058=CARTESIAN_POINT('Ctrl Pts',(14.3445994938058,17.035488255536,2.31145754566084));
#20059=CARTESIAN_POINT('Ctrl Pts',(14.1515761993843,16.8691175909564,2.30104106361459));
#20060=CARTESIAN_POINT('Ctrl Pts',(13.8439774695534,16.473833045966,2.27933827172479));
#20061=CARTESIAN_POINT('Ctrl Pts',(13.7312096376842,16.2497646250875,2.26838320345701));
#20062=CARTESIAN_POINT('Ctrl Pts',(13.6183400493023,15.8438701603391,2.2505376342567));
#20063=CARTESIAN_POINT('Ctrl Pts',(13.595,15.672181316349,2.24352289562618));
#20064=CARTESIAN_POINT('Ctrl Pts',(13.595,15.4999999999999,2.23699999999995));
#20065=CARTESIAN_POINT('Origin',(15.5,15.5,-1.713));
#20066=CARTESIAN_POINT('',(13.595,15.4999999999999,1.67449999999978));
#20067=CARTESIAN_POINT('',(13.595,15.5,1.73699999999994));
#20068=CARTESIAN_POINT('',(13.595,15.5,-1.713));
#20069=CARTESIAN_POINT('Ctrl Pts',(13.595,15.4999999999999,1.67449999999978));
#20070=CARTESIAN_POINT('Ctrl Pts',(13.595,15.6805943382424,1.68134161350361));
#20071=CARTESIAN_POINT('Ctrl Pts',(13.6206767895374,15.8605641359682,1.68872117656185));
#20072=CARTESIAN_POINT('Ctrl Pts',(13.7413289123729,16.2733083137167,1.70699646110305));
#20073=CARTESIAN_POINT('Ctrl Pts',(13.8572511397691,16.4961436352298,1.71797380856537));
#20074=CARTESIAN_POINT('Ctrl Pts',(14.1704568500251,16.8874656850136,1.73964912314549));
#20075=CARTESIAN_POINT('Ctrl Pts',(14.3657712252737,17.0512012839823,1.74988369314374));
#20076=CARTESIAN_POINT('Ctrl Pts',(14.8000789722952,17.2882735425523,1.76888228225231));
#20077=CARTESIAN_POINT('Ctrl Pts',(15.0331083699897,17.3627401021875,1.77907604418122));
#20078=CARTESIAN_POINT('Ctrl Pts',(15.5238841860569,17.4214287213786,1.80054480253939));
#20079=CARTESIAN_POINT('Ctrl Pts',(15.7774357888171,17.4014455462687,1.81163629872315));
#20080=CARTESIAN_POINT('Ctrl Pts',(16.2565712745634,17.2655644201264,1.83259585627988));
#20081=CARTESIAN_POINT('Ctrl Pts',(16.4781090057824,17.1531532245574,1.84159894199786));
#20082=CARTESIAN_POINT('Ctrl Pts',(16.865460791257,16.8508077335818,1.86152522234094));
#20083=CARTESIAN_POINT('Ctrl Pts',(17.027820762239,16.6640072719447,1.87215312832116));
#20084=CARTESIAN_POINT('Ctrl Pts',(17.277693383932,16.2306622638974,1.89403519728088));
#20085=CARTESIAN_POINT('Ctrl Pts',(17.3594407795806,15.9863735004033,1.90507780326818));
#20086=CARTESIAN_POINT('Ctrl Pts',(17.4202398674738,15.4935193143535,1.92507884392557));
#20087=CARTESIAN_POINT('Ctrl Pts',(17.4039583455681,15.2503744699176,1.93397956595357));
#20088=CARTESIAN_POINT('Ctrl Pts',(17.2797387468027,14.7767335439119,1.95463988413274));
#20089=CARTESIAN_POINT('Ctrl Pts',(17.1705139566369,14.5513370860411,1.96556776923869));
#20090=CARTESIAN_POINT('Ctrl Pts',(16.8692851398174,14.1517652070239,1.98729365752725));
#20091=CARTESIAN_POINT('Ctrl Pts',(16.6788710179229,13.9824464372533,1.99787289711194));
#20092=CARTESIAN_POINT('Ctrl Pts',(16.2522998301226,13.7332282337451,2.01664432708673));
#20093=CARTESIAN_POINT('Ctrl Pts',(16.022257718409,13.652098771619,2.02665408055944));
#20094=CARTESIAN_POINT('Ctrl Pts',(15.5348488553472,13.5788405414173,2.04797555313431));
#20095=CARTESIAN_POINT('Ctrl Pts',(15.2816037882842,13.5909752658634,2.05905364005744));
#20096=CARTESIAN_POINT('Ctrl Pts',(14.7973701563817,13.7120232043683,2.08023621363144));
#20097=CARTESIAN_POINT('Ctrl Pts',(14.5708164836265,13.8185845683307,2.08945814873325));
#20098=CARTESIAN_POINT('Ctrl Pts',(14.174065869201,14.1104943182623,2.10919465644389));
#20099=CARTESIAN_POINT('Ctrl Pts',(14.0068423137263,14.2919892661037,2.11972794661126));
#20100=CARTESIAN_POINT('Ctrl Pts',(13.7450669096734,14.7165035768415,2.14153581535119));
#20101=CARTESIAN_POINT('Ctrl Pts',(13.6562783501935,14.9574480480878,2.1526057327939));
#20102=CARTESIAN_POINT('Ctrl Pts',(13.6024563313451,15.3053056555503,2.1669611367478));
#20103=CARTESIAN_POINT('Ctrl Pts',(13.595,15.4026837338876,2.17081328264832));
#20104=CARTESIAN_POINT('Ctrl Pts',(13.595,15.5,2.1744999999998));
#20105=CARTESIAN_POINT('Ctrl Pts',(13.595,15.4999999999999,2.23699999999995));
#20106=CARTESIAN_POINT('Ctrl Pts',(13.595,15.431751208773,2.23441447126066));
#20107=CARTESIAN_POINT('Ctrl Pts',(13.5986674333316,15.3634311572752,2.2317460278289));
#20108=CARTESIAN_POINT('Ctrl Pts',(13.6331507396179,15.0443258754603,2.21890285487715));
#20109=CARTESIAN_POINT('Ctrl Pts',(13.7099023892996,14.8012177434886,2.20801424407246));
#20110=CARTESIAN_POINT('Ctrl Pts',(13.9504037976665,14.3650453166575,2.18623003120062));
#20111=CARTESIAN_POINT('Ctrl Pts',(14.109523173235,14.1748740307419,2.17554530449642));
#20112=CARTESIAN_POINT('Ctrl Pts',(14.4907642526035,13.8658220120849,2.15549860987993));
#20113=CARTESIAN_POINT('Ctrl Pts',(14.7091363539253,13.7496765856905,2.14659596002061));
#20114=CARTESIAN_POINT('Ctrl Pts',(15.1849155528709,13.6043623820501,2.12578322165901));
#20115=CARTESIAN_POINT('Ctrl Pts',(15.4385395576878,13.5793402113641,2.11468855828118));
#20116=CARTESIAN_POINT('Ctrl Pts',(15.9313006918732,13.6286407381194,2.0931329531112));
#20117=CARTESIAN_POINT('Ctrl Pts',(16.1661388964057,13.6988096067292,2.08286006577382));
#20118=CARTESIAN_POINT('Ctrl Pts',(16.6064383681386,13.928626421797,2.06359937147228));
#20119=CARTESIAN_POINT('Ctrl Pts',(16.8057127521754,14.0898333101884,2.05353034999365));
#20120=CARTESIAN_POINT('Ctrl Pts',(17.1264426786317,14.4773522669783,2.03183453965873));
#20121=CARTESIAN_POINT('Ctrl Pts',(17.2461296157387,14.6986524180764,2.02083300766985));
#20122=CARTESIAN_POINT('Ctrl Pts',(17.3911031791095,15.1670180712176,1.99991860103969));
#20123=CARTESIAN_POINT('Ctrl Pts',(17.4180203684862,15.4087388151163,1.99074211236779));
#20124=CARTESIAN_POINT('Ctrl Pts',(17.3794084666146,15.9007187389138,1.97125947618687));
#20125=CARTESIAN_POINT('Ctrl Pts',(17.3098301237469,16.1459452707687,1.96044750865836));
#20126=CARTESIAN_POINT('Ctrl Pts',(17.081936726472,16.589581810925,1.93865629201535));
#20127=CARTESIAN_POINT('Ctrl Pts',(16.9279232039071,16.7848188928723,1.92789132989771));
#20128=CARTESIAN_POINT('Ctrl Pts',(16.5560962147641,17.1040830769658,1.90766366635815));
#20129=CARTESIAN_POINT('Ctrl Pts',(16.3424560638699,17.2258881558211,1.89885284618849));
#20130=CARTESIAN_POINT('Ctrl Pts',(15.8718978195449,17.3854182082523,1.87826849604306));
#20131=CARTESIAN_POINT('Ctrl Pts',(15.6183489024308,17.4180958936047,1.86717711734167));
#20132=CARTESIAN_POINT('Ctrl Pts',(15.1229151224816,17.3831207028366,1.84550459853377));
#20133=CARTESIAN_POINT('Ctrl Pts',(14.8854864440878,17.319541139132,1.83511839212985));
#20134=CARTESIAN_POINT('Ctrl Pts',(14.4406052940417,17.1030585739811,1.81565727445506));
#20135=CARTESIAN_POINT('Ctrl Pts',(14.2386939916263,16.9495664214194,1.805994240649));
#20136=CARTESIAN_POINT('Ctrl Pts',(13.9068481615258,16.5739572903711,1.78450649067386));
#20137=CARTESIAN_POINT('Ctrl Pts',(13.7798172168087,16.3558550703986,1.77346547862325));
#20138=CARTESIAN_POINT('Ctrl Pts',(13.629909999065,15.9199032586047,1.75367112373648));
#20139=CARTESIAN_POINT('Ctrl Pts',(13.595,15.710569767174,1.74497719893441));
#20140=CARTESIAN_POINT('Ctrl Pts',(13.595,15.5,1.73699999999994));
#20141=CARTESIAN_POINT('Origin',(-15.5,15.5,-1.713));
#20142=CARTESIAN_POINT('',(-17.405,15.5,10.2995));
#20143=CARTESIAN_POINT('',(-17.405,15.5,10.362));
#20144=CARTESIAN_POINT('',(-17.405,15.5,-1.713));
#20145=CARTESIAN_POINT('',(-16.8346987578547,14.140733938563,10.7369999999983));
#20146=CARTESIAN_POINT('Ctrl Pts',(-17.405,15.5,10.2995));
#20147=CARTESIAN_POINT('Ctrl Pts',(-17.405,15.5040685861377,10.2996779783962));
#20148=CARTESIAN_POINT('Ctrl Pts',(-17.4049869658359,15.5081378012993,10.2998559843088));
#20149=CARTESIAN_POINT('Ctrl Pts',(-17.4033906330436,15.7572412627348,10.3107528986323));
#20150=CARTESIAN_POINT('Ctrl Pts',(-17.3545571787606,15.9997025387586,10.321359253664));
#20151=CARTESIAN_POINT('Ctrl Pts',(-17.1671265552,16.4542045755556,10.3412412325265));
#20152=CARTESIAN_POINT('Ctrl Pts',(-17.0297788069357,16.661722890711,10.3502888948547));
#20153=CARTESIAN_POINT('Ctrl Pts',(-16.6799939284003,17.0165709526528,10.3713014329842));
#20154=CARTESIAN_POINT('Ctrl Pts',(-16.4695260417865,17.1590316553049,10.3823907106664));
#20155=CARTESIAN_POINT('Ctrl Pts',(-16.0141127709042,17.3502424572529,10.4038257440338));
#20156=CARTESIAN_POINT('Ctrl Pts',(-15.7748789785151,17.4005720901235,10.4139896704593));
#20157=CARTESIAN_POINT('Ctrl Pts',(-15.2803405005136,17.4090409031514,10.4329099369341));
#20158=CARTESIAN_POINT('Ctrl Pts',(-15.0296503702655,17.3631985762762,10.4432329588745));
#20159=CARTESIAN_POINT('Ctrl Pts',(-14.5641602654383,17.1778105668438,10.4649223841023));
#20160=CARTESIAN_POINT('Ctrl Pts',(-14.353395506391,17.041475523071,10.4758889264227));
#20161=CARTESIAN_POINT('Ctrl Pts',(-14.001475342609,16.7006854117087,10.4966748781996));
#20162=CARTESIAN_POINT('Ctrl Pts',(-13.8616419045569,16.5014953707221,10.5056900537741));
#20163=CARTESIAN_POINT('Ctrl Pts',(-13.6591140212472,16.0512722065885,10.5253848553548));
#20164=CARTESIAN_POINT('Ctrl Pts',(-13.6023464090874,15.8027433923608,10.5362566320052));
#20165=CARTESIAN_POINT('Ctrl Pts',(-13.5891625890781,15.304680938602,10.5580441409185));
#20166=CARTESIAN_POINT('Ctrl Pts',(-13.6302802412451,15.0599877380409,10.5687481304444));
#20167=CARTESIAN_POINT('Ctrl Pts',(-13.8028590578393,14.6007565222116,10.5888369850301));
#20168=CARTESIAN_POINT('Ctrl Pts',(-13.9322886349895,14.3904011858836,10.5977117908643));
#20169=CARTESIAN_POINT('Ctrl Pts',(-14.2689778421792,14.0244002544545,10.6184721527331));
#20170=CARTESIAN_POINT('Ctrl Pts',(-14.4752263247542,13.8743802194899,10.629566922763));
#20171=CARTESIAN_POINT('Ctrl Pts',(-14.9255315746248,13.6674966826003,10.6511512427232));
#20172=CARTESIAN_POINT('Ctrl Pts',(-15.1637660001395,13.6092195380962,10.6614511393463));
#20173=CARTESIAN_POINT('Ctrl Pts',(-15.6593655361598,13.5848746537428,10.6807588484659));
#20174=CARTESIAN_POINT('Ctrl Pts',(-15.9121754512101,13.6229689888941,10.6907265488194));
#20175=CARTESIAN_POINT('Ctrl Pts',(-16.2782877509633,13.7559038448062,10.7075038882848));
#20176=CARTESIAN_POINT('Ctrl Pts',(-16.4010418909404,13.8160386819109,10.7134695760448));
#20177=CARTESIAN_POINT('Ctrl Pts',(-16.6311209277075,13.9611652333068,10.725360108259));
#20178=CARTESIAN_POINT('Ctrl Pts',(-16.7378480595021,14.0456337146558,10.7312508627682));
#20179=CARTESIAN_POINT('Ctrl Pts',(-16.8346987578564,14.1407339385622,10.7369999999993));
#20180=CARTESIAN_POINT('',(-15.5,13.595,10.737));
#20181=CARTESIAN_POINT('Origin',(-15.5,15.5,10.737));
#20182=CARTESIAN_POINT('Ctrl Pts',(-15.5000000000006,13.595,10.737));
#20183=CARTESIAN_POINT('Ctrl Pts',(-15.3699120138899,13.595,10.7320717628741));
#20184=CARTESIAN_POINT('Ctrl Pts',(-15.2401373096739,13.6083238613174,10.7268639710421));
#20185=CARTESIAN_POINT('Ctrl Pts',(-14.9809515435032,13.6621430987188,10.7158678609589));
#20186=CARTESIAN_POINT('Ctrl Pts',(-14.8524833192468,13.7033785949584,10.7100990729491));
#20187=CARTESIAN_POINT('Ctrl Pts',(-14.4988222300249,13.8597998187566,10.6932797335136));
#20188=CARTESIAN_POINT('Ctrl Pts',(-14.2907287000254,14.0065862685042,10.6821857917719));
#20189=CARTESIAN_POINT('Ctrl Pts',(-13.9483989836387,14.3678225922382,10.6613159583192));
#20190=CARTESIAN_POINT('Ctrl Pts',(-13.8155791216889,14.5769539155351,10.6523782189181));
#20191=CARTESIAN_POINT('Ctrl Pts',(-13.6365911873295,15.0341600256621,10.6323779516335));
#20192=CARTESIAN_POINT('Ctrl Pts',(-13.5921308386535,15.2779191745305,10.6217148217617));
#20193=CARTESIAN_POINT('Ctrl Pts',(-13.598241495346,15.7757974377006,10.5999353701795));
#20194=CARTESIAN_POINT('Ctrl Pts',(-13.6514821744474,16.0251188925287,10.589028919837));
#20195=CARTESIAN_POINT('Ctrl Pts',(-13.8476887277444,16.4783498191008,10.5692025450963));
#20196=CARTESIAN_POINT('Ctrl Pts',(-13.9848206347882,16.6796359062972,10.5602662234653));
#20197=CARTESIAN_POINT('Ctrl Pts',(-14.3318591399905,17.0251635041763,10.5395615882713));
#20198=CARTESIAN_POINT('Ctrl Pts',(-14.5403762591266,17.1642696671436,10.5286195846064));
#20199=CARTESIAN_POINT('Ctrl Pts',(-15.0027926478457,17.3562075644913,10.5069033427678));
#20200=CARTESIAN_POINT('Ctrl Pts',(-15.2527557847393,17.4056576180186,10.496380952772));
#20201=CARTESIAN_POINT('Ctrl Pts',(-15.7469658100237,17.4043563226145,10.477629899211));
#20202=CARTESIAN_POINT('Ctrl Pts',(-15.986566461954,17.3576312123841,10.467530913802));
#20203=CARTESIAN_POINT('Ctrl Pts',(-16.4441204477045,17.1735616671745,10.4461709773248));
#20204=CARTESIAN_POINT('Ctrl Pts',(-16.6564133010635,17.0345635599908,10.4350882976379));
#20205=CARTESIAN_POINT('Ctrl Pts',(-17.0120945880556,16.6848444658985,10.4139645628509));
#20206=CARTESIAN_POINT('Ctrl Pts',(-17.1530634482971,16.4786007112435,10.4048084300633));
#20207=CARTESIAN_POINT('Ctrl Pts',(-17.347151124169,16.0262599452583,10.3850209949808));
#20208=CARTESIAN_POINT('Ctrl Pts',(-17.3994067137205,15.7848752872053,10.3744617360984));
#20209=CARTESIAN_POINT('Ctrl Pts',(-17.4048584739919,15.526819595538,10.3631732106536));
#20210=CARTESIAN_POINT('Ctrl Pts',(-17.405,15.5134066598368,10.3625864680594));
#20211=CARTESIAN_POINT('Ctrl Pts',(-17.405,15.5,10.362));
#20212=CARTESIAN_POINT('Origin',(-15.5,15.5,-1.713));
#20213=CARTESIAN_POINT('',(-17.405,15.5,9.79949999999996));
#20214=CARTESIAN_POINT('',(-17.405,15.5,9.862));
#20215=CARTESIAN_POINT('',(-17.405,15.5,-1.713));
#20216=CARTESIAN_POINT('Ctrl Pts',(-17.405,15.5,9.79949999999996));
#20217=CARTESIAN_POINT('Ctrl Pts',(-17.405,15.5422757379386,9.80134933236823));
#20218=CARTESIAN_POINT('Ctrl Pts',(-17.40359275119,15.5845971736778,9.80320066376537));
#20219=CARTESIAN_POINT('Ctrl Pts',(-17.3845405641599,15.8699821476011,9.8156846958705));
#20220=CARTESIAN_POINT('Ctrl Pts',(-17.3218280438504,16.1077355872408,9.82608510880312));
#20221=CARTESIAN_POINT('Ctrl Pts',(-17.1070822286942,16.553205723457,9.84557199140226));
#20222=CARTESIAN_POINT('Ctrl Pts',(-16.9545805300396,16.755456643589,9.85518786661981));
#20223=CARTESIAN_POINT('Ctrl Pts',(-16.5805208159003,17.0887237001984,9.8766480041212));
#20224=CARTESIAN_POINT('Ctrl Pts',(-16.3628499713819,17.2166995848147,9.8876933419744));
#20225=CARTESIAN_POINT('Ctrl Pts',(-15.8989163528556,17.3783142982288,9.90880382561483));
#20226=CARTESIAN_POINT('Ctrl Pts',(-15.6581811203113,17.4136735025017,9.91831777690985));
#20227=CARTESIAN_POINT('Ctrl Pts',(-15.1651164143754,17.3922433860113,9.93746570426309));
#20228=CARTESIAN_POINT('Ctrl Pts',(-14.9176522095134,17.3312779904081,9.94817405884487));
#20229=CARTESIAN_POINT('Ctrl Pts',(-14.4656105936897,17.1186912299103,9.96994890150104));
#20230=CARTESIAN_POINT('Ctrl Pts',(-14.2645197804293,16.970959077615,9.98079823784833));
#20231=CARTESIAN_POINT('Ctrl Pts',(-13.9332143050592,16.6104026181867,10.0012355601492));
#20232=CARTESIAN_POINT('Ctrl Pts',(-13.8047642566147,16.4022110329364,10.0100332006589));
#20233=CARTESIAN_POINT('Ctrl Pts',(-13.628699972833,15.9379596044362,10.0303416620981));
#20234=CARTESIAN_POINT('Ctrl Pts',(-13.5870407057066,15.6847822439277,10.0414167872297));
#20235=CARTESIAN_POINT('Ctrl Pts',(-13.6051138243238,15.1867387248958,10.0632034678523));
#20236=CARTESIAN_POINT('Ctrl Pts',(-13.6608710205603,14.9465120725361,10.0737120703177));
#20237=CARTESIAN_POINT('Ctrl Pts',(-13.8618203853613,14.4964258783141,10.0934008802136));
#20238=CARTESIAN_POINT('Ctrl Pts',(-14.0065697067588,14.2915005667656,10.1026890264168));
#20239=CARTESIAN_POINT('Ctrl Pts',(-14.3683432847775,13.9471548902683,10.1239260319824));
#20240=CARTESIAN_POINT('Ctrl Pts',(-14.5824715741539,13.8117722617144,10.1349991663895));
#20241=CARTESIAN_POINT('Ctrl Pts',(-15.0422282039318,13.635097453793,10.156280807899));
#20242=CARTESIAN_POINT('Ctrl Pts',(-15.2821853899945,13.5921415314096,10.1661858171533));
#20243=CARTESIAN_POINT('Ctrl Pts',(-15.776049388456,13.5982881804018,10.1850297407394));
#20244=CARTESIAN_POINT('Ctrl Pts',(-16.0252412858902,13.651539455332,10.1956348217132));
#20245=CARTESIAN_POINT('Ctrl Pts',(-16.484306788393,13.8502633168274,10.2173725434068));
#20246=CARTESIAN_POINT('Ctrl Pts',(-16.6904337512215,13.992231707287,10.2282866020876));
#20247=CARTESIAN_POINT('Ctrl Pts',(-17.0323456700082,14.3426958132205,10.2489049949351));
#20248=CARTESIAN_POINT('Ctrl Pts',(-17.1666456642617,14.5462062897174,10.2577767405825));
#20249=CARTESIAN_POINT('Ctrl Pts',(-17.3555164898945,15.0010180770042,10.2776722693352));
#20250=CARTESIAN_POINT('Ctrl Pts',(-17.405,15.2493150318857,10.288533903407));
#20251=CARTESIAN_POINT('Ctrl Pts',(-17.405,15.5,10.2995));
#20252=CARTESIAN_POINT('Ctrl Pts',(-17.405,15.5,10.362));
#20253=CARTESIAN_POINT('Ctrl Pts',(-17.405,15.2592217904251,10.3514672699224));
#20254=CARTESIAN_POINT('Ctrl Pts',(-17.3593488079492,15.0204678429165,10.3410230902414));
#20255=CARTESIAN_POINT('Ctrl Pts',(-17.1809462278487,14.5715506218093,10.3213854165272));
#20256=CARTESIAN_POINT('Ctrl Pts',(-17.0495359155277,14.3657421139465,10.3125603028827));
#20257=CARTESIAN_POINT('Ctrl Pts',(-16.7128616771596,14.0102742229046,10.2920308895517));
#20258=CARTESIAN_POINT('Ctrl Pts',(-16.5092067974019,13.8654327846184,10.281147642893));
#20259=CARTESIAN_POINT('Ctrl Pts',(-16.0535638696873,13.6598196462403,10.2593888975018));
#20260=CARTESIAN_POINT('Ctrl Pts',(-15.8051960491987,13.602744809826,10.248731405803));
#20261=CARTESIAN_POINT('Ctrl Pts',(-15.3117087298555,13.5890330071187,10.2297362852278));
#20262=CARTESIAN_POINT('Ctrl Pts',(-15.0713779050357,13.6282170971557,10.2200356005496));
#20263=CARTESIAN_POINT('Ctrl Pts',(-14.6095248225641,13.7974066753042,10.1988382562227));
#20264=CARTESIAN_POINT('Ctrl Pts',(-14.3936055605611,13.9291201388172,10.1877775257845));
#20265=CARTESIAN_POINT('Ctrl Pts',(-14.0257138194173,14.2679906029282,10.1664284957877));
#20266=CARTESIAN_POINT('Ctrl Pts',(-13.8771261361364,14.4715876659088,10.1569874161896));
#20267=CARTESIAN_POINT('Ctrl Pts',(-13.6693004494634,14.9193870498654,10.1373986417383));
#20268=CARTESIAN_POINT('Ctrl Pts',(-13.6100619110029,15.1584049022711,10.1269429176611));
#20269=CARTESIAN_POINT('Ctrl Pts',(-13.5844801810218,15.6553609522086,10.105203807865));
#20270=CARTESIAN_POINT('Ctrl Pts',(-13.6221561794649,15.9087408059525,10.0941198247616));
#20271=CARTESIAN_POINT('Ctrl Pts',(-13.7909044092091,16.3758135735006,10.0736879451663));
#20272=CARTESIAN_POINT('Ctrl Pts',(-13.9164043028326,16.5864082562103,10.0648971992549));
#20273=CARTESIAN_POINT('Ctrl Pts',(-14.2423599818571,16.951995676498,10.0445525094611));
#20274=CARTESIAN_POINT('Ctrl Pts',(-14.4408670269628,17.1025531980931,10.0337392590372));
#20275=CARTESIAN_POINT('Ctrl Pts',(-14.8892292103314,17.3219982202937,10.0119538018197));
#20276=CARTESIAN_POINT('Ctrl Pts',(-15.1357348020651,17.3868100515806,10.0011976329544));
#20277=CARTESIAN_POINT('Ctrl Pts',(-15.6283411562131,17.4158954713742,9.98189963091358));
#20278=CARTESIAN_POINT('Ctrl Pts',(-15.8695009053101,17.384308993885,9.97254931435808));
#20279=CARTESIAN_POINT('Ctrl Pts',(-16.3354422641055,17.2301461277349,9.95152575851967));
#20280=CARTESIAN_POINT('Ctrl Pts',(-16.5547757501047,17.1058694878024,9.94049834422647));
#20281=CARTESIAN_POINT('Ctrl Pts',(-16.9348786729487,16.7781774979898,9.91893120590005));
#20282=CARTESIAN_POINT('Ctrl Pts',(-17.0912603497348,16.5772552192783,9.90912402534039));
#20283=CARTESIAN_POINT('Ctrl Pts',(-17.3127769926582,16.1340913484092,9.88973802923938));
#20284=CARTESIAN_POINT('Ctrl Pts',(-17.3788584645816,15.8976206198245,9.87939372790147));
#20285=CARTESIAN_POINT('Ctrl Pts',(-17.4028955886778,15.6034559308058,9.86652563126897));
#20286=CARTESIAN_POINT('Ctrl Pts',(-17.405,15.5516978034419,9.86426149621355));
#20287=CARTESIAN_POINT('Ctrl Pts',(-17.405,15.5,9.862));
#20288=CARTESIAN_POINT('Origin',(-15.5,15.5,-1.713));
#20289=CARTESIAN_POINT('',(-17.405,15.5,9.29949999999995));
#20290=CARTESIAN_POINT('',(-17.405,15.5,9.36199999999999));
#20291=CARTESIAN_POINT('',(-17.405,15.5,-1.713));
#20292=CARTESIAN_POINT('Ctrl Pts',(-17.405,15.5,9.29949999999995));
#20293=CARTESIAN_POINT('Ctrl Pts',(-17.405,15.5820677505046,9.30309001533261));
#20294=CARTESIAN_POINT('Ctrl Pts',(-17.3996969075475,15.6642233508363,9.30668387361483));
#20295=CARTESIAN_POINT('Ctrl Pts',(-17.3577900418683,15.9860939368977,9.32076395174525));
#20296=CARTESIAN_POINT('Ctrl Pts',(-17.2810140392098,16.2181113908634,9.33091344666938));
#20297=CARTESIAN_POINT('Ctrl Pts',(-17.0397143263387,16.6497656912777,9.34979596199811));
#20298=CARTESIAN_POINT('Ctrl Pts',(-16.8740446319471,16.8434043467781,9.36016249414648));
#20299=CARTESIAN_POINT('Ctrl Pts',(-16.4798112952846,17.1525057143526,9.38185832828277));
#20300=CARTESIAN_POINT('Ctrl Pts',(-16.2560680735181,17.2661174912732,9.39281953573834));
#20301=CARTESIAN_POINT('Ctrl Pts',(-15.7845989831092,17.3990107786923,9.41358728959235));
#20302=CARTESIAN_POINT('Ctrl Pts',(-15.5420761225529,17.4197545276094,9.4225832784414));
#20303=CARTESIAN_POINT('Ctrl Pts',(-15.0510290036265,17.3684722711093,9.44230770572467));
#20304=CARTESIAN_POINT('Ctrl Pts',(-14.8076501212771,17.29259475803,9.45318745425482));
#20305=CARTESIAN_POINT('Ctrl Pts',(-14.3705451850896,17.0536228676406,9.4749735401714));
#20306=CARTESIAN_POINT('Ctrl Pts',(-14.1797471571256,16.8951195212724,9.48566853633907));
#20307=CARTESIAN_POINT('Ctrl Pts',(-13.8694408043038,16.5150275804391,9.50573761573171));
#20308=CARTESIAN_POINT('Ctrl Pts',(-13.752598707486,16.297242456207,9.51462500191565));
#20309=CARTESIAN_POINT('Ctrl Pts',(-13.6055288142055,15.8220975418946,9.53540999379283));
#20310=CARTESIAN_POINT('Ctrl Pts',(-13.5795650113124,15.5684707496953,9.54650477910339));
#20311=CARTESIAN_POINT('Ctrl Pts',(-13.6271075672436,15.0753585645942,9.56807574083135));
#20312=CARTESIAN_POINT('Ctrl Pts',(-13.6964698442562,14.840191496141,9.57836301416701));
#20313=CARTESIAN_POINT('Ctrl Pts',(-13.9246409771947,14.3993208139103,9.5976486958044));
#20314=CARTESIAN_POINT('Ctrl Pts',(-14.0848851011449,14.1997178280672,9.60766341357319));
#20315=CARTESIAN_POINT('Ctrl Pts',(-14.4709331777304,13.8775961904101,9.62933394114247));
#20316=CARTESIAN_POINT('Ctrl Pts',(-14.6918497844256,13.7569945647325,9.64034094929446));
#20317=CARTESIAN_POINT('Ctrl Pts',(-15.159737967836,13.6101942820625,9.66127722201094));
#20318=CARTESIAN_POINT('Ctrl Pts',(-15.4013438456414,13.5823472271013,9.67048577767432));
#20319=CARTESIAN_POINT('Ctrl Pts',(-15.8934538493798,13.6190577395498,9.68993175409244));
#20320=CARTESIAN_POINT('Ctrl Pts',(-16.138943260469,13.6876866711395,9.70073291472929));
#20321=CARTESIAN_POINT('Ctrl Pts',(-16.5835358465521,13.9139017605907,9.72252364170252));
#20322=CARTESIAN_POINT('Ctrl Pts',(-16.7794303173594,14.0672309118011,9.7332985395059));
#20323=CARTESIAN_POINT('Ctrl Pts',(-17.1000328628224,14.4378141280377,9.75354970122975));
#20324=CARTESIAN_POINT('Ctrl Pts',(-17.2225779810542,14.6508420595766,9.76235398335849));
#20325=CARTESIAN_POINT('Ctrl Pts',(-17.3701864548766,15.080610356166,9.78115399633266));
#20326=CARTESIAN_POINT('Ctrl Pts',(-17.405,15.2897399857174,9.79030227409083));
#20327=CARTESIAN_POINT('Ctrl Pts',(-17.405,15.5,9.79949999999996));
#20328=CARTESIAN_POINT('Ctrl Pts',(-17.405,15.5,9.862));
#20329=CARTESIAN_POINT('Ctrl Pts',(-17.405,15.2996654395986,9.85323645842513));
#20330=CARTESIAN_POINT('Ctrl Pts',(-17.3733957080017,15.1002367309777,9.84451254291253));
#20331=CARTESIAN_POINT('Ctrl Pts',(-17.2353167025393,14.6769949840126,9.82599803079682));
#20332=CARTESIAN_POINT('Ctrl Pts',(-17.1156525983397,14.4615748866098,9.81716113898337));
#20333=CARTESIAN_POINT('Ctrl Pts',(-16.80025694917,14.0861659210485,9.79700168459996));
#20334=CARTESIAN_POINT('Ctrl Pts',(-16.6069287666911,13.9301940026155,9.78626620443764));
#20335=CARTESIAN_POINT('Ctrl Pts',(-16.1660850038395,13.6974830274193,9.76447541767791));
#20336=CARTESIAN_POINT('Ctrl Pts',(-15.9216377259792,13.6251723453872,9.75363320886213));
#20337=CARTESIAN_POINT('Ctrl Pts',(-15.4300473148473,13.5810767095709,9.73404538724335));
#20338=CARTESIAN_POINT('Ctrl Pts',(-15.1879872214084,13.605317384551,9.72495408202806));
#20339=CARTESIAN_POINT('Ctrl Pts',(-14.7182619044003,13.7450429607215,9.70410295143247));
#20340=CARTESIAN_POINT('Ctrl Pts',(-14.495880438928,13.8620960973241,9.69311806224912));
#20341=CARTESIAN_POINT('Ctrl Pts',(-14.1060014570964,14.177305655609,9.6714535879792));
#20342=CARTESIAN_POINT('Ctrl Pts',(-13.9432207050001,14.3734353392653,9.66128104377678));
#20343=CARTESIAN_POINT('Ctrl Pts',(-13.7082328973408,14.8090298803107,9.64222616446597));
#20344=CARTESIAN_POINT('Ctrl Pts',(-13.6349039528453,15.0425474193521,9.63201104902234));
#20345=CARTESIAN_POINT('Ctrl Pts',(-13.5787039095847,15.5338677316258,9.6105184719325));
#20346=CARTESIAN_POINT('Ctrl Pts',(-13.600024525759,15.7874480067464,9.59942572148978));
#20347=CARTESIAN_POINT('Ctrl Pts',(-13.7384157971629,16.265698939995,9.57850485826805));
#20348=CARTESIAN_POINT('Ctrl Pts',(-13.8518193442911,16.4863923752458,9.56953150176069));
#20349=CARTESIAN_POINT('Ctrl Pts',(-14.1559440668483,16.8721284426117,9.54957315664535));
#20350=CARTESIAN_POINT('Ctrl Pts',(-14.3436419591919,17.0336374285784,9.5389298654822));
#20351=CARTESIAN_POINT('Ctrl Pts',(-14.7761103255414,17.2800944931863,9.51715571308082));
#20352=CARTESIAN_POINT('Ctrl Pts',(-15.0181269721434,17.3602604306989,9.50623377376096));
#20353=CARTESIAN_POINT('Ctrl Pts',(-15.5084664054007,17.4202298003529,9.4863461495044));
#20354=CARTESIAN_POINT('Ctrl Pts',(-15.7515756341446,17.4036993399806,9.47744089150703));
#20355=CARTESIAN_POINT('Ctrl Pts',(-16.2250969623653,17.2789972666476,9.45677455134344));
#20356=CARTESIAN_POINT('Ctrl Pts',(-16.4504036897706,17.169527963874,9.44584471753051));
#20357=CARTESIAN_POINT('Ctrl Pts',(-16.8496765704376,16.867863712006,9.42412063250715));
#20358=CARTESIAN_POINT('Ctrl Pts',(-17.0187935914998,16.6772726628492,9.41354516614536));
#20359=CARTESIAN_POINT('Ctrl Pts',(-17.2675734884154,16.2504214554202,9.39478421625935));
#20360=CARTESIAN_POINT('Ctrl Pts',(-17.3484650463879,16.0202698478367,9.38475896097284));
#20361=CARTESIAN_POINT('Ctrl Pts',(-17.3980615102738,15.6878282291739,9.37021645796922));
#20362=CARTESIAN_POINT('Ctrl Pts',(-17.405,15.5938727688573,9.36610642033496));
#20363=CARTESIAN_POINT('Ctrl Pts',(-17.405,15.5,9.36199999999999));
#20364=CARTESIAN_POINT('Origin',(-15.5,15.5,-1.713));
#20365=CARTESIAN_POINT('',(-17.405,15.5,8.79949999999994));
#20366=CARTESIAN_POINT('',(-17.405,15.5,8.86199999999999));
#20367=CARTESIAN_POINT('',(-17.405,15.5,-1.713));
#20368=CARTESIAN_POINT('Ctrl Pts',(-17.405,15.5,8.79949999999994));
#20369=CARTESIAN_POINT('Ctrl Pts',(-17.405,15.6217129566144,8.80482427631728));
#20370=CARTESIAN_POINT('Ctrl Pts',(-17.3933354276504,15.7434379092509,8.81014907739487));
#20371=CARTESIAN_POINT('Ctrl Pts',(-17.3239854242046,16.100217949099,8.82575625324124));
#20372=CARTESIAN_POINT('Ctrl Pts',(-17.23344403582,16.3260306096801,8.83523091573828));
#20373=CARTESIAN_POINT('Ctrl Pts',(-16.9668880720112,16.7413595851955,8.85441327461609));
#20374=CARTESIAN_POINT('Ctrl Pts',(-16.7897028711993,16.9245620338575,8.86513278946336));
#20375=CARTESIAN_POINT('Ctrl Pts',(-16.3786302955034,17.2082416625364,8.88691052820751));
#20376=CARTESIAN_POINT('Ctrl Pts',(-16.1498761480714,17.3076922537381,8.89775183172885));
#20377=CARTESIAN_POINT('Ctrl Pts',(-15.6715856250916,17.4127003625554,8.91816809584514));
#20378=CARTESIAN_POINT('Ctrl Pts',(-15.4269252595872,17.4189899155349,8.92696236324586));
#20379=CARTESIAN_POINT('Ctrl Pts',(-14.9371123138399,17.337575254231,8.94729909923763));
#20380=CARTESIAN_POINT('Ctrl Pts',(-14.6974339538685,17.2462527758639,8.95837647402575));
#20381=CARTESIAN_POINT('Ctrl Pts',(-14.2762146774355,16.9802149363982,8.98015274321594));
#20382=CARTESIAN_POINT('Ctrl Pts',(-14.0966830482229,16.8112614467855,8.99064949284356));
#20383=CARTESIAN_POINT('Ctrl Pts',(-13.8086030715521,16.4110945374824,9.01031563600935));
#20384=CARTESIAN_POINT('Ctrl Pts',(-13.7042031430122,16.182673235973,9.01963677882861));
#20385=CARTESIAN_POINT('Ctrl Pts',(-13.5886461508703,15.69660922453,9.04089942149891));
#20386=CARTESIAN_POINT('Ctrl Pts',(-13.5793914148363,15.4435361769218,9.05196998351153));
#20387=CARTESIAN_POINT('Ctrl Pts',(-13.6579772676657,14.9574724633382,9.07323261315211));
#20388=CARTESIAN_POINT('Ctrl Pts',(-13.7415377755509,14.728542010486,9.0830895029216));
#20389=CARTESIAN_POINT('Ctrl Pts',(-13.9952354793971,14.3048442117511,9.10196778620158));
#20390=CARTESIAN_POINT('Ctrl Pts',(-14.1666082721507,14.116253615467,9.11258495550098));
#20391=CARTESIAN_POINT('Ctrl Pts',(-14.5692130647157,13.8194985153817,9.13432789198782));
#20392=CARTESIAN_POINT('Ctrl Pts',(-14.7955130433048,13.7127801672651,9.14523518439342));
#20393=CARTESIAN_POINT('Ctrl Pts',(-15.2703703828886,13.5935003764332,9.16583354024071));
#20394=CARTESIAN_POINT('Ctrl Pts',(-15.513886785152,13.5797728775705,9.17469303357404));
#20395=CARTESIAN_POINT('Ctrl Pts',(-16.0059932519448,13.6458404657106,9.19478098176649));
#20396=CARTESIAN_POINT('Ctrl Pts',(-16.2491394450304,13.730053755045,9.20583423744073));
#20397=CARTESIAN_POINT('Ctrl Pts',(-16.6794454210861,13.9841044758504,9.22769256058453));
#20398=CARTESIAN_POINT('Ctrl Pts',(-16.8644125458322,14.1481770209327,9.23828847053363));
#20399=CARTESIAN_POINT('Ctrl Pts',(-17.1631365063348,14.5388054967535,9.25814922190827));
#20400=CARTESIAN_POINT('Ctrl Pts',(-17.2735236272034,14.7620716191431,9.2672196683789));
#20401=CARTESIAN_POINT('Ctrl Pts',(-17.382654501544,15.1634597944469,9.28477820623121));
#20402=CARTESIAN_POINT('Ctrl Pts',(-17.405,15.3315448278493,9.29213100734244));
#20403=CARTESIAN_POINT('Ctrl Pts',(-17.405,15.5,9.29949999999995));
#20404=CARTESIAN_POINT('Ctrl Pts',(-17.405,15.5,9.36199999999999));
#20405=CARTESIAN_POINT('Ctrl Pts',(-17.405,15.3438909532137,9.35517108281774));
#20406=CARTESIAN_POINT('Ctrl Pts',(-17.3858102084349,15.1880105913564,9.34835216935078));
#20407=CARTESIAN_POINT('Ctrl Pts',(-17.2871979074516,14.7954169839361,9.33117834575409));
#20408=CARTESIAN_POINT('Ctrl Pts',(-17.1804249826959,14.5690457460954,9.32196559917841));
#20409=CARTESIAN_POINT('Ctrl Pts',(-16.8881395613673,14.1726311899945,9.30222220993619));
#20410=CARTESIAN_POINT('Ctrl Pts',(-16.7064524674602,14.0055789194889,9.29168538692149));
#20411=CARTESIAN_POINT('Ctrl Pts',(-16.2816164498491,13.7442247021789,9.26987454298673));
#20412=CARTESIAN_POINT('Ctrl Pts',(-16.0405488758122,13.6556861633548,9.25880543045145));
#20413=CARTESIAN_POINT('Ctrl Pts',(-15.5498125385308,13.5803107326153,9.23856580446651));
#20414=CARTESIAN_POINT('Ctrl Pts',(-15.3056131089065,13.5895274997495,9.22975556711626));
#20415=CARTESIAN_POINT('Ctrl Pts',(-14.8286544138276,13.7001309752404,9.20926737445485));
#20416=CARTESIAN_POINT('Ctrl Pts',(-14.6008347040115,13.8024350925033,9.19839905797125));
#20417=CARTESIAN_POINT('Ctrl Pts',(-14.1930293445707,14.0912666711002,9.17663240922349));
#20418=CARTESIAN_POINT('Ctrl Pts',(-14.0181009676516,14.2766023486454,9.16595173306307));
#20419=CARTESIAN_POINT('Ctrl Pts',(-13.7565713314147,14.6952245179651,9.14688776134465));
#20420=CARTESIAN_POINT('Ctrl Pts',(-13.6687599955847,14.9222432269351,9.13727369960923));
#20421=CARTESIAN_POINT('Ctrl Pts',(-13.580930297248,15.4059245590157,9.11611528613239));
#20422=CARTESIAN_POINT('Ctrl Pts',(-13.5851843147722,15.6586224483939,9.10506113524095));
#20423=CARTESIAN_POINT('Ctrl Pts',(-13.691139565932,16.1478117809865,9.08366177685982));
#20424=CARTESIAN_POINT('Ctrl Pts',(-13.7917616714532,16.3795115137555,9.07414444581643));
#20425=CARTESIAN_POINT('Ctrl Pts',(-14.0731868140641,16.785573240168,9.05460148055085));
#20426=CARTESIAN_POINT('Ctrl Pts',(-14.2492888490198,16.9574623633346,9.04417044828869));
#20427=CARTESIAN_POINT('Ctrl Pts',(-14.6647186105415,17.2307703373922,9.0224544940457));
#20428=CARTESIAN_POINT('Ctrl Pts',(-14.9021500355565,17.326430672079,9.01136736311557));
#20429=CARTESIAN_POINT('Ctrl Pts',(-15.3904552885232,17.4173371966627,8.99088013581188));
#20430=CARTESIAN_POINT('Ctrl Pts',(-15.6358674326582,17.4156519875527,8.98208579814301));
#20431=CARTESIAN_POINT('Ctrl Pts',(-16.1162026684393,17.3193851476517,8.96178326373925));
#20432=CARTESIAN_POINT('Ctrl Pts',(-16.346344706898,17.2244006751455,8.95098706566238));
#20433=CARTESIAN_POINT('Ctrl Pts',(-16.7623834649252,16.9488308762145,8.92919856903612));
#20434=CARTESIAN_POINT('Ctrl Pts',(-16.9430358563345,16.76901250103,8.91842172092558));
#20435=CARTESIAN_POINT('Ctrl Pts',(-17.2174051014579,16.3588603424316,8.89905659338433));
#20436=CARTESIAN_POINT('Ctrl Pts',(-17.3121965174972,16.1348911979066,8.8897730182812));
#20437=CARTESIAN_POINT('Ctrl Pts',(-17.3908915635191,15.7676602614367,8.87370867285382));
#20438=CARTESIAN_POINT('Ctrl Pts',(-17.405,15.6338562764287,8.86785548015872));
#20439=CARTESIAN_POINT('Ctrl Pts',(-17.405,15.5,8.86199999999999));
#20440=CARTESIAN_POINT('Origin',(-15.5,15.5,-1.713));
#20441=CARTESIAN_POINT('',(-17.405,15.5,8.29949999999994));
#20442=CARTESIAN_POINT('',(-17.405,15.5,8.36199999999998));
#20443=CARTESIAN_POINT('',(-17.405,15.5,-1.713));
#20444=CARTESIAN_POINT('Ctrl Pts',(-17.405,15.5,8.29949999999994));
#20445=CARTESIAN_POINT('Ctrl Pts',(-17.405,15.659889295304,8.30649428238419));
#20446=CARTESIAN_POINT('Ctrl Pts',(-17.3848694669146,15.8194993551224,8.31347634974275));
#20447=CARTESIAN_POINT('Ctrl Pts',(-17.2846557073979,16.2087039329203,8.3305019218249));
#20448=CARTESIAN_POINT('Ctrl Pts',(-17.1806408331997,16.4288130372242,8.33947939030711));
#20449=CARTESIAN_POINT('Ctrl Pts',(-16.8893971352298,16.8275317385818,8.35923371190873));
#20450=CARTESIAN_POINT('Ctrl Pts',(-16.7014386929281,16.9997636421122,8.37012140821907));
#20451=CARTESIAN_POINT('Ctrl Pts',(-16.2751610984012,17.2574129066877,8.39190582896325));
#20452=CARTESIAN_POINT('Ctrl Pts',(-16.0422967724175,17.3426348398669,8.40259162898628));
#20453=CARTESIAN_POINT('Ctrl Pts',(-15.557644496301,17.4198338786248,8.42264065359248));
#20454=CARTESIAN_POINT('Ctrl Pts',(-15.3104726891065,17.4113260431361,8.4315416642333));
#20455=CARTESIAN_POINT('Ctrl Pts',(-14.8257444026703,17.2994734054767,8.45235152113692));
#20456=CARTESIAN_POINT('Ctrl Pts',(-14.5935391277617,17.1944158351004,8.46344620408319));
#20457=CARTESIAN_POINT('Ctrl Pts',(-14.1913224566373,16.9054796646701,8.48500341931656));
#20458=CARTESIAN_POINT('Ctrl Pts',(-14.0229593781544,16.7273479814129,8.49527780884648));
#20459=CARTESIAN_POINT('Ctrl Pts',(-13.7564200897581,16.3082895945115,8.51454110667273));
#20460=CARTESIAN_POINT('Ctrl Pts',(-13.6643670389324,16.0691129066074,8.52460442228296));
#20461=CARTESIAN_POINT('Ctrl Pts',(-13.5801640706732,15.5732067014332,8.54629760711124));
#20462=CARTESIAN_POINT('Ctrl Pts',(-13.5870598138748,15.321698471096,8.55729971692476));
#20463=CARTESIAN_POINT('Ctrl Pts',(-13.6955023283534,14.8435430018443,8.57821640411864));
#20464=CARTESIAN_POINT('Ctrl Pts',(-13.7929618289516,14.620710097899,8.58739617365219));
#20465=CARTESIAN_POINT('Ctrl Pts',(-14.0722259123273,14.2138380182375,8.60687499387961));
#20466=CARTESIAN_POINT('Ctrl Pts',(-14.2550239314294,14.0361814582294,8.61768584288696));
#20467=CARTESIAN_POINT('Ctrl Pts',(-14.6741023301257,13.7657537432244,8.63947702385593));
#20468=CARTESIAN_POINT('Ctrl Pts',(-14.9050731475777,13.6735852101748,8.6502430283166));
#20469=CARTESIAN_POINT('Ctrl Pts',(-15.386674416427,13.5828221715784,8.67047314435406));
#20470=CARTESIAN_POINT('Ctrl Pts',(-15.6325779853084,13.58405715791,8.67928322319381));
#20471=CARTESIAN_POINT('Ctrl Pts',(-16.1198923784801,13.6809759238713,8.69986441423044));
#20472=CARTESIAN_POINT('Ctrl Pts',(-16.3558610117794,13.779358970167,8.71095568081319));
#20473=CARTESIAN_POINT('Ctrl Pts',(-16.7675587024543,14.0572124059979,8.73262966929611));
#20474=CARTESIAN_POINT('Ctrl Pts',(-16.9414628364907,14.2309270106159,8.74301736396836));
#20475=CARTESIAN_POINT('Ctrl Pts',(-17.2186438231263,14.6407208278419,8.76248117343841));
#20476=CARTESIAN_POINT('Ctrl Pts',(-17.3168405279419,14.8745326909115,8.77213922532401));
#20477=CARTESIAN_POINT('Ctrl Pts',(-17.392281680729,15.2458303944107,8.78838146957158));
#20478=CARTESIAN_POINT('Ctrl Pts',(-17.405,15.3729086573887,8.79394044870461));
#20479=CARTESIAN_POINT('Ctrl Pts',(-17.405,15.5,8.79949999999994));
#20480=CARTESIAN_POINT('Ctrl Pts',(-17.405,15.5,8.86199999999999));
#20481=CARTESIAN_POINT('Ctrl Pts',(-17.405,15.3855229224658,8.85699225382614));
#20482=CARTESIAN_POINT('Ctrl Pts',(-17.3946811986137,15.2710075985785,8.85198283458356));
#20483=CARTESIAN_POINT('Ctrl Pts',(-17.3286272675359,14.9092076691282,8.83615606601617));
#20484=CARTESIAN_POINT('Ctrl Pts',(-17.2342052023006,14.6721012428112,8.82625705957892));
#20485=CARTESIAN_POINT('Ctrl Pts',(-16.9635816997827,14.2565828049718,8.80691646259897));
#20486=CARTESIAN_POINT('Ctrl Pts',(-16.7930874537182,14.0801193134113,8.79659782331327));
#20487=CARTESIAN_POINT('Ctrl Pts',(-16.3872122755908,13.7953832855463,8.77499387628981));
#20488=CARTESIAN_POINT('Ctrl Pts',(-16.153547037711,13.6928614102057,8.76389934568372));
#20489=CARTESIAN_POINT('Ctrl Pts',(-15.6678085401293,13.5867163450376,8.74317605560998));
#20490=CARTESIAN_POINT('Ctrl Pts',(-15.421129930203,13.5809919918463,8.7343184829412));
#20491=CARTESIAN_POINT('Ctrl Pts',(-14.9376278753187,13.6633575294034,8.71420003013759));
#20492=CARTESIAN_POINT('Ctrl Pts',(-14.7054597718186,13.7512259923533,8.70348272011769));
#20493=CARTESIAN_POINT('Ctrl Pts',(-14.2818750115858,14.0137591886409,8.68169349172043));
#20494=CARTESIAN_POINT('Ctrl Pts',(-14.0958604448596,14.188073077006,8.67083389922518));
#20495=CARTESIAN_POINT('Ctrl Pts',(-13.8091654649599,14.5899091772312,8.65118371611744));
#20496=CARTESIAN_POINT('Ctrl Pts',(-13.7076445856252,14.8110433198424,8.642138087496));
#20497=CARTESIAN_POINT('Ctrl Pts',(-13.5906893278651,15.286833932135,8.62132484986291));
#20498=CARTESIAN_POINT('Ctrl Pts',(-13.5791977767196,15.5377080032355,8.61035048104836));
#20499=CARTESIAN_POINT('Ctrl Pts',(-13.6538319112419,16.0332982624169,8.58867111712966));
#20500=CARTESIAN_POINT('Ctrl Pts',(-13.7406537883804,16.2729150218738,8.57841211733937));
#20501=CARTESIAN_POINT('Ctrl Pts',(-13.9974050276377,16.6958252070472,8.55943538119602));
#20502=CARTESIAN_POINT('Ctrl Pts',(-14.1615973637091,16.8771145995509,8.54924992929767));
#20503=CARTESIAN_POINT('Ctrl Pts',(-14.5566124809955,17.1740528601567,8.52779051299181));
#20504=CARTESIAN_POINT('Ctrl Pts',(-14.7859169215418,17.2839633295296,8.51669958099706));
#20505=CARTESIAN_POINT('Ctrl Pts',(-15.2686105331722,17.4068648278051,8.49572514184335));
#20506=CARTESIAN_POINT('Ctrl Pts',(-15.516764690117,17.4207780307135,8.4867099898438));
#20507=CARTESIAN_POINT('Ctrl Pts',(-16.0035896898075,17.3535209067153,8.46679610625113));
#20508=CARTESIAN_POINT('Ctrl Pts',(-16.2377072623264,17.2733907321687,8.45617419669088));
#20509=CARTESIAN_POINT('Ctrl Pts',(-16.6711781378121,17.0239343677871,8.43429646387539));
#20510=CARTESIAN_POINT('Ctrl Pts',(-16.8644167285607,16.8536687488138,8.42325174217519));
#20511=CARTESIAN_POINT('Ctrl Pts',(-17.1642937602988,16.4578660758281,8.40323413657636));
#20512=CARTESIAN_POINT('Ctrl Pts',(-17.272221033532,16.2393379204675,8.39434199127156));
#20513=CARTESIAN_POINT('Ctrl Pts',(-17.3820334094121,15.8411433720287,8.37692315713163));
#20514=CARTESIAN_POINT('Ctrl Pts',(-17.405,15.6707800180835,8.36947069195464));
#20515=CARTESIAN_POINT('Ctrl Pts',(-17.405,15.5,8.36199999999998));
#20516=CARTESIAN_POINT('Origin',(-15.5,15.5,-1.713));
#20517=CARTESIAN_POINT('',(-17.405,15.5,7.79949999999993));
#20518=CARTESIAN_POINT('',(-17.405,15.5,7.86199999999997));
#20519=CARTESIAN_POINT('',(-17.405,15.5,-1.713));
#20520=CARTESIAN_POINT('Ctrl Pts',(-17.405,15.5,7.79949999999993));
#20521=CARTESIAN_POINT('Ctrl Pts',(-17.405,15.6975196488277,7.80814040458557));
#20522=CARTESIAN_POINT('Ctrl Pts',(-17.3742778394761,15.8941571127754,7.81674221840651));
#20523=CARTESIAN_POINT('Ctrl Pts',(-17.2394266701263,16.3138268615082,7.83510047513149));
#20524=CARTESIAN_POINT('Ctrl Pts',(-17.1217319567968,16.5285441088021,7.84389243139474));
#20525=CARTESIAN_POINT('Ctrl Pts',(-16.8049244234265,16.9109041573485,7.86425740935985));
#20526=CARTESIAN_POINT('Ctrl Pts',(-16.605500990129,17.0720470183816,7.87533690147979));
#20527=CARTESIAN_POINT('Ctrl Pts',(-16.1638497969511,17.3022071724644,7.89710248459199));
#20528=CARTESIAN_POINT('Ctrl Pts',(-15.9276056025431,17.3723832941734,7.90758724114091));
#20529=CARTESIAN_POINT('Ctrl Pts',(-15.436677343757,17.4201648145539,7.92723059650988));
#20530=CARTESIAN_POINT('Ctrl Pts',(-15.1864838895139,17.3954586412815,7.9365858965675));
#20531=CARTESIAN_POINT('Ctrl Pts',(-14.7081429702316,17.2506698475039,7.95787416361287));
#20532=CARTESIAN_POINT('Ctrl Pts',(-14.4848664556224,17.1313747146956,7.96894199826398));
#20533=CARTESIAN_POINT('Ctrl Pts',(-14.1044542813343,16.8190167941685,7.99018546139198));
#20534=CARTESIAN_POINT('Ctrl Pts',(-13.9486774532445,16.6316831386892,7.9999950508009));
#20535=CARTESIAN_POINT('Ctrl Pts',(-13.710127524274,16.1993372753248,8.01890781822715));
#20536=CARTESIAN_POINT('Ctrl Pts',(-13.6333368077763,15.9563538337873,8.0295370151448));
#20537=CARTESIAN_POINT('Ctrl Pts',(-13.5793899361072,15.4591965407512,8.05128492822599));
#20538=CARTESIAN_POINT('Ctrl Pts',(-13.6009677390036,15.2100142466142,8.06218529104914));
#20539=CARTESIAN_POINT('Ctrl Pts',(-13.7366804393283,14.7395980072616,8.08276342925354));
#20540=CARTESIAN_POINT('Ctrl Pts',(-13.8473311902744,14.5221514404535,8.09161159696003));
#20541=CARTESIAN_POINT('Ctrl Pts',(-14.1519610237373,14.1300797586998,8.1117276518772));
#20542=CARTESIAN_POINT('Ctrl Pts',(-14.3469687875577,13.9623417964605,8.12278411113019));
#20543=CARTESIAN_POINT('Ctrl Pts',(-14.7828085084972,13.7182512489598,8.144634222419));
#20544=CARTESIAN_POINT('Ctrl Pts',(-15.0175620224701,13.6408974478214,8.15521949832876));
#20545=CARTESIAN_POINT('Ctrl Pts',(-15.5055502329557,13.5790652088895,8.17505879432587));
#20546=CARTESIAN_POINT('Ctrl Pts',(-15.7542579090358,13.5959566304196,8.18415319875526));
#20547=CARTESIAN_POINT('Ctrl Pts',(-16.2357891521937,13.7249229177914,8.20521625356614));
#20548=CARTESIAN_POINT('Ctrl Pts',(-16.4634602409219,13.8374648979382,8.21630286496682));
#20549=CARTESIAN_POINT('Ctrl Pts',(-16.8544572608822,14.1387217742593,8.23770451808363));
#20550=CARTESIAN_POINT('Ctrl Pts',(-17.0163359296066,14.3217036695108,8.24783933816551));
#20551=CARTESIAN_POINT('Ctrl Pts',(-17.2680640740017,14.7472552555663,8.2666835534289));
#20552=CARTESIAN_POINT('Ctrl Pts',(-17.3521336084914,14.9878171755692,8.27709480208075));
#20553=CARTESIAN_POINT('Ctrl Pts',(-17.3989688038528,15.3248756230826,8.29183926610146));
#20554=CARTESIAN_POINT('Ctrl Pts',(-17.405,15.4124796446347,8.29567146301983));
#20555=CARTESIAN_POINT('Ctrl Pts',(-17.405,15.5,8.29949999999994));
#20556=CARTESIAN_POINT('Ctrl Pts',(-17.405,15.5,8.36199999999998));
#20557=CARTESIAN_POINT('Ctrl Pts',(-17.405,15.4237223563989,8.35866327018366));
#20558=CARTESIAN_POINT('Ctrl Pts',(-17.4004188007143,15.3473615926038,8.35532290431339));
#20559=CARTESIAN_POINT('Ctrl Pts',(-17.3609408206951,15.020855136578,8.34104003222127));
#20560=CARTESIAN_POINT('Ctrl Pts',(-17.2811919732465,14.7788464883823,8.33045347718208));
#20561=CARTESIAN_POINT('Ctrl Pts',(-17.0372789993401,14.3492654021155,8.31166165363585));
#20562=CARTESIAN_POINT('Ctrl Pts',(-16.8790373404125,14.1636894364016,8.30168180611397));
#20563=CARTESIAN_POINT('Ctrl Pts',(-16.4942877349889,13.8557881049619,8.28037149998481));
#20564=CARTESIAN_POINT('Ctrl Pts',(-16.2692048955806,13.739213606314,8.26929474118309));
#20565=CARTESIAN_POINT('Ctrl Pts',(-15.7895412841264,13.6008458658965,8.24809680841848));
#20566=CARTESIAN_POINT('Ctrl Pts',(-15.5399575414503,13.5793194731614,8.23885671519635));
#20567=CARTESIAN_POINT('Ctrl Pts',(-15.0502061650656,13.6327856423769,8.21913360854301));
#20568=CARTESIAN_POINT('Ctrl Pts',(-14.8145379663992,13.7058628640712,8.20860721931481));
#20569=CARTESIAN_POINT('Ctrl Pts',(-14.3751816447576,13.9416635369909,8.18680520390296));
#20570=CARTESIAN_POINT('Ctrl Pts',(-14.1775156357315,14.1054824757792,8.17573375794165));
#20571=CARTESIAN_POINT('Ctrl Pts',(-13.8656118399955,14.4917801955565,8.15546842677224));
#20572=CARTESIAN_POINT('Ctrl Pts',(-13.7507656728511,14.7075897292398,8.14666361639372));
#20573=CARTESIAN_POINT('Ctrl Pts',(-13.6066151074591,15.175517044435,8.12619435501161));
#20574=CARTESIAN_POINT('Ctrl Pts',(-13.5805257646738,15.4238069094281,8.11533303108365));
#20575=CARTESIAN_POINT('Ctrl Pts',(-13.6251480140868,15.921466768242,8.09356313349774));
#20576=CARTESIAN_POINT('Ctrl Pts',(-13.6974040568621,16.1658652264558,8.0828720373379));
#20577=CARTESIAN_POINT('Ctrl Pts',(-13.9277599983122,16.6023848199964,8.06377669203865));
#20578=CARTESIAN_POINT('Ctrl Pts',(-14.0798197501874,16.7924059014821,8.05420075343611));
#20579=CARTESIAN_POINT('Ctrl Pts',(-14.4536516307035,17.1114565550985,8.0330601921028));
#20580=CARTESIAN_POINT('Ctrl Pts',(-14.6741360716317,17.2348161556276,8.02200923290562));
#20581=CARTESIAN_POINT('Ctrl Pts',(-15.1504002019035,17.3893230647177,8.00058708547467));
#20582=CARTESIAN_POINT('Ctrl Pts',(-15.4015317171629,17.4188661114753,7.99103364348828));
#20583=CARTESIAN_POINT('Ctrl Pts',(-15.8941999682968,17.379645034335,7.97151160675642));
#20584=CARTESIAN_POINT('Ctrl Pts',(-16.1312424873964,17.3138280762805,7.96109195136076));
#20585=CARTESIAN_POINT('Ctrl Pts',(-16.5762050805964,17.0921688775659,7.93938685473773));
#20586=CARTESIAN_POINT('Ctrl Pts',(-16.7782000529196,16.9350735395531,7.92829847125238));
#20587=CARTESIAN_POINT('Ctrl Pts',(-17.1023321254605,16.5586656791824,7.90778619919696));
#20588=CARTESIAN_POINT('Ctrl Pts',(-17.2243146842095,16.3455651446033,7.89898885146997));
#20589=CARTESIAN_POINT('Ctrl Pts',(-17.370589418067,15.91693477667,7.88023861665224));
#20590=CARTESIAN_POINT('Ctrl Pts',(-17.405,15.7090406870887,7.87114438701173));
#20591=CARTESIAN_POINT('Ctrl Pts',(-17.405,15.5,7.86199999999997));
#20592=CARTESIAN_POINT('Origin',(-15.5,15.5,-1.713));
#20593=CARTESIAN_POINT('',(-17.405,15.5,7.29949999999993));
#20594=CARTESIAN_POINT('',(-17.405,15.5,7.36199999999997));
#20595=CARTESIAN_POINT('',(-17.405,15.5,-1.713));
#20596=CARTESIAN_POINT('Ctrl Pts',(-17.405,15.5,7.29949999999993));
#20597=CARTESIAN_POINT('Ctrl Pts',(-17.405,15.7346844862759,7.30976616300412));
#20598=CARTESIAN_POINT('Ctrl Pts',(-17.3616308313112,15.9674729947138,7.3199493873452));
#20599=CARTESIAN_POINT('Ctrl Pts',(-17.188586342212,16.4153375533469,7.33954101283222));
#20600=CARTESIAN_POINT('Ctrl Pts',(-17.0568707339665,16.624865920156,7.34845640218951));
#20601=CARTESIAN_POINT('Ctrl Pts',(-16.7163727742873,16.9876559067647,7.36929082372597));
#20602=CARTESIAN_POINT('Ctrl Pts',(-16.5088738801906,17.1354961938847,7.38038528816625));
#20603=CARTESIAN_POINT('Ctrl Pts',(-16.0570334202494,17.3378486587404,7.40192866302165));
#20604=CARTESIAN_POINT('Ctrl Pts',(-15.8184823713025,17.3938228957298,7.41219018476189));
#20605=CARTESIAN_POINT('Ctrl Pts',(-15.3220069380349,17.4136024760751,7.43143122272065));
#20606=CARTESIAN_POINT('Ctrl Pts',(-15.0686719423133,17.3728450906666,7.44154367935196));
#20607=CARTESIAN_POINT('Ctrl Pts',(-14.5975242118065,17.1960611997515,7.46325924580043));
#20608=CARTESIAN_POINT('Ctrl Pts',(-14.383695789403,17.0636347797371,7.47425636110489));
#20609=CARTESIAN_POINT('Ctrl Pts',(-14.0250181273177,16.7294640161342,7.49515353297442));
#20610=CARTESIAN_POINT('Ctrl Pts',(-13.8814342167352,16.5331416030756,7.50430570415231));
#20611=CARTESIAN_POINT('Ctrl Pts',(-13.6702310630037,16.0871105921573,7.52381712195276));
#20612=CARTESIAN_POINT('Ctrl Pts',(-13.6086255963041,15.8397572562305,7.53463747785507));
#20613=CARTESIAN_POINT('Ctrl Pts',(-13.5856885629066,15.3416065223655,7.55642884854033));
#20614=CARTESIAN_POINT('Ctrl Pts',(-13.6221738802065,15.0957006058977,7.56718588775589));
#20615=CARTESIAN_POINT('Ctrl Pts',(-13.785927657894,14.633720204913,7.58739500415943));
#20616=CARTESIAN_POINT('Ctrl Pts',(-13.9107533017096,14.4216771100387,7.59621187363859));
#20617=CARTESIAN_POINT('Ctrl Pts',(-14.239705269712,14.0492323911653,7.6168200591308));
#20618=CARTESIAN_POINT('Ctrl Pts',(-14.4433563780086,13.8948325603828,7.62791222661482));
#20619=CARTESIAN_POINT('Ctrl Pts',(-14.8904201844231,13.6788149766268,7.64957353043571));
#20620=CARTESIAN_POINT('Ctrl Pts',(-15.127946838379,13.615882339785,7.65994844009548));
#20621=CARTESIAN_POINT('Ctrl Pts',(-15.6217480265965,13.5823404443143,7.6793891803033));
#20622=CARTESIAN_POINT('Ctrl Pts',(-15.8735137276434,13.6151256989545,7.68909034235678));
#20623=CARTESIAN_POINT('Ctrl Pts',(-16.3483419251982,13.7761111850588,7.71059979225039));
#20624=CARTESIAN_POINT('Ctrl Pts',(-16.5669268548491,13.902144028833,7.72163726048528));
#20625=CARTESIAN_POINT('Ctrl Pts',(-16.9363616526307,14.2256227819054,7.74270809585085));
#20626=CARTESIAN_POINT('Ctrl Pts',(-17.0859510511762,14.417455145383,7.75214458203764));
#20627=CARTESIAN_POINT('Ctrl Pts',(-17.3107912676849,14.8567493754688,7.77136130251383));
#20628=CARTESIAN_POINT('Ctrl Pts',(-17.3799862553193,15.1020495253587,7.78209184275398));
#20629=CARTESIAN_POINT('Ctrl Pts',(-17.4031280242506,15.4024279056926,7.79523175440463));
#20630=CARTESIAN_POINT('Ctrl Pts',(-17.405,15.4512408323701,7.79736705303449));
#20631=CARTESIAN_POINT('Ctrl Pts',(-17.405,15.5,7.79949999999993));
#20632=CARTESIAN_POINT('Ctrl Pts',(-17.405,15.5,7.86199999999997));
#20633=CARTESIAN_POINT('Ctrl Pts',(-17.405,15.4630602155995,7.86038408642165));
#20634=CARTESIAN_POINT('Ctrl Pts',(-17.4039255679755,15.4260846266625,7.85876660659067));
#20635=CARTESIAN_POINT('Ctrl Pts',(-17.387080139803,15.1371592208085,7.84612769994789));
#20636=CARTESIAN_POINT('Ctrl Pts',(-17.3224616755698,14.8905901473679,7.83534165124095));
#20637=CARTESIAN_POINT('Ctrl Pts',(-17.105849975258,14.4472097491717,7.81594618325336));
#20638=CARTESIAN_POINT('Ctrl Pts',(-16.9599010103547,14.2526704430696,7.80669145159722));
#20639=CARTESIAN_POINT('Ctrl Pts',(-16.5969765988213,13.9226974163492,7.78572521041605));
#20640=CARTESIAN_POINT('Ctrl Pts',(-16.3812522583051,13.7927700947983,7.77471093133132));
#20641=CARTESIAN_POINT('Ctrl Pts',(-15.9086227031579,13.6222144824737,7.75307545418788));
#20642=CARTESIAN_POINT('Ctrl Pts',(-15.6559096497849,13.5846116642005,7.74313367827248));
#20643=CARTESIAN_POINT('Ctrl Pts',(-15.1604736749438,13.6098026607374,7.72381365909359));
#20644=CARTESIAN_POINT('Ctrl Pts',(-14.9223004500424,13.6685072296533,7.71350673224652));
#20645=CARTESIAN_POINT('Ctrl Pts',(-14.4722850980472,13.8762308132931,7.69191502101551));
#20646=CARTESIAN_POINT('Ctrl Pts',(-14.266271196293,14.0266544528219,7.68082031006991));
#20647=CARTESIAN_POINT('Ctrl Pts',(-13.93029022398,14.3932495833448,7.66007378240269));
#20648=CARTESIAN_POINT('Ctrl Pts',(-13.8012842680293,14.6037589371102,7.65120564579572));
#20649=CARTESIAN_POINT('Ctrl Pts',(-13.629511599771,15.0632431785232,7.63110572272428));
#20650=CARTESIAN_POINT('Ctrl Pts',(-13.5888157191007,15.3080507039922,7.62039673210884));
#20651=CARTESIAN_POINT('Ctrl Pts',(-13.6028899025254,15.8061291795299,7.59860852233028));
#20652=CARTESIAN_POINT('Ctrl Pts',(-13.6601003824371,16.0545546479973,7.58774126649181));
#20653=CARTESIAN_POINT('Ctrl Pts',(-13.8634221218517,16.5043972734192,7.56806311139898));
#20654=CARTESIAN_POINT('Ctrl Pts',(-14.0035966438283,16.7033244873628,7.55903679252281));
#20655=CARTESIAN_POINT('Ctrl Pts',(-14.3561323851029,17.0435145939322,7.53824064374894));
#20656=CARTESIAN_POINT('Ctrl Pts',(-14.5671785530695,17.1794970602246,7.52727115223642));
#20657=CARTESIAN_POINT('Ctrl Pts',(-15.0330507577244,17.3640542656091,7.50558542315329));
#20658=CARTESIAN_POINT('Ctrl Pts',(-15.2838292559505,17.4094400025414,7.49528649856399));
#20659=CARTESIAN_POINT('Ctrl Pts',(-15.7784019892638,17.4000648055593,7.47634510969437));
#20660=CARTESIAN_POINT('Ctrl Pts',(-16.0175856000629,17.3492797400771,7.46617312299874));
#20661=CARTESIAN_POINT('Ctrl Pts',(-16.4727205920939,17.1571681024677,7.44472892859563));
#20662=CARTESIAN_POINT('Ctrl Pts',(-16.6829539636631,17.0142714125952,7.43363899922387));
#20663=CARTESIAN_POINT('Ctrl Pts',(-17.0319919929381,16.6587785935647,7.41264065234048));
#20664=CARTESIAN_POINT('Ctrl Pts',(-17.1688836487448,16.451098825887,7.40360537296093));
#20665=CARTESIAN_POINT('Ctrl Pts',(-17.3554698481453,15.9963244729221,7.38371148175513));
#20666=CARTESIAN_POINT('Ctrl Pts',(-17.4038675341353,15.7537299678413,7.37309929868073));
#20667=CARTESIAN_POINT('Ctrl Pts',(-17.4049934554365,15.5057662871049,7.3622522435304));
#20668=CARTESIAN_POINT('Ctrl Pts',(-17.405,15.5028829839971,7.36212611478549));
#20669=CARTESIAN_POINT('Ctrl Pts',(-17.405,15.5,7.36199999999997));
#20670=CARTESIAN_POINT('Origin',(-15.5,15.5,-1.713));
#20671=CARTESIAN_POINT('',(-17.405,15.5,6.79949999999992));
#20672=CARTESIAN_POINT('',(-17.405,15.5,6.86199999999996));
#20673=CARTESIAN_POINT('',(-17.405,15.5,-1.713));
#20674=CARTESIAN_POINT('Ctrl Pts',(-17.405,15.5,6.79949999999992));
#20675=CARTESIAN_POINT('Ctrl Pts',(-17.405,15.529549846541,6.80079264420556));
#20676=CARTESIAN_POINT('Ctrl Pts',(-17.4043124534958,15.5591255898548,6.80208642125338));
#20677=CARTESIAN_POINT('Ctrl Pts',(-17.3915676693565,15.8325360994437,6.81404663602105));
#20678=CARTESIAN_POINT('Ctrl Pts',(-17.333440693878,16.0719462026126,6.82451951892433));
#20679=CARTESIAN_POINT('Ctrl Pts',(-17.1278167083024,16.520480786797,6.84414045436547));
#20680=CARTESIAN_POINT('Ctrl Pts',(-16.980463496419,16.724504038407,6.85353031591982));
#20681=CARTESIAN_POINT('Ctrl Pts',(-16.6145319788221,17.0651375512721,6.87484364692231));
#20682=CARTESIAN_POINT('Ctrl Pts',(-16.3991807744398,17.1980307541944,6.88590866071021));
#20683=CARTESIAN_POINT('Ctrl Pts',(-15.9379957669685,17.3696215386,6.90713321558848));
#20684=CARTESIAN_POINT('Ctrl Pts',(-15.6977875712375,17.4100163428367,6.91689732140571));
#20685=CARTESIAN_POINT('Ctrl Pts',(-15.2041750736869,17.3987380335797,6.93584395820067));
#20686=CARTESIAN_POINT('Ctrl Pts',(-14.9555355034449,17.3428921189607,6.94648486552899));
#20687=CARTESIAN_POINT('Ctrl Pts',(-14.4987799696637,17.1394893913568,6.96823741405812));
#20688=CARTESIAN_POINT('Ctrl Pts',(-14.294325396585,16.9955679076125,6.97913083470897));
#20689=CARTESIAN_POINT('Ctrl Pts',(-13.9559636865064,16.6417078228246,6.9996890096429));
#20690=CARTESIAN_POINT('Ctrl Pts',(-13.8236226580918,16.436642552474,7.0085270099529));
#20691=CARTESIAN_POINT('Ctrl Pts',(-13.6379799213828,15.9761578395865,7.0286706981807));
#20692=CARTESIAN_POINT('Ctrl Pts',(-13.5910870227694,15.7233378417343,7.03973019065018));
#20693=CARTESIAN_POINT('Ctrl Pts',(-13.5992639609071,15.224034742332,7.06157197102649));
#20694=CARTESIAN_POINT('Ctrl Pts',(-13.6504175832456,14.9822974973374,7.07214665365967));
#20695=CARTESIAN_POINT('Ctrl Pts',(-13.8423565232607,14.52925632131,7.09196472785161));
#20696=CARTESIAN_POINT('Ctrl Pts',(-13.9821516037496,14.3226007751505,7.10108374200246));
#20697=CARTESIAN_POINT('Ctrl Pts',(-14.3359280564568,13.971217198846,7.12217172028144));
#20698=CARTESIAN_POINT('Ctrl Pts',(-14.5476365321871,13.8310965413759,7.13325681419718));
#20699=CARTESIAN_POINT('Ctrl Pts',(-15.0045099354585,13.6447143929865,7.15464154944394));
#20700=CARTESIAN_POINT('Ctrl Pts',(-15.2439977845298,13.5968231411538,7.16476176760272));
#20701=CARTESIAN_POINT('Ctrl Pts',(-15.7383251588478,13.5932041716068,7.18356795958517));
#20702=CARTESIAN_POINT('Ctrl Pts',(-15.988528809768,13.6414881810142,7.19402416667735));
#20703=CARTESIAN_POINT('Ctrl Pts',(-16.4519492153176,13.8313119381252,7.21573220352747));
#20704=CARTESIAN_POINT('Ctrl Pts',(-16.6611974772414,13.9695253264105,7.22668237870974));
#20705=CARTESIAN_POINT('Ctrl Pts',(-17.0098172624393,14.3135223328633,7.2474134414162));
#20706=CARTESIAN_POINT('Ctrl Pts',(-17.1478236533182,14.5141271475301,7.25637345352264));
#20707=CARTESIAN_POINT('Ctrl Pts',(-17.3460828933711,14.9663857636705,7.2761572949986));
#20708=CARTESIAN_POINT('Ctrl Pts',(-17.4004688935963,15.2154557242057,7.28705274384091));
#20709=CARTESIAN_POINT('Ctrl Pts',(-17.4049096459225,15.4785717763734,7.29856263238718));
#20710=CARTESIAN_POINT('Ctrl Pts',(-17.405,15.4892878632759,7.29903140259292));
#20711=CARTESIAN_POINT('Ctrl Pts',(-17.405,15.5,7.29949999999993));
#20712=CARTESIAN_POINT('Ctrl Pts',(-17.405,15.5,7.36199999999997));
#20713=CARTESIAN_POINT('Ctrl Pts',(-17.405,15.2480559696299,7.35097882631798));
#20714=CARTESIAN_POINT('Ctrl Pts',(-17.3550184248228,14.9985489919044,7.34006426036327));
#20715=CARTESIAN_POINT('Ctrl Pts',(-17.1648009926083,14.5429999576051,7.32013648108508));
#20716=CARTESIAN_POINT('Ctrl Pts',(-17.0301331039721,14.3397800127035,7.31125739919347));
#20717=CARTESIAN_POINT('Ctrl Pts',(-16.6875547606706,13.9899554238771,7.29062774729064));
#20718=CARTESIAN_POINT('Ctrl Pts',(-16.481115413662,13.8483563120135,7.27970993124595));
#20719=CARTESIAN_POINT('Ctrl Pts',(-16.0216210024307,13.6505150043546,7.25797526427951));
#20720=CARTESIAN_POINT('Ctrl Pts',(-15.7723283761313,13.5977521369995,7.2473770498863));
#20721=CARTESIAN_POINT('Ctrl Pts',(-15.2784189513864,13.5925705913544,7.2285525143736));
#20722=CARTESIAN_POINT('Ctrl Pts',(-15.0385078305141,13.6360094360532,7.21861991861553));
#20723=CARTESIAN_POINT('Ctrl Pts',(-14.5790228459424,13.8136434960377,7.19732758706308));
#20724=CARTESIAN_POINT('Ctrl Pts',(-14.3651283543253,13.9494945162497,7.18625306503437));
#20725=CARTESIAN_POINT('Ctrl Pts',(-14.004140425649,14.2945374747623,7.16503057177324));
#20726=CARTESIAN_POINT('Ctrl Pts',(-13.8598809196958,14.4996329878048,7.15576058671019));
#20727=CARTESIAN_POINT('Ctrl Pts',(-13.6598155630892,14.9500111762076,7.13605900366546));
#20728=CARTESIAN_POINT('Ctrl Pts',(-13.6045079682599,15.190389739209,7.12554375594011));
#20729=CARTESIAN_POINT('Ctrl Pts',(-13.5874029842169,15.6885651694387,7.10375130492394));
#20730=CARTESIAN_POINT('Ctrl Pts',(-13.62957506411,15.9417120961294,7.09267751110545));
#20731=CARTESIAN_POINT('Ctrl Pts',(-13.8065794903464,16.4055974478555,7.07238506352337));
#20732=CARTESIAN_POINT('Ctrl Pts',(-13.9354099523288,16.6134811841275,7.06358504530741));
#20733=CARTESIAN_POINT('Ctrl Pts',(-14.2674053951108,16.9733859386865,7.04313583862896));
#20734=CARTESIAN_POINT('Ctrl Pts',(-14.4688273826557,17.1207496834881,7.03228201402286));
#20735=CARTESIAN_POINT('Ctrl Pts',(-14.9213369984178,17.332445292316,7.01050893322144));
#20736=CARTESIAN_POINT('Ctrl Pts',(-15.1689206323108,17.3929123707671,6.99980695353036));
#20737=CARTESIAN_POINT('Ctrl Pts',(-15.662041736227,17.4133525920293,6.98067854085473));
#20738=CARTESIAN_POINT('Ctrl Pts',(-15.9027237815361,17.3775040697993,6.97114186392743));
#20739=CARTESIAN_POINT('Ctrl Pts',(-16.3663937750528,17.2149213346843,6.95002019459603));
#20740=CARTESIAN_POINT('Ctrl Pts',(-16.5838442157415,17.0864664974281,6.93897273071463));
#20741=CARTESIAN_POINT('Ctrl Pts',(-16.9571170705607,16.7524798042926,6.91752666241261));
#20742=CARTESIAN_POINT('Ctrl Pts',(-17.1091169017913,16.5500566576449,6.90793423699233));
#20743=CARTESIAN_POINT('Ctrl Pts',(-17.3229804931394,16.1042880116648,6.8884342962233));
#20744=CARTESIAN_POINT('Ctrl Pts',(-17.3852518264387,15.8663707366947,6.87802671639084));
#20745=CARTESIAN_POINT('Ctrl Pts',(-17.4036733949879,15.5821367961441,6.86559303570184));
#20746=CARTESIAN_POINT('Ctrl Pts',(-17.405,15.5410465275867,6.86379556113674));
#20747=CARTESIAN_POINT('Ctrl Pts',(-17.405,15.5,6.86199999999996));
#20748=CARTESIAN_POINT('Origin',(-15.5,15.5,-1.713));
#20749=CARTESIAN_POINT('',(-17.405,15.5,6.29949999999991));
#20750=CARTESIAN_POINT('',(-17.405,15.5,6.36199999999995));
#20751=CARTESIAN_POINT('',(-17.405,15.5,-1.713));
#20752=CARTESIAN_POINT('Ctrl Pts',(-17.405,15.5,6.29949999999991));
#20753=CARTESIAN_POINT('Ctrl Pts',(-17.405,15.5669742781042,6.30242975844716));
#20754=CARTESIAN_POINT('Ctrl Pts',(-17.4014681653938,15.6340281976763,6.30536300077314));
#20755=CARTESIAN_POINT('Ctrl Pts',(-17.3687838133474,15.9422510559641,6.31884606544015));
#20756=CARTESIAN_POINT('Ctrl Pts',(-17.2972902898554,16.1765419380487,6.32909501041323));
#20757=CARTESIAN_POINT('Ctrl Pts',(-17.0647622138604,16.6158967725631,6.3483143820018));
#20758=CARTESIAN_POINT('Ctrl Pts',(-16.9019625998521,16.814627588759,6.35847544040902));
#20759=CARTESIAN_POINT('Ctrl Pts',(-16.5120200024818,17.1330523072791,6.3802126475219));
#20760=CARTESIAN_POINT('Ctrl Pts',(-16.2900949650584,17.2512273505908,6.39120478408358));
#20761=CARTESIAN_POINT('Ctrl Pts',(-15.8209460953331,17.3931862699167,6.4120829248973));
#20762=CARTESIAN_POINT('Ctrl Pts',(-15.5790321175968,17.4185669224691,6.42120921772569));
#20763=CARTESIAN_POINT('Ctrl Pts',(-15.0872730490648,17.3768088108984,6.44075230178849));
#20764=CARTESIAN_POINT('Ctrl Pts',(-14.8424897793338,17.3056617463602,6.45158178832733));
#20765=CARTESIAN_POINT('Ctrl Pts',(-14.4004491373596,17.0750001587067,6.47337309275785));
#20766=CARTESIAN_POINT('Ctrl Pts',(-14.2063049243362,16.9198602281328,6.48412128986035));
#20767=CARTESIAN_POINT('Ctrl Pts',(-13.8892586880858,16.5459772061103,6.504309899037));
#20768=CARTESIAN_POINT('Ctrl Pts',(-13.7686807192717,16.331318436343,6.51313436411438));
#20769=CARTESIAN_POINT('Ctrl Pts',(-13.6122230850309,15.8596154661282,6.53376878975806));
#20770=CARTESIAN_POINT('Ctrl Pts',(-13.5812057389649,15.6060313522453,6.54486170812565));
#20771=CARTESIAN_POINT('Ctrl Pts',(-13.6192942000783,15.1111421259293,6.56651040568978));
#20772=CARTESIAN_POINT('Ctrl Pts',(-13.6843089867792,14.8742591769762,6.57687273941476));
#20773=CARTESIAN_POINT('Ctrl Pts',(-13.9036751911704,14.4303598896421,6.59629090596482));
#20774=CARTESIAN_POINT('Ctrl Pts',(-14.0588191332799,14.2290142456763,6.6060351546427));
#20775=CARTESIAN_POINT('Ctrl Pts',(-14.4370019565762,13.8995415593533,6.62756850002376));
#20776=CARTESIAN_POINT('Ctrl Pts',(-14.6558129771089,13.7740855777316,6.63860191617512));
#20777=CARTESIAN_POINT('Ctrl Pts',(-15.1211196278604,13.6175516623919,6.65965328703122));
#20778=CARTESIAN_POINT('Ctrl Pts',(-15.362141385934,13.5847635605764,6.66905348724296));
#20779=CARTESIAN_POINT('Ctrl Pts',(-15.8548982851256,13.6114064367251,6.68830376854936));
#20780=CARTESIAN_POINT('Ctrl Pts',(-16.1017164620508,13.6749924589575,6.69904496813158));
#20781=CARTESIAN_POINT('Ctrl Pts',(-16.5512641515885,13.8922557714788,6.72082761798341));
#20782=CARTESIAN_POINT('Ctrl Pts',(-16.7505999094325,14.0419164102183,6.73165264639748));
#20783=CARTESIAN_POINT('Ctrl Pts',(-17.0782652109025,14.4059003364521,6.75202703126749));
#20784=CARTESIAN_POINT('Ctrl Pts',(-17.2047080459699,14.6157239430174,6.76081775778718));
#20785=CARTESIAN_POINT('Ctrl Pts',(-17.3655964399404,15.054098393127,6.77999424291883));
#20786=CARTESIAN_POINT('Ctrl Pts',(-17.405,15.2763071874294,6.78971466261713));
#20787=CARTESIAN_POINT('Ctrl Pts',(-17.405,15.5,6.79949999999992));
#20788=CARTESIAN_POINT('Ctrl Pts',(-17.405,15.5,6.86199999999996));
#20789=CARTESIAN_POINT('Ctrl Pts',(-17.405,15.2884438551032,6.85274557546379));
#20790=CARTESIAN_POINT('Ctrl Pts',(-17.3697559300109,15.0780496586515,6.84354197981851));
#20791=CARTESIAN_POINT('Ctrl Pts',(-17.2208852103652,14.6474394617906,6.82470513831103));
#20792=CARTESIAN_POINT('Ctrl Pts',(-17.0979639297337,14.4347222488425,6.81590369562122));
#20793=CARTESIAN_POINT('Ctrl Pts',(-16.776680761579,14.0647723813145,6.79564060204316));
#20794=CARTESIAN_POINT('Ctrl Pts',(-16.5804526031638,13.9117925937642,6.78486070423475));
#20795=CARTESIAN_POINT('Ctrl Pts',(-16.1353758746613,13.6864332346946,6.76307035283269));
#20796=CARTESIAN_POINT('Ctrl Pts',(-15.8897541185117,13.6182879012923,6.75227475584018));
#20797=CARTESIAN_POINT('Ctrl Pts',(-15.3975788836265,13.5825451244441,6.73284747478383));
#20798=CARTESIAN_POINT('Ctrl Pts',(-15.1560309139864,13.6108658278522,6.72362209621475));
#20799=CARTESIAN_POINT('Ctrl Pts',(-14.6883869547904,13.7585972478523,6.70267470957475));
#20800=CARTESIAN_POINT('Ctrl Pts',(-14.4676672708304,13.8796646900924,6.69166497315547));
#20801=CARTESIAN_POINT('Ctrl Pts',(-14.0823695986942,14.202494243938,6.67000739008409));
#20802=CARTESIAN_POINT('Ctrl Pts',(-13.92261554486,14.4022645182293,6.66001992483683));
#20803=CARTESIAN_POINT('Ctrl Pts',(-13.6952840840443,14.8434260196211,6.64072152145137));
#20804=CARTESIAN_POINT('Ctrl Pts',(-13.6263340880438,15.0787599025041,6.63042695089656));
#20805=CARTESIAN_POINT('Ctrl Pts',(-13.5796896196656,15.5720489222286,6.60884825362078));
#20806=CARTESIAN_POINT('Ctrl Pts',(-13.6061342350988,15.8256758352762,6.59775346302376));
#20807=CARTESIAN_POINT('Ctrl Pts',(-13.7540997980542,16.3004960162174,6.5769826764559));
#20808=CARTESIAN_POINT('Ctrl Pts',(-13.8712975287011,16.517981966357,6.56810265670043));
#20809=CARTESIAN_POINT('Ctrl Pts',(-14.1822445273313,16.8974862231662,6.54802216114273));
#20810=CARTESIAN_POINT('Ctrl Pts',(-14.3733621908496,17.0556737310417,6.5373219640449));
#20811=CARTESIAN_POINT('Ctrl Pts',(-14.8109417400543,17.2938623446181,6.51553502998647));
#20812=CARTESIAN_POINT('Ctrl Pts',(-15.0544577816917,17.3692926308519,6.5046598671954));
#20813=CARTESIAN_POINT('Ctrl Pts',(-15.5455752341148,17.4196719474759,6.4849525247478));
#20814=CARTESIAN_POINT('Ctrl Pts',(-15.7880388344627,17.3984894506981,6.47594557206593));
#20815=CARTESIAN_POINT('Ctrl Pts',(-16.2592911603662,17.2647405448217,6.45516731577707));
#20816=CARTESIAN_POINT('Ctrl Pts',(-16.4828667093827,17.1506970735552,6.44420301828159));
#20817=CARTESIAN_POINT('Ctrl Pts',(-16.8765598212287,16.8408277807641,6.42251085369063));
#20818=CARTESIAN_POINT('Ctrl Pts',(-17.0418698243712,16.6468750229317,6.41216951106434));
#20819=CARTESIAN_POINT('Ctrl Pts',(-17.2823828232524,16.2147224745612,6.393265200112));
#20820=CARTESIAN_POINT('Ctrl Pts',(-17.3587288208372,15.9825144586595,6.38310736914518));
#20821=CARTESIAN_POINT('Ctrl Pts',(-17.3998554219865,15.6617515569817,6.36907574614965));
#20822=CARTESIAN_POINT('Ctrl Pts',(-17.405,15.5808319110706,6.36553595411502));
#20823=CARTESIAN_POINT('Ctrl Pts',(-17.405,15.5,6.36199999999995));
#20824=CARTESIAN_POINT('Origin',(-15.5,15.5,-1.713));
#20825=CARTESIAN_POINT('',(-17.405,15.5,5.7994999999999));
#20826=CARTESIAN_POINT('',(-17.405,15.5,5.86199999999995));
#20827=CARTESIAN_POINT('',(-17.405,15.5,-1.713));
#20828=CARTESIAN_POINT('Ctrl Pts',(-17.405,15.5,5.7994999999999));
#20829=CARTESIAN_POINT('Ctrl Pts',(-17.405,15.607624307934,5.80420797497514));
#20830=CARTESIAN_POINT('Ctrl Pts',(-17.3958796715229,15.7153059195385,5.8089184566726));
#20831=CARTESIAN_POINT('Ctrl Pts',(-17.3347501370527,16.0718927659009,5.82451718136037));
#20832=CARTESIAN_POINT('Ctrl Pts',(-17.2423928614072,16.3108035450705,5.83455884913306));
#20833=CARTESIAN_POINT('Ctrl Pts',(-16.9753304835568,16.7294096435034,5.85383207104165));
#20834=CARTESIAN_POINT('Ctrl Pts',(-16.8066941725831,16.9073295516354,5.86411217967549));
#20835=CARTESIAN_POINT('Ctrl Pts',(-16.4040076320726,17.1957315044031,5.88567551083158));
#20836=CARTESIAN_POINT('Ctrl Pts',(-16.1716143212648,17.3004661290847,5.89677025375238));
#20837=CARTESIAN_POINT('Ctrl Pts',(-15.6867554165738,17.4115894323903,5.91756910678677));
#20838=CARTESIAN_POINT('Ctrl Pts',(-15.439647193832,17.419741280294,5.92646397301758));
#20839=CARTESIAN_POINT('Ctrl Pts',(-14.9551408247193,17.3418832337638,5.94652188409423));
#20840=CARTESIAN_POINT('Ctrl Pts',(-14.7223635928588,17.2563237175178,5.95721176836094));
#20841=CARTESIAN_POINT('Ctrl Pts',(-14.2964260852282,16.9980504147149,5.97899695442543));
#20842=CARTESIAN_POINT('Ctrl Pts',(-14.1087140860853,16.8255518986737,5.98988114593346));
#20843=CARTESIAN_POINT('Ctrl Pts',(-13.8180496036205,16.4264347437861,6.00962223968831));
#20844=CARTESIAN_POINT('Ctrl Pts',(-13.7143526760721,16.2061957186731,6.0186077988331));
#20845=CARTESIAN_POINT('Ctrl Pts',(-13.5928784167332,15.7316795459691,6.03936528670292));
#20846=CARTESIAN_POINT('Ctrl Pts',(-13.5789510576611,15.4811760614512,6.05032344433238));
#20847=CARTESIAN_POINT('Ctrl Pts',(-13.6471560950891,14.9954922943206,6.07156945339331));
#20848=CARTESIAN_POINT('Ctrl Pts',(-13.7261405569804,14.7644691566145,6.08167545246647));
#20849=CARTESIAN_POINT('Ctrl Pts',(-13.9714778376261,14.3354041651447,6.10044469968738));
#20850=CARTESIAN_POINT('Ctrl Pts',(-14.1389919316573,14.1433938326413,6.11094512343558));
#20851=CARTESIAN_POINT('Ctrl Pts',(-14.5359866799602,13.8382635693377,6.13265871349906));
#20852=CARTESIAN_POINT('Ctrl Pts',(-14.7605810771286,13.7268799501902,6.14360343191852));
#20853=CARTESIAN_POINT('Ctrl Pts',(-15.2331602037098,13.5983967279777,6.16431678012604));
#20854=CARTESIAN_POINT('Ctrl Pts',(-15.4759944676697,13.5799183708665,6.17326070798783));
#20855=CARTESIAN_POINT('Ctrl Pts',(-15.9666683923341,13.6358680227389,6.19307308373893));
#20856=CARTESIAN_POINT('Ctrl Pts',(-16.2093249528404,13.7140529016083,6.20397593523624));
#20857=CARTESIAN_POINT('Ctrl Pts',(-16.6439545254303,13.9570579311734,6.22575645867812));
#20858=CARTESIAN_POINT('Ctrl Pts',(-16.8330924862036,14.1171836157561,6.23642404927922));
#20859=CARTESIAN_POINT('Ctrl Pts',(-17.1400816581269,14.5003102399934,6.2564338364048));
#20860=CARTESIAN_POINT('Ctrl Pts',(-17.255080234941,14.7196511698602,6.26536400568057));
#20861=CARTESIAN_POINT('Ctrl Pts',(-17.3782592374228,15.1320480082316,6.28340411234599));
#20862=CARTESIAN_POINT('Ctrl Pts',(-17.405,15.3157225386145,6.29143886870571));
#20863=CARTESIAN_POINT('Ctrl Pts',(-17.405,15.5,6.29949999999991));
#20864=CARTESIAN_POINT('Ctrl Pts',(-17.405,15.5,6.36199999999995));
#20865=CARTESIAN_POINT('Ctrl Pts',(-17.405,15.3302508811004,6.35457440424756));
#20866=CARTESIAN_POINT('Ctrl Pts',(-17.3823098623818,15.1608886824466,6.34716573414024));
#20867=CARTESIAN_POINT('Ctrl Pts',(-17.2720539956363,14.7585888660469,6.3295673169749));
#20868=CARTESIAN_POINT('Ctrl Pts',(-17.1612889929575,14.5356460396956,6.32051012645561));
#20869=CARTESIAN_POINT('Ctrl Pts',(-16.8618897192935,14.1456273570438,6.30063712915929));
#20870=CARTESIAN_POINT('Ctrl Pts',(-16.6765800686231,13.9818721663105,6.29003518425932));
#20871=CARTESIAN_POINT('Ctrl Pts',(-16.2457052882105,13.7285967342994,6.26817226992455));
#20872=CARTESIAN_POINT('Ctrl Pts',(-16.0023445596127,13.6448414733778,6.25712090493287));
#20873=CARTESIAN_POINT('Ctrl Pts',(-15.510097417241,13.5797544998568,6.23704907566801));
#20874=CARTESIAN_POINT('Ctrl Pts',(-15.2666510046418,13.5939572944337,6.22818264194464));
#20875=CARTESIAN_POINT('Ctrl Pts',(-14.7920185730827,13.7141549326478,6.20757273108299));
#20876=CARTESIAN_POINT('Ctrl Pts',(-14.5658843790827,13.821339394038,6.19666152428667));
#20877=CARTESIAN_POINT('Ctrl Pts',(-14.1638391967449,14.1189278523225,6.17492156057207));
#20878=CARTESIAN_POINT('Ctrl Pts',(-13.9928464481022,14.3078589220662,6.16431134189055));
#20879=CARTESIAN_POINT('Ctrl Pts',(-13.7399799463516,14.7320915034382,6.14545285085959));
#20880=CARTESIAN_POINT('Ctrl Pts',(-13.656870508123,14.9612272192553,6.13556836311214));
#20881=CARTESIAN_POINT('Ctrl Pts',(-13.5792709743863,15.4475415209429,6.11429477161225));
#20882=CARTESIAN_POINT('Ctrl Pts',(-13.5890590453456,15.7006488462555,6.1032227101375));
#20883=CARTESIAN_POINT('Ctrl Pts',(-13.7056349573522,16.1863755603015,6.08197482238395));
#20884=CARTESIAN_POINT('Ctrl Pts',(-13.8104358762094,16.4144498835814,6.07267281343426));
#20885=CARTESIAN_POINT('Ctrl Pts',(-14.1039832532025,16.820568086407,6.05266937566003));
#20886=CARTESIAN_POINT('Ctrl Pts',(-14.2910746473196,16.9937345530823,6.04179408530873));
#20887=CARTESIAN_POINT('Ctrl Pts',(-14.716154040337,17.2535730471962,6.02000717367115));
#20888=CARTESIAN_POINT('Ctrl Pts',(-14.9487104303037,17.339980014467,6.00930712007716));
#20889=CARTESIAN_POINT('Ctrl Pts',(-15.4328494820932,17.4194924007523,5.98922694024529));
#20890=CARTESIAN_POINT('Ctrl Pts',(-15.6797989499746,17.4122329811197,5.98034672057336));
#20891=CARTESIAN_POINT('Ctrl Pts',(-16.1649834712463,17.3029388767399,5.95957554064623));
#20892=CARTESIAN_POINT('Ctrl Pts',(-16.3978464847786,17.1990156042947,5.94848074967756));
#20893=CARTESIAN_POINT('Ctrl Pts',(-16.8017084293941,16.9119567131846,5.92690226545998));
#20894=CARTESIAN_POINT('Ctrl Pts',(-16.9710288589272,16.7345697444875,5.91660789635657));
#20895=CARTESIAN_POINT('Ctrl Pts',(-17.2394016216833,16.3170980789924,5.89730984460776));
#20896=CARTESIAN_POINT('Ctrl Pts',(-17.3325199503514,16.0788524545823,5.88732162968424));
#20897=CARTESIAN_POINT('Ctrl Pts',(-17.3954472466174,15.72034309072,5.8716388053683));
#20898=CARTESIAN_POINT('Ctrl Pts',(-17.405,15.6101460660609,5.8668182881041));
#20899=CARTESIAN_POINT('Ctrl Pts',(-17.405,15.5,5.86199999999995));
#20900=CARTESIAN_POINT('Origin',(-15.5,15.5,-1.713));
#20901=CARTESIAN_POINT('',(-17.405,15.5,5.2994999999999));
#20902=CARTESIAN_POINT('',(-17.405,15.5,5.36199999999994));
#20903=CARTESIAN_POINT('',(-17.405,15.5,-1.713));
#20904=CARTESIAN_POINT('Ctrl Pts',(-17.405,15.5,5.2994999999999));
#20905=CARTESIAN_POINT('Ctrl Pts',(-17.405,15.6490875914274,5.30602176690398));
#20906=CARTESIAN_POINT('Ctrl Pts',(-17.3874977888974,15.7980127697812,5.31253642912411));
#20907=CARTESIAN_POINT('Ctrl Pts',(-17.2946926680793,16.1855303593754,5.32948820469691));
#20908=CARTESIAN_POINT('Ctrl Pts',(-17.189983289926,16.4136838746745,5.33879455276844));
#20909=CARTESIAN_POINT('Ctrl Pts',(-16.9013559622059,16.8133636006812,5.35847077591085));
#20910=CARTESIAN_POINT('Ctrl Pts',(-16.7215432471211,16.9820716592986,5.36897280602877));
#20911=CARTESIAN_POINT('Ctrl Pts',(-16.2998513511192,17.2475038146678,5.39075373219641));
#20912=CARTESIAN_POINT('Ctrl Pts',(-16.0599908077106,17.3384658143737,5.40183012431409));
#20913=CARTESIAN_POINT('Ctrl Pts',(-15.570056397893,17.4190962505169,5.42215430905432));
#20914=CARTESIAN_POINT('Ctrl Pts',(-15.325456662796,17.4124265145795,5.43094994342898));
#20915=CARTESIAN_POINT('Ctrl Pts',(-14.8473377086516,17.3066933148065,5.45137556723504));
#20916=CARTESIAN_POINT('Ctrl Pts',(-14.6187026292344,17.2068726812802,5.46222045366264));
#20917=CARTESIAN_POINT('Ctrl Pts',(-14.2080495792291,16.9225236407745,5.4839969407011));
#20918=CARTESIAN_POINT('Ctrl Pts',(-14.0311552063945,16.7390432767342,5.49471151649644));
#20919=CARTESIAN_POINT('Ctrl Pts',(-13.7652495010312,16.3232866491125,5.51387859478455));
#20920=CARTESIAN_POINT('Ctrl Pts',(-13.6750614412334,16.0973188620358,5.52337056596503));
#20921=CARTESIAN_POINT('Ctrl Pts',(-13.5821051334709,15.6149847480906,5.54447004601513));
#20922=CARTESIAN_POINT('Ctrl Pts',(-13.5835849443739,15.3625370642135,5.55551325178403));
#20923=CARTESIAN_POINT('Ctrl Pts',(-13.6841742256802,14.871643483799,5.57698716168843));
#20924=CARTESIAN_POINT('Ctrl Pts',(-13.7826847966996,14.6381052044559,5.58662636944033));
#20925=CARTESIAN_POINT('Ctrl Pts',(-14.0604137005514,14.2287920034237,5.60610042397301));
#20926=CARTESIAN_POINT('Ctrl Pts',(-14.2346020090227,14.0553110198802,5.61649377445202));
#20927=CARTESIAN_POINT('Ctrl Pts',(-14.6467831693807,13.7780403942228,5.63817333126129));
#20928=CARTESIAN_POINT('Ctrl Pts',(-14.8829419130355,13.6800069155095,5.649264154126));
#20929=CARTESIAN_POINT('Ctrl Pts',(-15.3703854233353,13.5838625400674,5.66983329894448));
#20930=CARTESIAN_POINT('Ctrl Pts',(-15.6162252426114,13.5830038782554,5.67864068030565));
#20931=CARTESIAN_POINT('Ctrl Pts',(-16.0976645942582,13.6744743713744,5.69888013592539));
#20932=CARTESIAN_POINT('Ctrl Pts',(-16.3285308321627,13.7670050027371,5.70965009841809));
#20933=CARTESIAN_POINT('Ctrl Pts',(-16.7472223115211,14.0380951674903,5.73144111065996));
#20934=CARTESIAN_POINT('Ctrl Pts',(-16.9297461722653,14.2160309225986,5.74224768011558));
#20935=CARTESIAN_POINT('Ctrl Pts',(-17.2083821419098,14.6233255343363,5.76171194669427));
#20936=CARTESIAN_POINT('Ctrl Pts',(-17.3054989818797,14.8463034602087,5.77090435084015));
#20937=CARTESIAN_POINT('Ctrl Pts',(-17.3894642425502,15.2191704996068,5.78721524495205));
#20938=CARTESIAN_POINT('Ctrl Pts',(-17.405,15.3595364453997,5.7933554875502));
#20939=CARTESIAN_POINT('Ctrl Pts',(-17.405,15.5,5.7994999999999));
#20940=CARTESIAN_POINT('Ctrl Pts',(-17.405,15.5,5.86199999999995));
#20941=CARTESIAN_POINT('Ctrl Pts',(-17.405,15.3619687117345,5.85596188590259));
#20942=CARTESIAN_POINT('Ctrl Pts',(-17.3899976664485,15.2240174501072,5.8499272725331));
#20943=CARTESIAN_POINT('Ctrl Pts',(-17.3079876536534,14.8532208083365,5.83370694699631));
#20944=CARTESIAN_POINT('Ctrl Pts',(-17.2117279799498,14.6298789440439,5.82448203792766));
#20945=CARTESIAN_POINT('Ctrl Pts',(-16.9346639441148,14.2215290025838,5.80505423984198));
#20946=CARTESIAN_POINT('Ctrl Pts',(-16.7528277205932,14.0428968294752,5.79425848850987));
#20947=CARTESIAN_POINT('Ctrl Pts',(-16.3351086117615,13.770152156226,5.77246812558253));
#20948=CARTESIAN_POINT('Ctrl Pts',(-16.1045063871937,13.6767162920844,5.76168836544625));
#20949=CARTESIAN_POINT('Ctrl Pts',(-15.6234730666851,13.5834768813911,5.74142560162412));
#20950=CARTESIAN_POINT('Ctrl Pts',(-15.3777916705263,13.5833958255771,5.73262408439776));
#20951=CARTESIAN_POINT('Ctrl Pts',(-14.8900277034025,13.6776059092146,5.71208510677751));
#20952=CARTESIAN_POINT('Ctrl Pts',(-14.6533962925942,13.7747647786244,5.70099550713628));
#20953=CARTESIAN_POINT('Ctrl Pts',(-14.2400110887766,14.0505762177703,5.67930225220943));
#20954=CARTESIAN_POINT('Ctrl Pts',(-14.0651143574527,14.2234717132942,5.66889486987666));
#20955=CARTESIAN_POINT('Ctrl Pts',(-13.7860184999547,14.6315843224716,5.64939528950602));
#20956=CARTESIAN_POINT('Ctrl Pts',(-13.6867258707621,14.8644412284995,5.63980222097551));
#20957=CARTESIAN_POINT('Ctrl Pts',(-13.5841493983871,15.3547072418563,5.61835576369831));
#20958=CARTESIAN_POINT('Ctrl Pts',(-13.5816439640591,15.6072509385608,5.60730835789322));
#20959=CARTESIAN_POINT('Ctrl Pts',(-13.6727049726614,16.0900852469167,5.58618699707275));
#20960=CARTESIAN_POINT('Ctrl Pts',(-13.7620126940766,16.316440786022,5.57665095211607));
#20961=CARTESIAN_POINT('Ctrl Pts',(-14.026297880845,16.7332610794051,5.55752200057289));
#20962=CARTESIAN_POINT('Ctrl Pts',(-14.2024659946565,16.9174315372379,5.5468198443693));
#20963=CARTESIAN_POINT('Ctrl Pts',(-14.6120694412223,17.2034450886869,5.52504671375127));
#20964=CARTESIAN_POINT('Ctrl Pts',(-14.8404054292413,17.3041867794144,5.51419301245704));
#20965=CARTESIAN_POINT('Ctrl Pts',(-15.3180958718409,17.4117254104433,5.49374413345657));
#20966=CARTESIAN_POINT('Ctrl Pts',(-15.5625458017275,17.4193406628748,5.48494418539988));
#20967=CARTESIAN_POINT('Ctrl Pts',(-16.0527803027092,17.3406608105051,5.46465129573029));
#20968=CARTESIAN_POINT('Ctrl Pts',(-16.2930916782223,17.2505967635547,5.45357746460658));
#20969=CARTESIAN_POINT('Ctrl Pts',(-16.7159552806254,16.9866743745706,5.43178517167092));
#20970=CARTESIAN_POINT('Ctrl Pts',(-16.8964656036269,16.8185786568013,5.42127010674313));
#20971=CARTESIAN_POINT('Ctrl Pts',(-17.1864527192459,16.4201107912361,5.40156887569857));
#20972=CARTESIAN_POINT('Ctrl Pts',(-17.2919300783062,16.1926212949345,5.3922983943541));
#20973=CARTESIAN_POINT('Ctrl Pts',(-17.3868794224892,15.803210383172,5.37526379628925));
#20974=CARTESIAN_POINT('Ctrl Pts',(-17.405,15.6516981483465,5.36863596449454));
#20975=CARTESIAN_POINT('Ctrl Pts',(-17.405,15.5,5.36199999999994));
#20976=CARTESIAN_POINT('Origin',(-15.5,15.5,-1.713));
#20977=CARTESIAN_POINT('',(-17.405,15.5,4.79949999999989));
#20978=CARTESIAN_POINT('',(-17.405,15.5,4.86199999999993));
#20979=CARTESIAN_POINT('',(-17.405,15.5,-1.713));
#20980=CARTESIAN_POINT('Ctrl Pts',(-17.405,15.5,4.79949999999989));
#20981=CARTESIAN_POINT('Ctrl Pts',(-17.405,15.6915631165309,4.80787983886826));
#20982=CARTESIAN_POINT('Ctrl Pts',(-17.3761027908371,15.8823946807576,4.81622767632339));
#20983=CARTESIAN_POINT('Ctrl Pts',(-17.2462428313094,16.2997547529611,4.83448489732968));
#20984=CARTESIAN_POINT('Ctrl Pts',(-17.1291261431025,16.5173088515136,4.84336657042241));
#20985=CARTESIAN_POINT('Ctrl Pts',(-16.8183251554813,16.8969470943868,4.86344446509599));
#20986=CARTESIAN_POINT('Ctrl Pts',(-16.6272803126036,17.0552066573078,4.87414347947283));
#20987=CARTESIAN_POINT('Ctrl Pts',(-16.1898088341769,17.2935739128674,4.89593022669629));
#20988=CARTESIAN_POINT('Ctrl Pts',(-15.9463239856834,17.3691061729049,4.90680643816831));
#20989=CARTESIAN_POINT('Ctrl Pts',(-15.4552225136842,17.4196913240906,4.9265176772838));
#20990=CARTESIAN_POINT('Ctrl Pts',(-15.2127454325004,17.398608859155,4.93552210512798));
#20991=CARTESIAN_POINT('Ctrl Pts',(-14.7414436346965,17.265055070943,4.95629796793872));
#20992=CARTESIAN_POINT('Ctrl Pts',(-14.5178297768122,17.1511100267658,4.96726156389913));
#20993=CARTESIAN_POINT('Ctrl Pts',(-14.124013342636,16.8414157801667,4.98895457176108));
#20994=CARTESIAN_POINT('Ctrl Pts',(-13.9586212615899,16.6475345981838,4.99930163612475));
#20995=CARTESIAN_POINT('Ctrl Pts',(-13.7179287628858,16.2154955524047,5.01820098195934));
#20996=CARTESIAN_POINT('Ctrl Pts',(-13.6414846626363,15.9833309251378,5.02835691491065));
#20997=CARTESIAN_POINT('Ctrl Pts',(-13.5784639975189,15.4935345675145,5.04978282731762));
#20998=CARTESIAN_POINT('Ctrl Pts',(-13.59611601601,15.2400493117157,5.06087142118459));
#20999=CARTESIAN_POINT('Ctrl Pts',(-13.7276102201286,14.7593829644292,5.08189794556283));
#21000=CARTESIAN_POINT('Ctrl Pts',(-13.8382890535805,14.5363664403885,5.090958131516));
#21001=CARTESIAN_POINT('Ctrl Pts',(-14.1375343006581,14.1462086260846,5.11082833681272));
#21002=CARTESIAN_POINT('Ctrl Pts',(-14.3227658536095,13.9823809721575,5.12142890800266));
#21003=CARTESIAN_POINT('Ctrl Pts',(-14.7535109844111,13.7289285569402,5.1432907817314));
#21004=CARTESIAN_POINT('Ctrl Pts',(-14.9968228405967,13.645068755593,5.15434258178268));
#21005=CARTESIAN_POINT('Ctrl Pts',(-15.4890379478735,13.5797580488182,5.1744180909872));
#21006=CARTESIAN_POINT('Ctrl Pts',(-15.7325002956529,13.5938523991739,5.18328291172378));
#21007=CARTESIAN_POINT('Ctrl Pts',(-16.2071841013761,13.7138405611191,5.20389018711722));
#21008=CARTESIAN_POINT('Ctrl Pts',(-16.4333562159829,13.8209186591222,5.2148005040848));
#21009=CARTESIAN_POINT('Ctrl Pts',(-16.8355292739374,14.1183170077084,5.23654115409353));
#21010=CARTESIAN_POINT('Ctrl Pts',(-17.0066088233403,14.3071704386349,5.24715296298741));
#21011=CARTESIAN_POINT('Ctrl Pts',(-17.2596650716638,14.7312810048394,5.2660159736058));
#21012=CARTESIAN_POINT('Ctrl Pts',(-17.3428774803348,14.9603698228013,5.27589413048106));
#21013=CARTESIAN_POINT('Ctrl Pts',(-17.397031820958,15.2987316456968,5.2906956100478));
#21014=CARTESIAN_POINT('Ctrl Pts',(-17.405,15.3994027954335,5.29509942237232));
#21015=CARTESIAN_POINT('Ctrl Pts',(-17.405,15.5,5.2994999999999));
#21016=CARTESIAN_POINT('Ctrl Pts',(-17.405,15.5,5.36199999999994));
#21017=CARTESIAN_POINT('Ctrl Pts',(-17.405,15.4019038262264,5.35770882879374));
#21018=CARTESIAN_POINT('Ctrl Pts',(-17.3974231139549,15.3037299106598,5.35341425680927));
#21019=CARTESIAN_POINT('Ctrl Pts',(-17.344979858954,14.9675672590125,5.33870897895943));
#21020=CARTESIAN_POINT('Ctrl Pts',(-17.262631280343,14.7380842724675,5.32877714796658));
#21021=CARTESIAN_POINT('Ctrl Pts',(-17.0111668090028,14.3129513102799,5.30995207791304));
#21022=CARTESIAN_POINT('Ctrl Pts',(-16.8408162368535,14.1234481187272,5.29935367376576));
#21023=CARTESIAN_POINT('Ctrl Pts',(-16.4397182602489,13.8244573193156,5.27761892149752));
#21024=CARTESIAN_POINT('Ctrl Pts',(-16.2138656386321,13.7164876949478,5.26670120846099));
#21025=CARTESIAN_POINT('Ctrl Pts',(-15.7396134010243,13.5947431526479,5.24607186652224));
#21026=CARTESIAN_POINT('Ctrl Pts',(-15.4962839632397,13.5797400887434,5.23719299096207));
#21027=CARTESIAN_POINT('Ctrl Pts',(-15.0038015418331,13.6431761226221,5.21714835820639));
#21028=CARTESIAN_POINT('Ctrl Pts',(-14.7600815571484,13.7261592765739,5.20610027093066));
#21029=CARTESIAN_POINT('Ctrl Pts',(-14.3282524044727,13.9781269882643,5.18422980408214));
#21030=CARTESIAN_POINT('Ctrl Pts',(-14.1423674143573,14.1413464337119,5.17361778105738));
#21031=CARTESIAN_POINT('Ctrl Pts',(-13.8418324877926,14.5303383904024,5.15372421765079));
#21032=CARTESIAN_POINT('Ctrl Pts',(-13.7304324860787,14.7527385717229,5.14468860141197));
#21033=CARTESIAN_POINT('Ctrl Pts',(-13.5971113315973,15.2327697208616,5.1236898634794));
#21034=CARTESIAN_POINT('Ctrl Pts',(-13.5784894764905,15.4862851087353,5.11259995149892));
#21035=CARTESIAN_POINT('Ctrl Pts',(-13.6397087259588,15.9764936508038,5.09115600827632));
#21036=CARTESIAN_POINT('Ctrl Pts',(-13.7153309275349,16.2090202047905,5.08098424301005));
#21037=CARTESIAN_POINT('Ctrl Pts',(-13.9545192833494,16.6420070811145,5.0620434347719));
#21038=CARTESIAN_POINT('Ctrl Pts',(-14.1192234089349,16.8364863803383,5.05174385015941));
#21039=CARTESIAN_POINT('Ctrl Pts',(-14.5120053035011,17.1476444104558,5.03005801840527));
#21040=CARTESIAN_POINT('Ctrl Pts',(-14.735297199777,17.2624129624023,5.01908860761755));
#21041=CARTESIAN_POINT('Ctrl Pts',(-15.2061841812833,17.3975998855666,4.99829273929394));
#21042=CARTESIAN_POINT('Ctrl Pts',(-15.448549029226,17.4195192309441,4.9892667306742));
#21043=CARTESIAN_POINT('Ctrl Pts',(-15.9397831942183,17.3706555599016,4.96958811730537));
#21044=CARTESIAN_POINT('Ctrl Pts',(-16.1835275815734,17.2959765775398,4.95872073661156));
#21045=CARTESIAN_POINT('Ctrl Pts',(-16.6219006739087,17.0591049338943,4.9369325451802));
#21046=CARTESIAN_POINT('Ctrl Pts',(-16.8135537499556,16.9014490198769,4.9262236917428));
#21047=CARTESIAN_POINT('Ctrl Pts',(-17.1255753275233,16.5229316751174,4.90612407297281));
#21048=CARTESIAN_POINT('Ctrl Pts',(-17.2433693043559,16.3059465957354,4.89725575659387));
#21049=CARTESIAN_POINT('Ctrl Pts',(-17.3753951061978,15.8870131088787,4.87892970730005));
#21050=CARTESIAN_POINT('Ctrl Pts',(-17.405,15.6938944322268,4.87048182118221));
#21051=CARTESIAN_POINT('Ctrl Pts',(-17.405,15.5,4.86199999999993));
#21052=CARTESIAN_POINT('Origin',(-15.5,15.5,-1.713));
#21053=CARTESIAN_POINT('',(-17.405,15.5,4.29949999999989));
#21054=CARTESIAN_POINT('',(-17.405,15.5,4.36199999999993));
#21055=CARTESIAN_POINT('',(-17.405,15.5,-1.713));
#21056=CARTESIAN_POINT('Ctrl Pts',(-17.405,15.5,4.29949999999989));
#21057=CARTESIAN_POINT('Ctrl Pts',(-17.405,15.7316143560873,4.30963186159601));
#21058=CARTESIAN_POINT('Ctrl Pts',(-17.3627567347742,15.961507388049,4.31968842467383));
#21059=CARTESIAN_POINT('Ctrl Pts',(-17.1938338138213,16.4048278056338,4.33908126883765));
#21060=CARTESIAN_POINT('Ctrl Pts',(-17.0650898508518,16.6127814998738,4.34788071653058));
#21061=CARTESIAN_POINT('Ctrl Pts',(-16.7332512944162,16.9728344984569,4.36832722217888));
#21062=CARTESIAN_POINT('Ctrl Pts',(-16.5319045679017,17.1202820929434,4.37918002958804));
#21063=CARTESIAN_POINT('Ctrl Pts',(-16.0795012341922,17.3321804659507,4.40095351892543));
#21064=CARTESIAN_POINT('Ctrl Pts',(-15.8319446713374,17.392760897025,4.41165695233938));
#21065=CARTESIAN_POINT('Ctrl Pts',(-15.3388363370757,17.4134262550738,4.43078980550267));
#21066=CARTESIAN_POINT('Ctrl Pts',(-15.0981422293757,17.3776890517327,4.44032128224835));
#21067=CARTESIAN_POINT('Ctrl Pts',(-14.6344121963986,17.2153265681764,4.46144040870655));
#21068=CARTESIAN_POINT('Ctrl Pts',(-14.4169115189193,17.086980672769,4.4724873929472));
#21069=CARTESIAN_POINT('Ctrl Pts',(-14.0434595959548,16.7531576246628,4.49393666575702));
#21070=CARTESIAN_POINT('Ctrl Pts',(-13.8913456195006,16.550773658121,4.50353439815721));
#21071=CARTESIAN_POINT('Ctrl Pts',(-13.6772812436004,16.1050729095015,4.52303136878798));
#21072=CARTESIAN_POINT('Ctrl Pts',(-13.6149094566655,15.8671928542976,4.53343732045919));
#21073=CARTESIAN_POINT('Ctrl Pts',(-13.5825512110825,15.3713167974186,4.5551291864644));
#21074=CARTESIAN_POINT('Ctrl Pts',(-13.6166230909332,15.1178055136802,4.5662189189114));
#21075=CARTESIAN_POINT('Ctrl Pts',(-13.7787288519487,14.6482137858557,4.58676098924494));
#21076=CARTESIAN_POINT('Ctrl Pts',(-13.901564546466,14.4354258053553,4.59556305285422));
#21077=CARTESIAN_POINT('Ctrl Pts',(-14.2226927406017,14.065331732804,4.6158234295064));
#21078=CARTESIAN_POINT('Ctrl Pts',(-14.4188449704033,13.9122723318701,4.62660219216974));
#21079=CARTESIAN_POINT('Ctrl Pts',(-14.8638116031428,13.6867180287382,4.64839263658595));
#21080=CARTESIAN_POINT('Ctrl Pts',(-15.1094033098687,13.618462555476,4.65918950419813));
#21081=CARTESIAN_POINT('Ctrl Pts',(-15.6015637489736,13.5824994210303,4.67862104445296));
#21082=CARTESIAN_POINT('Ctrl Pts',(-15.8431248716566,13.6107122496045,4.68784256256878));
#21083=CARTESIAN_POINT('Ctrl Pts',(-16.3108245138832,13.7582315620518,4.70878741942499));
#21084=CARTESIAN_POINT('Ctrl Pts',(-16.5315891397848,13.8791929198398,4.71979653811186));
#21085=CARTESIAN_POINT('Ctrl Pts',(-16.9170577878751,14.2018613025606,4.74145707323737));
#21086=CARTESIAN_POINT('Ctrl Pts',(-17.0769234362671,14.4015934816703,4.75145072098273));
#21087=CARTESIAN_POINT('Ctrl Pts',(-17.3044462179037,14.842688756663,4.77074622732537));
#21088=CARTESIAN_POINT('Ctrl Pts',(-17.3734901964393,15.0779846890365,4.78103913775291));
#21089=CARTESIAN_POINT('Ctrl Pts',(-17.4021618668534,15.3798527943734,4.79424421672653));
#21090=CARTESIAN_POINT('Ctrl Pts',(-17.405,15.439962325706,4.79687368003952));
#21091=CARTESIAN_POINT('Ctrl Pts',(-17.405,15.5,4.79949999999989));
#21092=CARTESIAN_POINT('Ctrl Pts',(-17.405,15.5,4.86199999999993));
#21093=CARTESIAN_POINT('Ctrl Pts',(-17.405,15.442180147366,4.85947069760999));
#21094=CARTESIAN_POINT('Ctrl Pts',(-17.4023676760667,15.384291310761,4.85693837754862));
#21095=CARTESIAN_POINT('Ctrl Pts',(-17.3749487573809,15.0844652353877,4.84382262621995));
#21096=CARTESIAN_POINT('Ctrl Pts',(-17.3066907671614,14.8488532982766,4.83351589231308));
#21097=CARTESIAN_POINT('Ctrl Pts',(-17.0807664256711,14.4072053923165,4.81419621138743));
#21098=CARTESIAN_POINT('Ctrl Pts',(-16.9218318768361,14.207155325346,4.80425372650585));
#21099=CARTESIAN_POINT('Ctrl Pts',(-16.5377915939255,13.8831427274651,4.7826179023581));
#21100=CARTESIAN_POINT('Ctrl Pts',(-16.3174037618294,13.7612960189594,4.77160369345465));
#21101=CARTESIAN_POINT('Ctrl Pts',(-15.8501699940223,13.6120055732969,4.75063774703041));
#21102=CARTESIAN_POINT('Ctrl Pts',(-15.608718013233,13.5828923181582,4.74138348216231));
#21103=CARTESIAN_POINT('Ctrl Pts',(-15.1164351703261,13.6170170003983,4.72198751589263));
#21104=CARTESIAN_POINT('Ctrl Pts',(-14.8705943170609,13.6843531721741,4.71120131685047));
#21105=CARTESIAN_POINT('Ctrl Pts',(-14.4247117857891,13.9082794227657,4.68941178384605));
#21106=CARTESIAN_POINT('Ctrl Pts',(-14.2279270505859,14.0606734938221,4.67862361169857));
#21107=CARTESIAN_POINT('Ctrl Pts',(-13.9055064884792,14.4295641212511,4.65834059721033));
#21108=CARTESIAN_POINT('Ctrl Pts',(-13.7819572656015,14.641762613156,4.64954319277536));
#21109=CARTESIAN_POINT('Ctrl Pts',(-13.6180694285514,15.1106825581303,4.62903050926817));
#21110=CARTESIAN_POINT('Ctrl Pts',(-13.5830318586544,15.3641634543827,4.61794210610752));
#21111=CARTESIAN_POINT('Ctrl Pts',(-13.6135760220822,15.8603378399028,4.59623718985554));
#21112=CARTESIAN_POINT('Ctrl Pts',(-13.6751098443104,16.0985268650805,4.58581772243744));
#21113=CARTESIAN_POINT('Ctrl Pts',(-13.8875008995235,16.5447927407348,4.56629603058904));
#21114=CARTESIAN_POINT('Ctrl Pts',(-14.0386649367322,16.7475029360245,4.55674198688621));
#21115=CARTESIAN_POINT('Ctrl Pts',(-14.4106247533747,17.0826873364552,4.53531946498705));
#21116=CARTESIAN_POINT('Ctrl Pts',(-14.6277054116799,17.2119400123398,4.52426855935693));
#21117=CARTESIAN_POINT('Ctrl Pts',(-15.0909343363085,17.3761369776451,4.50312829255253));
#21118=CARTESIAN_POINT('Ctrl Pts',(-15.3315286777462,17.4128011071027,4.49355297455963));
#21119=CARTESIAN_POINT('Ctrl Pts',(-15.8247422542316,17.3940092756639,4.4744571126853));
#21120=CARTESIAN_POINT('Ctrl Pts',(-16.0725224561213,17.3343724488225,4.46376584572063));
#21121=CARTESIAN_POINT('Ctrl Pts',(-16.5258074097486,17.1241629404857,4.44199589650089));
#21122=CARTESIAN_POINT('Ctrl Pts',(-16.7277793655432,16.9774142091866,4.43113468870475));
#21123=CARTESIAN_POINT('Ctrl Pts',(-17.0609228345532,16.6185952804082,4.41066573981338));
#21124=CARTESIAN_POINT('Ctrl Pts',(-17.1903862601901,16.4112227261169,4.40186101164118));
#21125=CARTESIAN_POINT('Ctrl Pts',(-17.3618494871938,15.9663776396961,4.38240147155279));
#21126=CARTESIAN_POINT('Ctrl Pts',(-17.405,15.7340888477603,4.37224010707606));
#21127=CARTESIAN_POINT('Ctrl Pts',(-17.405,15.5,4.36199999999993));
#21128=CARTESIAN_POINT('Origin',(-15.5,15.5,-1.713));
#21129=CARTESIAN_POINT('',(-17.405,15.5,3.79949999999988));
#21130=CARTESIAN_POINT('',(-17.405,15.5,3.86199999999992));
#21131=CARTESIAN_POINT('',(-17.405,15.5,-1.713));
#21132=CARTESIAN_POINT('Ctrl Pts',(-17.405,15.5,3.79949999999988));
#21133=CARTESIAN_POINT('Ctrl Pts',(-17.405,15.5176704969382,3.80027298761747));
#21134=CARTESIAN_POINT('Ctrl Pts',(-17.4047541376814,15.5353510584371,3.80104641550444));
#21135=CARTESIAN_POINT('Ctrl Pts',(-17.3972339401769,15.80536106744,3.81285787696563));
#21136=CARTESIAN_POINT('Ctrl Pts',(-17.3401239250485,16.0538100548939,3.82372616163116));
#21137=CARTESIAN_POINT('Ctrl Pts',(-17.1369822758118,16.5037390621237,3.84340809545575));
#21138=CARTESIAN_POINT('Ctrl Pts',(-16.9968851667794,16.7027258920315,3.85243186198737));
#21139=CARTESIAN_POINT('Ctrl Pts',(-16.6444891216015,17.0430522125178,3.87322569783866));
#21140=CARTESIAN_POINT('Ctrl Pts',(-16.4335067749666,17.1791147524432,3.88419452294358));
#21141=CARTESIAN_POINT('Ctrl Pts',(-15.9677211723474,17.3638605915779,3.90588109705348));
#21142=CARTESIAN_POINT('Ctrl Pts',(-15.7169626616863,17.4093499767944,3.91618546959334));
#21143=CARTESIAN_POINT('Ctrl Pts',(-15.2223975598373,17.4001805186165,3.93512206937967));
#21144=CARTESIAN_POINT('Ctrl Pts',(-14.9832024838002,17.349498823534,3.94529222947809));
#21145=CARTESIAN_POINT('Ctrl Pts',(-14.5280041766517,17.1575916214525,3.96673435103501));
#21146=CARTESIAN_POINT('Ctrl Pts',(-14.3177174993268,17.0147938586229,3.97782413607682));
#21147=CARTESIAN_POINT('Ctrl Pts',(-13.9685099193908,16.6594473181571,3.99882570675274));
#21148=CARTESIAN_POINT('Ctrl Pts',(-13.831514770583,16.4518042050906,4.00786377055572));
#21149=CARTESIAN_POINT('Ctrl Pts',(-13.6447368436005,15.9970916456269,4.02775495863375));
#21150=CARTESIAN_POINT('Ctrl Pts',(-13.5962401833917,15.7545273240917,4.03836582134307));
#21151=CARTESIAN_POINT('Ctrl Pts',(-13.593758117278,15.2545881601184,4.06023542606632));
#21152=CARTESIAN_POINT('Ctrl Pts',(-13.6436544882321,15.0020200803626,4.07128389849659));
#21153=CARTESIAN_POINT('Ctrl Pts',(-13.834779566897,14.5437277846285,4.09133168046222));
#21154=CARTESIAN_POINT('Ctrl Pts',(-13.969363896983,14.3404418930211,4.10020906843054));
#21155=CARTESIAN_POINT('Ctrl Pts',(-14.3117908874209,13.9904720051824,4.1208361645189));
#21156=CARTESIAN_POINT('Ctrl Pts',(-14.5181593317412,13.8487889523204,4.1317531304748));
#21157=CARTESIAN_POINT('Ctrl Pts',(-14.9775564642285,13.6507470886944,4.15348849875881));
#21158=CARTESIAN_POINT('Ctrl Pts',(-15.2268262960436,13.5978732610907,4.16408827656067));
#21159=CARTESIAN_POINT('Ctrl Pts',(-15.7207254532908,13.5924724783421,4.182917218313));
#21160=CARTESIAN_POINT('Ctrl Pts',(-15.960647006969,13.6358015845445,4.19284351716882));
#21161=CARTESIAN_POINT('Ctrl Pts',(-16.4201937842834,13.8132176501179,4.21413342163813));
#21162=CARTESIAN_POINT('Ctrl Pts',(-16.6341414924654,13.9489622633598,4.22520763235503));
#21163=CARTESIAN_POINT('Ctrl Pts',(-16.9953079945519,14.2938468480346,4.24643342667437));
#21164=CARTESIAN_POINT('Ctrl Pts',(-17.1396787721256,14.4989036810798,4.25570751010824));
#21165=CARTESIAN_POINT('Ctrl Pts',(-17.3399450798589,14.9492155337354,4.27540619132677));
#21166=CARTESIAN_POINT('Ctrl Pts',(-17.3953549173897,15.1895596350089,4.28591993153996));
#21167=CARTESIAN_POINT('Ctrl Pts',(-17.4046168492424,15.4558661493172,4.29756938535922));
#21168=CARTESIAN_POINT('Ctrl Pts',(-17.405,15.4779408815478,4.29853503418833));
#21169=CARTESIAN_POINT('Ctrl Pts',(-17.405,15.5,4.29949999999989));
#21170=CARTESIAN_POINT('Ctrl Pts',(-17.405,15.5,4.36199999999992));
#21171=CARTESIAN_POINT('Ctrl Pts',(-17.405,15.4802786628464,4.36113729933704));
#21172=CARTESIAN_POINT('Ctrl Pts',(-17.4046937566948,15.4605445496239,4.3602740397911));
#21173=CARTESIAN_POINT('Ctrl Pts',(-17.3964838036035,15.196462759103,4.34872190547259));
#21174=CARTESIAN_POINT('Ctrl Pts',(-17.3419245741628,14.9558334540293,4.33819568915266));
#21175=CARTESIAN_POINT('Ctrl Pts',(-17.1433286776143,14.5049708959333,4.31847291758239));
#21176=CARTESIAN_POINT('Ctrl Pts',(-16.9998815572957,14.2995927046866,4.30923236586305));
#21177=CARTESIAN_POINT('Ctrl Pts',(-16.6401991058068,13.9533939709778,4.28803404971522));
#21178=CARTESIAN_POINT('Ctrl Pts',(-16.4266950092731,13.8167660487444,4.2769573247578));
#21179=CARTESIAN_POINT('Ctrl Pts',(-15.9676626533492,13.6375389919569,4.25564729808314));
#21180=CARTESIAN_POINT('Ctrl Pts',(-15.7278271357321,13.5932983649885,4.24566819355739));
#21181=CARTESIAN_POINT('Ctrl Pts',(-15.2338436728025,13.5968793835659,4.22687586034501));
#21182=CARTESIAN_POINT('Ctrl Pts',(-14.9843861963398,13.6488319941837,4.2162891229395));
#21183=CARTESIAN_POINT('Ctrl Pts',(-14.5241843554176,13.8452078975466,4.19455970750693));
#21184=CARTESIAN_POINT('Ctrl Pts',(-14.3172284572202,13.9861932444804,4.18363574693085));
#21185=CARTESIAN_POINT('Ctrl Pts',(-13.9735457966652,14.3349566669919,4.16298746932207));
#21186=CARTESIAN_POINT('Ctrl Pts',(-13.8382681374568,14.5376960900176,4.15409553411999));
#21187=CARTESIAN_POINT('Ctrl Pts',(-13.6454549294062,14.9953080207069,4.1340775144048));
#21188=CARTESIAN_POINT('Ctrl Pts',(-13.594632734797,15.2477915561283,4.12303274032687));
#21189=CARTESIAN_POINT('Ctrl Pts',(-13.5953570499606,15.747914024217,4.10115511705089));
#21190=CARTESIAN_POINT('Ctrl Pts',(-13.6430324851627,15.9907274358747,4.09053335801075));
#21191=CARTESIAN_POINT('Ctrl Pts',(-13.8282206878626,16.4459517174347,4.07061978488913));
#21192=CARTESIAN_POINT('Ctrl Pts',(-13.9643588390081,16.6538987001136,4.06160432661678));
#21193=CARTESIAN_POINT('Ctrl Pts',(-14.3121609791575,17.0104560948599,4.04062951532048));
#21194=CARTESIAN_POINT('Ctrl Pts',(-14.5220046281817,17.1540729720191,4.02953859802139));
#21195=CARTESIAN_POINT('Ctrl Pts',(-14.9766756252456,17.3476734773997,4.00807941663418));
#21196=CARTESIAN_POINT('Ctrl Pts',(-15.2157743708606,17.3992116297402,3.99789417324461));
#21197=CARTESIAN_POINT('Ctrl Pts',(-15.710400153106,17.41008596889,3.97891798503961));
#21198=CARTESIAN_POINT('Ctrl Pts',(-15.9613230313347,17.3654556147342,3.96865837020476));
#21199=CARTESIAN_POINT('Ctrl Pts',(-16.4278239611227,17.1822738180355,3.94697890588126));
#21200=CARTESIAN_POINT('Ctrl Pts',(-16.6393341928236,17.0468755746498,3.93600461211458));
#21201=CARTESIAN_POINT('Ctrl Pts',(-16.9928872705094,16.7076783661737,3.91519163962551));
#21202=CARTESIAN_POINT('Ctrl Pts',(-17.1336257165707,16.5091847997703,3.90614631670038));
#21203=CARTESIAN_POINT('Ctrl Pts',(-17.3382578393871,16.0599716762618,3.88649569887411));
#21204=CARTESIAN_POINT('Ctrl Pts',(-17.3961992884504,15.8117186546584,3.87563598664299));
#21205=CARTESIAN_POINT('Ctrl Pts',(-17.404691385027,15.5396074743704,3.86373261042742));
#21206=CARTESIAN_POINT('Ctrl Pts',(-17.405,15.5197975511803,3.86286603460973));
#21207=CARTESIAN_POINT('Ctrl Pts',(-17.405,15.5,3.86199999999992));
#21208=CARTESIAN_POINT('Origin',(-15.5,15.5,-1.713));
#21209=CARTESIAN_POINT('',(-17.405,15.5,3.29949999999987));
#21210=CARTESIAN_POINT('',(-17.405,15.5,3.36199999999991));
#21211=CARTESIAN_POINT('',(-17.405,15.5,-1.713));
#21212=CARTESIAN_POINT('Ctrl Pts',(-17.405,15.5,3.29949999999987));
#21213=CARTESIAN_POINT('Ctrl Pts',(-17.405,15.5564229479164,3.30196819544678));
#21214=CARTESIAN_POINT('Ctrl Pts',(-17.4024933261743,15.61291045123,3.30443921483919));
#21215=CARTESIAN_POINT('Ctrl Pts',(-17.3750365175576,15.9206454284538,3.31790093737742));
#21216=CARTESIAN_POINT('Ctrl Pts',(-17.3028873277189,16.1650760840202,3.32859344199538));
#21217=CARTESIAN_POINT('Ctrl Pts',(-17.0727241164517,16.601693105207,3.34769304922141));
#21218=CARTESIAN_POINT('Ctrl Pts',(-16.920751105621,16.79177744042,3.35726387446552));
#21219=CARTESIAN_POINT('Ctrl Pts',(-16.547073310477,17.1109838535724,3.37840200526172));
#21220=CARTESIAN_POINT('Ctrl Pts',(-16.3266549814992,17.234437712566,3.38945252152817));
#21221=CARTESIAN_POINT('Ctrl Pts',(-15.8504405112782,17.3891718533417,3.41087775771578));
#21222=CARTESIAN_POINT('Ctrl Pts',(-15.5992868634806,17.4188283703308,3.42043617098827));
#21223=CARTESIAN_POINT('Ctrl Pts',(-15.1065785124235,17.3798068533132,3.43995536202857));
#21224=CARTESIAN_POINT('Ctrl Pts',(-14.8695183682189,17.3140913580522,3.45037346591032));
#21225=CARTESIAN_POINT('Ctrl Pts',(-14.4244806486061,17.0926303898112,3.47207707286342));
#21226=CARTESIAN_POINT('Ctrl Pts',(-14.2224268061852,16.9356296381043,3.4831656177594));
#21227=CARTESIAN_POINT('Ctrl Pts',(-13.8981248505675,16.5593608623171,3.50368128354923));
#21228=CARTESIAN_POINT('Ctrl Pts',(-13.7760423459017,16.3462976357972,3.51247910604536));
#21229=CARTESIAN_POINT('Ctrl Pts',(-13.6176127567415,15.8826803267161,3.53275982822738));
#21230=CARTESIAN_POINT('Ctrl Pts',(-13.583937438819,15.6360843793156,3.54354705252312));
#21231=CARTESIAN_POINT('Ctrl Pts',(-13.6127634592529,15.1379732216046,3.56533669196804));
#21232=CARTESIAN_POINT('Ctrl Pts',(-13.6772757298006,14.8913758199954,3.57612397987746));
#21233=CARTESIAN_POINT('Ctrl Pts',(-13.8936967036479,14.4479014725849,3.59552355762946));
#21234=CARTESIAN_POINT('Ctrl Pts',(-14.0395619017465,14.2532993430224,3.60477444596417));
#21235=CARTESIAN_POINT('Ctrl Pts',(-14.4023361163371,13.9231773424532,3.62573825549865));
#21236=CARTESIAN_POINT('Ctrl Pts',(-14.6179938004087,13.7931610755427,3.63675195481547));
#21237=CARTESIAN_POINT('Ctrl Pts',(-15.0905715941891,13.622384990327,3.65839029327942));
#21238=CARTESIAN_POINT('Ctrl Pts',(-15.3433065988528,13.5846707710406,3.66833792298843));
#21239=CARTESIAN_POINT('Ctrl Pts',(-15.8387796964528,13.609669902849,3.68765515200495));
#21240=CARTESIAN_POINT('Ctrl Pts',(-16.0769668684721,13.6682775324893,3.69796048694128));
#21241=CARTESIAN_POINT('Ctrl Pts',(-16.5270481052016,13.8758106202084,3.71955052756395));
#21242=CARTESIAN_POINT('Ctrl Pts',(-16.7331152783245,14.02614274918,3.73064525509223));
#21243=CARTESIAN_POINT('Ctrl Pts',(-17.0692569141695,14.3926031635416,3.75139492276905));
#21244=CARTESIAN_POINT('Ctrl Pts',(-17.1983589291318,14.6030775710289,3.76026454816374));
#21245=CARTESIAN_POINT('Ctrl Pts',(-17.3641119979468,15.0459327355284,3.77963704004911));
#21246=CARTESIAN_POINT('Ctrl Pts',(-17.405,15.272129525868,3.78953191276751));
#21247=CARTESIAN_POINT('Ctrl Pts',(-17.405,15.5,3.79949999999988));
#21248=CARTESIAN_POINT('Ctrl Pts',(-17.405,15.5,3.86199999999992));
#21249=CARTESIAN_POINT('Ctrl Pts',(-17.405,15.2742109308075,3.85212296285239));
#21250=CARTESIAN_POINT('Ctrl Pts',(-17.3648553701787,15.0500311101823,3.84231632153029));
#21251=CARTESIAN_POINT('Ctrl Pts',(-17.2013040268939,14.6087211876983,3.82301142553361));
#21252=CARTESIAN_POINT('Ctrl Pts',(-17.0729962895187,14.3979574338972,3.81415369482636));
#21253=CARTESIAN_POINT('Ctrl Pts',(-16.7381842898046,14.0303834987862,3.79343004369775));
#21254=CARTESIAN_POINT('Ctrl Pts',(-16.5325589824563,13.8792948756376,3.78233550951582));
#21255=CARTESIAN_POINT('Ctrl Pts',(-16.0830251392004,13.6701864876885,3.76073175089401));
#21256=CARTESIAN_POINT('Ctrl Pts',(-15.8449545163795,13.6107769922595,3.75041329267126));
#21257=CARTESIAN_POINT('Ctrl Pts',(-15.3497889743819,13.5841913498518,3.73107301447124));
#21258=CARTESIAN_POINT('Ctrl Pts',(-15.0972352470335,13.6209853811416,3.72117335090165));
#21259=CARTESIAN_POINT('Ctrl Pts',(-14.6242311443009,13.7899391912535,3.69955871948796));
#21260=CARTESIAN_POINT('Ctrl Pts',(-14.4080235381815,13.919219244812,3.68854028964674));
#21261=CARTESIAN_POINT('Ctrl Pts',(-14.0440081901868,14.2481090815363,3.6675564113837));
#21262=CARTESIAN_POINT('Ctrl Pts',(-13.8974505145118,14.4421925951016,3.65827328980309));
#21263=CARTESIAN_POINT('Ctrl Pts',(-13.6794547169359,14.8848901646036,3.63890769183713));
#21264=CARTESIAN_POINT('Ctrl Pts',(-13.6140657478863,15.1312521894653,3.62813070037336));
#21265=CARTESIAN_POINT('Ctrl Pts',(-13.5834593005368,15.6293376228352,3.6063421862277));
#21266=CARTESIAN_POINT('Ctrl Pts',(-13.6162831343669,15.8761359329288,3.59554610967067));
#21267=CARTESIAN_POINT('Ctrl Pts',(-13.7731034757767,16.3402450791531,3.57524387230302));
#21268=CARTESIAN_POINT('Ctrl Pts',(-13.8943614984445,16.5536165703811,3.56644949459541));
#21269=CARTESIAN_POINT('Ctrl Pts',(-14.2172608701428,16.9310322330413,3.54596187910604));
#21270=CARTESIAN_POINT('Ctrl Pts',(-14.4188276118528,17.088812946621,3.53487472793943));
#21271=CARTESIAN_POINT('Ctrl Pts',(-14.8632427821596,17.3119091088748,3.51315894016867));
#21272=CARTESIAN_POINT('Ctrl Pts',(-15.1001561943329,17.3784618194619,3.50272808326872));
#21273=CARTESIAN_POINT('Ctrl Pts',(-15.5925331225056,17.4191295483254,3.48318544142854));
#21274=CARTESIAN_POINT('Ctrl Pts',(-15.8435045405407,17.3904080860209,3.4736675583809));
#21275=CARTESIAN_POINT('Ctrl Pts',(-16.3201269499146,17.2375475037393,3.4522678468467));
#21276=CARTESIAN_POINT('Ctrl Pts',(-16.5410892612555,17.1148718894886,3.44121374439588));
#21277=CARTESIAN_POINT('Ctrl Pts',(-16.916037209688,16.7969507213421,3.42005560649069));
#21278=CARTESIAN_POINT('Ctrl Pts',(-17.0687256345697,16.6073873393512,3.41044214082902));
#21279=CARTESIAN_POINT('Ctrl Pts',(-17.3004763667435,16.1715738534205,3.39137768387667));
#21280=CARTESIAN_POINT('Ctrl Pts',(-17.3735054583902,15.9274098964587,3.38069684586435));
#21281=CARTESIAN_POINT('Ctrl Pts',(-17.4022858919956,15.617489805707,3.36713953655762));
#21282=CARTESIAN_POINT('Ctrl Pts',(-17.405,15.5587111509317,3.3645682918167));
#21283=CARTESIAN_POINT('Ctrl Pts',(-17.405,15.5,3.36199999999991));
#21284=CARTESIAN_POINT('Origin',(-15.5,15.5,-1.713));
#21285=CARTESIAN_POINT('',(-17.405,15.5,2.79949999999986));
#21286=CARTESIAN_POINT('',(-17.405,15.5,2.86199999999991));
#21287=CARTESIAN_POINT('',(-17.405,15.5,-1.713));
#21288=CARTESIAN_POINT('Ctrl Pts',(-17.405,15.5,2.79949999999986));
#21289=CARTESIAN_POINT('Ctrl Pts',(-17.405,15.5944999131661,2.80363385446907));
#21290=CARTESIAN_POINT('Ctrl Pts',(-17.3979684804714,15.6890787995141,2.80777116358316));
#21291=CARTESIAN_POINT('Ctrl Pts',(-17.3463774788093,16.0325724073037,2.82279713067807));
#21292=CARTESIAN_POINT('Ctrl Pts',(-17.2596502024004,16.2722222104947,2.83306121295661));
#21293=CARTESIAN_POINT('Ctrl Pts',(-17.0030714688162,16.6952243150178,2.8520334244009));
#21294=CARTESIAN_POINT('Ctrl Pts',(-16.8389585105207,16.8765724635878,2.86221715428976));
#21295=CARTESIAN_POINT('Ctrl Pts',(-16.4440809776058,17.1736602906283,2.88367462972319));
#21296=CARTESIAN_POINT('Ctrl Pts',(-16.2148322932427,17.2836617476485,2.89476543956363));
#21297=CARTESIAN_POINT('Ctrl Pts',(-15.7321781580959,17.4067720537753,2.91574295029601));
#21298=CARTESIAN_POINT('Ctrl Pts',(-15.4840051051965,17.4207876543533,2.92476063683499));
#21299=CARTESIAN_POINT('Ctrl Pts',(-14.9971397146739,17.3537176806962,2.9446719571869));
#21300=CARTESIAN_POINT('Ctrl Pts',(-14.7629996406341,17.2736833185551,2.95529262355756));
#21301=CARTESIAN_POINT('Ctrl Pts',(-14.3294458847818,17.0244119172388,2.97716945064122));
#21302=CARTESIAN_POINT('Ctrl Pts',(-14.1361456673276,16.8542333088828,2.98821460388052));
#21303=CARTESIAN_POINT('Ctrl Pts',(-13.8361042007355,16.4585591815783,3.00823562732364));
#21304=CARTESIAN_POINT('Ctrl Pts',(-13.7280829228089,16.2400686139527,3.01712604488369));
#21305=CARTESIAN_POINT('Ctrl Pts',(-13.5977175306194,15.7680977558765,3.03777218915649));
#21306=CARTESIAN_POINT('Ctrl Pts',(-13.5790079742218,15.5183920020373,3.0486954504793));
#21307=CARTESIAN_POINT('Ctrl Pts',(-13.6388562736904,15.0216435275147,3.07042547998597));
#21308=CARTESIAN_POINT('Ctrl Pts',(-13.7185028504376,14.779600489273,3.08101353940162));
#21309=CARTESIAN_POINT('Ctrl Pts',(-13.9622301456127,14.349923249031,3.0998095691585));
#21310=CARTESIAN_POINT('Ctrl Pts',(-14.1203860318548,14.1642864361832,3.10978329125428));
#21311=CARTESIAN_POINT('Ctrl Pts',(-14.5049850693437,13.8562297834734,3.13109129051462));
#21312=CARTESIAN_POINT('Ctrl Pts',(-14.7300056668644,13.739560292438,3.14216776905116));
#21313=CARTESIAN_POINT('Ctrl Pts',(-15.2096239685188,13.6009694456039,3.16336886514782));
#21314=CARTESIAN_POINT('Ctrl Pts',(-15.4592287489489,13.5793327691483,3.1726127491432));
#21315=CARTESIAN_POINT('Ctrl Pts',(-15.9490213858857,13.6326010275756,3.19233309014878));
#21316=CARTESIAN_POINT('Ctrl Pts',(-16.1847102553598,13.7055771748497,3.2028580517407));
#21317=CARTESIAN_POINT('Ctrl Pts',(-16.62414775939,13.9411815613598,3.22465884942753));
#21318=CARTESIAN_POINT('Ctrl Pts',(-16.8218756183518,14.1049075031833,3.23573060444978));
#21319=CARTESIAN_POINT('Ctrl Pts',(-17.1339506675152,14.4910683301043,3.25599942920582));
#21320=CARTESIAN_POINT('Ctrl Pts',(-17.2488960307138,14.7068395714669,3.26480356830537));
#21321=CARTESIAN_POINT('Ctrl Pts',(-17.3765543584212,15.1206105897759,3.28290378782895));
#21322=CARTESIAN_POINT('Ctrl Pts',(-17.405,15.3099390455677,3.29118587250939));
#21323=CARTESIAN_POINT('Ctrl Pts',(-17.405,15.5,3.29949999999987));
#21324=CARTESIAN_POINT('Ctrl Pts',(-17.405,15.5,3.36199999999991));
#21325=CARTESIAN_POINT('Ctrl Pts',(-17.405,15.3121642442446,3.35378321278402));
#21326=CARTESIAN_POINT('Ctrl Pts',(-17.3772165691224,15.1250194340757,3.34559665065949));
#21327=CARTESIAN_POINT('Ctrl Pts',(-17.251673036774,14.7130224484878,3.32757403536692));
#21328=CARTESIAN_POINT('Ctrl Pts',(-17.1375440348227,14.4969355114396,3.31876388843797));
#21329=CARTESIAN_POINT('Ctrl Pts',(-16.8268793902558,14.1096485908813,3.29852386505512));
#21330=CARTESIAN_POINT('Ctrl Pts',(-16.6296619290207,13.9451577431649,3.2874547156519));
#21331=CARTESIAN_POINT('Ctrl Pts',(-16.1908952481043,13.7079383025191,3.26564400645109));
#21332=CARTESIAN_POINT('Ctrl Pts',(-15.9553778095696,13.6341302556848,3.2551073437992));
#21333=CARTESIAN_POINT('Ctrl Pts',(-15.465925329409,13.5792333586909,3.23536426723483));
#21334=CARTESIAN_POINT('Ctrl Pts',(-15.2164932530801,13.5999633821052,3.22615110516058));
#21335=CARTESIAN_POINT('Ctrl Pts',(-14.7365036590348,13.7367192091974,3.20497607910888));
#21336=CARTESIAN_POINT('Ctrl Pts',(-14.5109722524345,13.8526064231924,3.19389735931602));
#21337=CARTESIAN_POINT('Ctrl Pts',(-14.1251351188222,14.1593845568473,3.17257042028456));
#21338=CARTESIAN_POINT('Ctrl Pts',(-13.9662734753601,14.3445213777374,3.16254587149006));
#21339=CARTESIAN_POINT('Ctrl Pts',(-13.7210204081244,14.7734075803916,3.14378444530221));
#21340=CARTESIAN_POINT('Ctrl Pts',(-13.6405337707849,15.0151666662594,3.13320880725025));
#21341=CARTESIAN_POINT('Ctrl Pts',(-13.5789452302557,15.5117811349214,3.11148463976722));
#21342=CARTESIAN_POINT('Ctrl Pts',(-13.5968070574536,15.7616351175305,3.10055489424626));
#21343=CARTESIAN_POINT('Ctrl Pts',(-13.7255942596754,16.2340614020054,3.07988882755881));
#21344=CARTESIAN_POINT('Ctrl Pts',(-13.8328436761047,16.4528611452913,3.07098377759962));
#21345=CARTESIAN_POINT('Ctrl Pts',(-14.129967623663,16.8475094767687,3.05109571756475));
#21346=CARTESIAN_POINT('Ctrl Pts',(-14.3204097543996,17.0170100655722,3.04017366955205));
#21347=CARTESIAN_POINT('Ctrl Pts',(-14.7500930156158,17.2682891865639,3.01839955842826));
#21348=CARTESIAN_POINT('Ctrl Pts',(-14.9838155763777,17.3500745688595,3.00775641030031));
#21349=CARTESIAN_POINT('Ctrl Pts',(-15.4699399590987,17.4205642683659,2.98779836504272));
#21350=CARTESIAN_POINT('Ctrl Pts',(-15.7177700447031,17.4084159155821,2.9788247404591));
#21351=CARTESIAN_POINT('Ctrl Pts',(-16.2011385886972,17.2891163202623,2.95790351403087));
#21352=CARTESIAN_POINT('Ctrl Pts',(-16.4313993908793,17.1807796518502,2.94681077394374));
#21353=CARTESIAN_POINT('Ctrl Pts',(-16.8287792218349,16.8864311625419,2.92531841728524));
#21354=CARTESIAN_POINT('Ctrl Pts',(-16.9943376052565,16.7061607028033,2.91510350058699));
#21355=CARTESIAN_POINT('Ctrl Pts',(-17.2540594787777,16.2848470967839,2.89604914610767));
#21356=CARTESIAN_POINT('Ctrl Pts',(-17.3425113232036,16.0458060378014,2.88587602965012));
#21357=CARTESIAN_POINT('Ctrl Pts',(-17.3972762380981,15.6981581272708,2.8706683345263));
#21358=CARTESIAN_POINT('Ctrl Pts',(-17.405,15.599042312654,2.86633255960857));
#21359=CARTESIAN_POINT('Ctrl Pts',(-17.405,15.5000000000001,2.86199999999991));
#21360=CARTESIAN_POINT('Origin',(-15.5,15.5,-1.713));
#21361=CARTESIAN_POINT('',(-17.405,15.5,2.29949999999986));
#21362=CARTESIAN_POINT('',(-17.405,15.5,2.3619999999999));
#21363=CARTESIAN_POINT('',(-17.405,15.5,-1.713));
#21364=CARTESIAN_POINT('Ctrl Pts',(-17.405,15.5,2.29949999999986));
#21365=CARTESIAN_POINT('Ctrl Pts',(-17.405,15.6349750892016,2.30540442209967));
#21366=CARTESIAN_POINT('Ctrl Pts',(-17.3906547175841,15.7698930104027,2.31130634341201));
#21367=CARTESIAN_POINT('Ctrl Pts',(-17.3091350371661,16.1470568170573,2.32780519759638));
#21368=CARTESIAN_POINT('Ctrl Pts',(-17.2085948138019,16.3788277748054,2.33732709422014));
#21369=CARTESIAN_POINT('Ctrl Pts',(-16.9273133283528,16.7850161734643,2.35686738780469));
#21370=CARTESIAN_POINT('Ctrl Pts',(-16.751285560269,16.9569676813291,2.3672969710446));
#21371=CARTESIAN_POINT('Ctrl Pts',(-16.3359816313264,17.2304306746696,2.38901154888475));
#21372=CARTESIAN_POINT('Ctrl Pts',(-16.0985993472981,17.326183728861,2.40009884614951));
#21373=CARTESIAN_POINT('Ctrl Pts',(-15.6103272733066,17.4172942791093,2.42058927900862));
#21374=CARTESIAN_POINT('Ctrl Pts',(-15.3648986121507,17.4157081120999,2.42938395353938));
#21375=CARTESIAN_POINT('Ctrl Pts',(-14.8845200628733,17.3196284646875,2.44968403450236));
#21376=CARTESIAN_POINT('Ctrl Pts',(-14.654349264037,17.2247397227717,2.46047922828888));
#21377=CARTESIAN_POINT('Ctrl Pts',(-14.2382060120843,16.9493443709446,2.48226786799658));
#21378=CARTESIAN_POINT('Ctrl Pts',(-14.0574801656378,16.7695991333544,2.49304589918372));
#21379=CARTESIAN_POINT('Ctrl Pts',(-13.7829441267767,16.3595582698038,2.51241491124335));
#21380=CARTESIAN_POINT('Ctrl Pts',(-13.6880618743612,16.1356280757084,2.52169474734417));
#21381=CARTESIAN_POINT('Ctrl Pts',(-13.585073025739,15.6559826280725,2.54267661294504));
#21382=CARTESIAN_POINT('Ctrl Pts',(-13.5811253210558,15.4041120390609,2.55369457396917));
#21383=CARTESIAN_POINT('Ctrl Pts',(-13.6711292410151,14.9099469975137,2.57531159240956));
#21384=CARTESIAN_POINT('Ctrl Pts',(-13.7654706440895,14.6727701017159,2.585216030766));
#21385=CARTESIAN_POINT('Ctrl Pts',(-14.0359546772966,14.2571304573011,2.60455399517033));
#21386=CARTESIAN_POINT('Ctrl Pts',(-14.206376233983,14.0806094442151,2.61487113882675));
#21387=CARTESIAN_POINT('Ctrl Pts',(-14.6121268718779,13.7957288906123,2.63647352888887));
#21388=CARTESIAN_POINT('Ctrl Pts',(-14.8457425680365,13.6931198901864,2.64756808828558));
#21389=CARTESIAN_POINT('Ctrl Pts',(-15.3314469326937,13.586779428234,2.66829435904228));
#21390=CARTESIAN_POINT('Ctrl Pts',(-15.5781422579797,13.5809598700289,2.6771532421492));
#21391=CARTESIAN_POINT('Ctrl Pts',(-16.0616840103632,13.6631481801623,2.69726932248259));
#21392=CARTESIAN_POINT('Ctrl Pts',(-16.293876506192,13.7509258641659,2.70798557103718));
#21393=CARTESIAN_POINT('Ctrl Pts',(-16.7175546481377,14.0132918520873,2.72977467986982));
#21394=CARTESIAN_POINT('Ctrl Pts',(-16.9036363424498,14.1875346364906,2.74063526021344));
#21395=CARTESIAN_POINT('Ctrl Pts',(-17.1904876517898,14.589264042189,2.76028903203523));
#21396=CARTESIAN_POINT('Ctrl Pts',(-17.2920941372137,14.8103627739561,2.76933214234265));
#21397=CARTESIAN_POINT('Ctrl Pts',(-17.3865337341854,15.1939311843254,2.78611116291874));
#21398=CARTESIAN_POINT('Ctrl Pts',(-17.405,15.3468618982312,2.7928010454168));
#21399=CARTESIAN_POINT('Ctrl Pts',(-17.405,15.5,2.79949999999986));
#21400=CARTESIAN_POINT('Ctrl Pts',(-17.405,15.5000000000001,2.86199999999991));
#21401=CARTESIAN_POINT('Ctrl Pts',(-17.405,15.3512516229631,2.85549307187056));
#21402=CARTESIAN_POINT('Ctrl Pts',(-17.3875773407963,15.2026690372746,2.84899339620625));
#21403=CARTESIAN_POINT('Ctrl Pts',(-17.2968195960562,14.8227897877569,2.83237575624485));
#21404=CARTESIAN_POINT('Ctrl Pts',(-17.1967725884005,14.6010434309328,2.8232847717177));
#21405=CARTESIAN_POINT('Ctrl Pts',(-16.9127711516358,14.197373883066,2.80369652880942));
#21406=CARTESIAN_POINT('Ctrl Pts',(-16.7279167244992,14.0218399237571,2.79285420118227));
#21407=CARTESIAN_POINT('Ctrl Pts',(-16.3059501787976,13.7564329807281,2.7710634216705));
#21408=CARTESIAN_POINT('Ctrl Pts',(-16.0742075216153,13.6670024169188,2.76032806252068));
#21409=CARTESIAN_POINT('Ctrl Pts',(-15.5913913266025,13.5815869421211,2.74016888370885));
#21410=CARTESIAN_POINT('Ctrl Pts',(-15.3449980770684,13.5856759097506,2.73133186536444));
#21411=CARTESIAN_POINT('Ctrl Pts',(-14.8586778930605,13.6884627347192,2.71065999107711));
#21412=CARTESIAN_POINT('Ctrl Pts',(-14.6241660972474,13.789483754856,2.69956621667948));
#21413=CARTESIAN_POINT('Ctrl Pts',(-14.2161583938901,14.0717277875137,2.67793598691674));
#21414=CARTESIAN_POINT('Ctrl Pts',(-14.0444178943956,14.2471981421006,2.66759185687674));
#21415=CARTESIAN_POINT('Ctrl Pts',(-13.7714012327442,14.6606332321423,2.64820616529025));
#21416=CARTESIAN_POINT('Ctrl Pts',(-13.6755976023477,14.8965330213078,2.63839838052026));
#21417=CARTESIAN_POINT('Ctrl Pts',(-13.5818831565501,15.3895650821121,2.61683092379216));
#21418=CARTESIAN_POINT('Ctrl Pts',(-13.5839352941782,15.641650445142,2.60580356757912));
#21419=CARTESIAN_POINT('Ctrl Pts',(-13.6834194236602,16.122242903278,2.58478027544718));
#21420=CARTESIAN_POINT('Ctrl Pts',(-13.776655110423,16.3468820683731,2.57543042080797));
#21421=CARTESIAN_POINT('Ctrl Pts',(-14.0481663058559,16.7589361605946,2.55613196766852));
#21422=CARTESIAN_POINT('Ctrl Pts',(-14.2275563446959,16.940001960658,2.54537565835736));
#21423=CARTESIAN_POINT('Ctrl Pts',(-14.6417946261065,17.218552411423,2.52359017715421));
#21424=CARTESIAN_POINT('Ctrl Pts',(-14.8714381905177,17.315174747068,2.51277703942813));
#21425=CARTESIAN_POINT('Ctrl Pts',(-15.3510290654114,17.4146453191073,2.49243263141847));
#21426=CARTESIAN_POINT('Ctrl Pts',(-15.5961612290483,17.4180226750135,2.48364187534089));
#21427=CARTESIAN_POINT('Ctrl Pts',(-16.0850284715075,17.3306030497403,2.4632096240861));
#21428=CARTESIAN_POINT('Ctrl Pts',(-16.3232942738259,17.2365307721866,2.45212561811769));
#21429=CARTESIAN_POINT('Ctrl Pts',(-16.7408656001719,16.9658803597754,2.43038665999374));
#21430=CARTESIAN_POINT('Ctrl Pts',(-16.9182333572259,16.7950621087425,2.41993109967277));
#21431=CARTESIAN_POINT('Ctrl Pts',(-17.2021096654342,16.3911655021351,2.40034263083006));
#21432=CARTESIAN_POINT('Ctrl Pts',(-17.3041266818208,16.1606781246921,2.39090105532342));
#21433=CARTESIAN_POINT('Ctrl Pts',(-17.3895750341878,15.7798334598907,2.3742411837223));
#21434=CARTESIAN_POINT('Ctrl Pts',(-17.405,15.6399618896503,2.36812256735118));
#21435=CARTESIAN_POINT('Ctrl Pts',(-17.405,15.5,2.3619999999999));
#21436=CARTESIAN_POINT('Origin',(-15.5,15.5,-1.713));
#21437=CARTESIAN_POINT('',(-17.405,15.5,1.79949999999985));
#21438=CARTESIAN_POINT('',(-17.405,15.5,1.86199999999989));
#21439=CARTESIAN_POINT('',(-17.405,15.5,-1.713));
#21440=CARTESIAN_POINT('Ctrl Pts',(-17.405,15.5,1.79949999999985));
#21441=CARTESIAN_POINT('Ctrl Pts',(-17.405,15.6758129035626,1.80719085317407));
#21442=CARTESIAN_POINT('Ctrl Pts',(-17.3806596497542,15.8511550139008,1.81486111171898));
#21443=CARTESIAN_POINT('Ctrl Pts',(-17.2650749842631,16.2577005203566,1.83264525460857));
#21444=CARTESIAN_POINT('Ctrl Pts',(-17.1525410716862,16.4791337298434,1.84164454575853));
#21445=CARTESIAN_POINT('Ctrl Pts',(-16.8499756822054,16.8662860371983,1.86157479367078));
#21446=CARTESIAN_POINT('Ctrl Pts',(-16.6630641861499,17.0285411759165,1.87220461314595));
#21447=CARTESIAN_POINT('Ctrl Pts',(-16.2295355547136,17.2781584906455,1.8940880543295));
#21448=CARTESIAN_POINT('Ctrl Pts',(-15.9851780470513,17.3597553999023,1.90512997313393));
#21449=CARTESIAN_POINT('Ctrl Pts',(-15.4922789879605,17.4202338148899,1.92512569991292));
#21450=CARTESIAN_POINT('Ctrl Pts',(-15.2491564026104,17.4037967993866,1.93402924444523));
#21451=CARTESIAN_POINT('Ctrl Pts',(-14.7755901589679,17.279275854445,1.95469332449074));
#21452=CARTESIAN_POINT('Ctrl Pts',(-14.5502497144695,17.1698983391235,1.96562242803827));
#21453=CARTESIAN_POINT('Ctrl Pts',(-14.1508645276189,16.8683975242138,1.98734719291853));
#21454=CARTESIAN_POINT('Ctrl Pts',(-13.981671743571,16.6778728715177,1.99792407723483));
#21455=CARTESIAN_POINT('Ctrl Pts',(-13.7327272831338,16.2511267747944,2.01668896241555));
#21456=CARTESIAN_POINT('Ctrl Pts',(-13.6517464023149,16.0210162929489,2.02670838613501));
#21457=CARTESIAN_POINT('Ctrl Pts',(-13.5788147179765,15.5335256561171,2.04803343586519));
#21458=CARTESIAN_POINT('Ctrl Pts',(-13.5911258922105,15.280271092335,2.05911193821786));
#21459=CARTESIAN_POINT('Ctrl Pts',(-13.7125093691987,14.7961503166125,2.08028957495113));
#21460=CARTESIAN_POINT('Ctrl Pts',(-13.819202861008,14.5697105895712,2.08950576046523));
#21461=CARTESIAN_POINT('Ctrl Pts',(-14.1113472156176,14.1731698218157,2.10924656608824));
#21462=CARTESIAN_POINT('Ctrl Pts',(-14.2929621670787,14.0060531995224,2.11978206358689));
#21463=CARTESIAN_POINT('Ctrl Pts',(-14.7176774141026,13.7445407599599,2.1415917929429));
#21464=CARTESIAN_POINT('Ctrl Pts',(-14.9586987854945,13.6559083064524,2.15266120926984));
#21465=CARTESIAN_POINT('Ctrl Pts',(-15.4494045149217,13.5803297812339,2.17290411784708));
#21466=CARTESIAN_POINT('Ctrl Pts',(-15.6936192208834,13.5894481237492,2.18171361442766));
#21467=CARTESIAN_POINT('Ctrl Pts',(-16.1706231028332,13.6998629991341,2.2021993938312));
#21468=CARTESIAN_POINT('Ctrl Pts',(-16.3984748931021,13.8020710132237,2.21306682365253));
#21469=CARTESIAN_POINT('Ctrl Pts',(-16.8063914917534,14.0907294601935,2.23483389979174));
#21470=CARTESIAN_POINT('Ctrl Pts',(-16.9813964057174,14.2759936634906,2.24551591216831));
#21471=CARTESIAN_POINT('Ctrl Pts',(-17.2430957761371,14.6945050877789,2.26458389183068));
#21472=CARTESIAN_POINT('Ctrl Pts',(-17.3309992678079,14.9214828069085,2.27419303617254));
#21473=CARTESIAN_POINT('Ctrl Pts',(-17.3947425846049,15.2716869136996,2.28951255090531));
#21474=CARTESIAN_POINT('Ctrl Pts',(-17.405,15.3858638959536,2.29450716955163));
#21475=CARTESIAN_POINT('Ctrl Pts',(-17.405,15.5,2.29949999999986));
#21476=CARTESIAN_POINT('Ctrl Pts',(-17.405,15.5,2.3619999999999));
#21477=CARTESIAN_POINT('Ctrl Pts',(-17.405,15.3906515670809,2.35721660398419));
#21478=CARTESIAN_POINT('Ctrl Pts',(-17.3955851122864,15.2812480043357,2.35243079634019));
#21479=CARTESIAN_POINT('Ctrl Pts',(-17.3352956387922,14.935218870948,2.33729391386478));
#21480=CARTESIAN_POINT('Ctrl Pts',(-17.2490540991717,14.707498955458,2.32759382153132));
#21481=CARTESIAN_POINT('Ctrl Pts',(-16.9904162426923,14.286994913319,2.3085982408156));
#21482=CARTESIAN_POINT('Ctrl Pts',(-16.8167952691443,14.100447590647,2.29794059273781));
#21483=CARTESIAN_POINT('Ctrl Pts',(-16.4108947458734,13.808675505369,2.27618179102299));
#21484=CARTESIAN_POINT('Ctrl Pts',(-16.1836271957613,13.7047368876666,2.26529864226079));
#21485=CARTESIAN_POINT('Ctrl Pts',(-15.7074406505977,13.5909239280283,2.24476950294009));
#21486=CARTESIAN_POINT('Ctrl Pts',(-15.4634983903644,13.5800347208373,2.23594450211546));
#21487=CARTESIAN_POINT('Ctrl Pts',(-14.9722466215299,13.6519590091507,2.21576083389054));
#21488=CARTESIAN_POINT('Ctrl Pts',(-14.7303994517394,13.7388986235731,2.2046971593462));
#21489=CARTESIAN_POINT('Ctrl Pts',(-14.3035204103725,13.9975567011301,2.1828678884387));
#21490=CARTESIAN_POINT('Ctrl Pts',(-14.1206111259464,14.163511083443,2.17230877741255));
#21491=CARTESIAN_POINT('Ctrl Pts',(-13.8259323840979,14.5577807002497,2.15252163459544));
#21492=CARTESIAN_POINT('Ctrl Pts',(-13.7178134794438,14.7829929281575,2.14336513875066));
#21493=CARTESIAN_POINT('Ctrl Pts',(-13.5928113341082,15.2658892729356,2.12224106417595));
#21494=CARTESIAN_POINT('Ctrl Pts',(-13.5785939146864,15.5192387751817,2.1111584087846));
#21495=CARTESIAN_POINT('Ctrl Pts',(-13.6479843183902,16.0075214670508,2.08979871097755));
#21496=CARTESIAN_POINT('Ctrl Pts',(-13.7273296613187,16.23837962393,2.07969992896183));
#21497=CARTESIAN_POINT('Ctrl Pts',(-13.973326260038,16.6670166536837,2.06094940272588));
#21498=CARTESIAN_POINT('Ctrl Pts',(-14.1411412929859,16.8587584931067,2.05042637418511));
#21499=CARTESIAN_POINT('Ctrl Pts',(-14.5385852068307,17.1632354950527,2.02871005629614));
#21500=CARTESIAN_POINT('Ctrl Pts',(-14.763317098085,17.274253239104,2.01776813158519));
#21501=CARTESIAN_POINT('Ctrl Pts',(-15.2360771136105,17.4020132521351,1.99706374882692));
#21502=CARTESIAN_POINT('Ctrl Pts',(-15.4789633995476,17.4201194492865,1.98812764457752));
#21503=CARTESIAN_POINT('Ctrl Pts',(-15.9695743949547,17.363402239757,1.96830086460536));
#21504=CARTESIAN_POINT('Ctrl Pts',(-16.2121100361483,17.2848386351519,1.95739431041028));
#21505=CARTESIAN_POINT('Ctrl Pts',(-16.6463290172403,17.0411728993748,1.93561489062376));
#21506=CARTESIAN_POINT('Ctrl Pts',(-16.8351927338306,16.8807820766524,1.92495189028335));
#21507=CARTESIAN_POINT('Ctrl Pts',(-17.1416354883154,16.4971568914956,1.90495189891119));
#21508=CARTESIAN_POINT('Ctrl Pts',(-17.2563300345455,16.2775586051926,1.89601393723492));
#21509=CARTESIAN_POINT('Ctrl Pts',(-17.3785616890088,15.8658792821985,1.87800521794384));
#21510=CARTESIAN_POINT('Ctrl Pts',(-17.405,15.683232457912,1.87001541810628));
#21511=CARTESIAN_POINT('Ctrl Pts',(-17.405,15.5,1.86199999999989));
#21512=CARTESIAN_POINT('Origin',(-15.5,15.5,11.20575));
#21513=CARTESIAN_POINT('',(-15.5,13.5679367061317,1.22137499999989));
#21514=CARTESIAN_POINT('',(-15.5,13.5679367061317,1.3858));
#21515=CARTESIAN_POINT('',(-15.5,13.5679367061317,11.20575));
#21516=CARTESIAN_POINT('',(-17.2021646372135,16.4140591443298,1.3857999999999));
#21517=CARTESIAN_POINT('Origin',(-15.5,15.5,1.3858));
#21518=CARTESIAN_POINT('Ctrl Pts',(-17.2021646372131,16.4140591443306,1.38579999999995));
#21519=CARTESIAN_POINT('Ctrl Pts',(-17.2835044921692,16.2625877372984,1.3792667682509));
#21520=CARTESIAN_POINT('Ctrl Pts',(-17.3442533198926,16.1009564770173,1.37229532392361));
#21521=CARTESIAN_POINT('Ctrl Pts',(-17.4225863575886,15.7606826337724,1.35761870660277));
#21522=CARTESIAN_POINT('Ctrl Pts',(-17.4383899414388,15.583279243606,1.3499669822032));
#21523=CARTESIAN_POINT('Ctrl Pts',(-17.4173618065871,15.150545952148,1.33130242409274));
#21524=CARTESIAN_POINT('Ctrl Pts',(-17.354246909013,14.8998465932948,1.32048931393011));
#21525=CARTESIAN_POINT('Ctrl Pts',(-17.1389102320616,14.4480453999454,1.30100232322681));
#21526=CARTESIAN_POINT('Ctrl Pts',(-16.9927945769671,14.2493134357546,1.29183017937045));
#21527=CARTESIAN_POINT('Ctrl Pts',(-16.6281426362718,13.9112799548102,1.27091926226126));
#21528=CARTESIAN_POINT('Ctrl Pts',(-16.410884372517,13.7774947329751,1.25991876919078));
#21529=CARTESIAN_POINT('Ctrl Pts',(-15.9581594815713,13.6089622530652,1.23937348400477));
#21530=CARTESIAN_POINT('Ctrl Pts',(-15.7298816359758,13.5679367061317,1.22996181912958));
#21531=CARTESIAN_POINT('Ctrl Pts',(-15.5,13.5679367061317,1.22137499999989));
#21532=CARTESIAN_POINT('Origin',(-15.5,15.5,11.20575));
#21533=CARTESIAN_POINT('',(-15.5,13.5679367061317,0.721374999999882));
#21534=CARTESIAN_POINT('',(-15.5,13.5679367061317,1.19012499999984));
#21535=CARTESIAN_POINT('',(-15.5,13.5679367061317,11.20575));
#21536=CARTESIAN_POINT('',(-16.7089831815964,17.0070594673503,1.3858));
#21537=CARTESIAN_POINT('Ctrl Pts',(-15.5,13.5679367061317,1.19012499999984));
#21538=CARTESIAN_POINT('Ctrl Pts',(-15.6209597157618,13.5679367061317,1.19464323477234));
#21539=CARTESIAN_POINT('Ctrl Pts',(-15.7419184750194,13.5792946957063,1.19940637898293));
#21540=CARTESIAN_POINT('Ctrl Pts',(-16.1137167329605,13.6500674067386,1.21482051737712));
#21541=CARTESIAN_POINT('Ctrl Pts',(-16.3540308512701,13.7479960405399,1.22590894156164));
#21542=CARTESIAN_POINT('Ctrl Pts',(-16.7741136008819,14.026702340501,1.24761093429799));
#21543=CARTESIAN_POINT('Ctrl Pts',(-16.9519823816307,14.2016401214962,1.258027594988));
#21544=CARTESIAN_POINT('Ctrl Pts',(-17.2359894885833,14.6147032779413,1.27754424976214));
#21545=CARTESIAN_POINT('Ctrl Pts',(-17.3372359040119,14.8503902891215,1.28710617538617));
#21546=CARTESIAN_POINT('Ctrl Pts',(-17.4426537117389,15.3471703745469,1.30853318586947));
#21547=CARTESIAN_POINT('Ctrl Pts',(-17.4459126157984,15.6033601229582,1.31958310631912));
#21548=CARTESIAN_POINT('Ctrl Pts',(-17.357744835181,16.0780177664297,1.34005593645267));
#21549=CARTESIAN_POINT('Ctrl Pts',(-17.2762233318702,16.2939199281608,1.34923226468177));
#21550=CARTESIAN_POINT('Ctrl Pts',(-17.0408566361002,16.6881134566224,1.36652510317405));
#21551=CARTESIAN_POINT('Ctrl Pts',(-16.8884973676933,16.8630507957942,1.37598889193056));
#21552=CARTESIAN_POINT('Ctrl Pts',(-16.7089831815964,17.0070594673503,1.38579999999999));
#21553=CARTESIAN_POINT('Origin',(-15.5,15.5,1.3858));
#21554=CARTESIAN_POINT('Ctrl Pts',(-15.5,13.5679367061317,1.22137499999989));
#21555=CARTESIAN_POINT('Ctrl Pts',(-15.4729341637143,13.5679367061317,1.22036400388534));
#21556=CARTESIAN_POINT('Ctrl Pts',(-15.4458469977579,13.5685054395913,1.2193399457951));
#21557=CARTESIAN_POINT('Ctrl Pts',(-15.1726369387374,13.5800041737923,1.20888669013352));
#21558=CARTESIAN_POINT('Ctrl Pts',(-14.9307787644431,13.6373364196089,1.19861608777127));
#21559=CARTESIAN_POINT('Ctrl Pts',(-14.4729009299767,13.8436681823131,1.17706314833877));
#21560=CARTESIAN_POINT('Ctrl Pts',(-14.2627623231917,13.9941383691091,1.16596877123743));
#21561=CARTESIAN_POINT('Ctrl Pts',(-13.9183617245921,14.3628583035511,1.14515252623231));
#21562=CARTESIAN_POINT('Ctrl Pts',(-13.7853340431921,14.5755603823523,1.13624772831502));
#21563=CARTESIAN_POINT('Ctrl Pts',(-13.6069662800139,15.0402511769473,1.11620478613719));
#21564=CARTESIAN_POINT('Ctrl Pts',(-13.563518985263,15.2879321565451,1.10552186405143));
#21565=CARTESIAN_POINT('Ctrl Pts',(-13.5731954041822,15.7929752639186,1.08373845470453));
#21566=CARTESIAN_POINT('Ctrl Pts',(-13.628926931347,16.0454493143052,1.07284879893307));
#21567=CARTESIAN_POINT('Ctrl Pts',(-13.8310245097158,16.5036338505738,1.05308648327279));
#21568=CARTESIAN_POINT('Ctrl Pts',(-13.9714260897244,16.7067442547807,1.0441143077112));
#21569=CARTESIAN_POINT('Ctrl Pts',(-14.3257784403693,17.0548537163586,1.02337081594498));
#21570=CARTESIAN_POINT('Ctrl Pts',(-14.5383567467269,17.1945806683055,1.01241699564406));
#21571=CARTESIAN_POINT('Ctrl Pts',(-15.0088443360005,17.3860429606324,0.990713714656131));
#21572=CARTESIAN_POINT('Ctrl Pts',(-15.2627143703035,17.4344332046964,0.980289491368659));
#21573=CARTESIAN_POINT('Ctrl Pts',(-15.764107690538,17.4296140644544,0.961456907738265));
#21574=CARTESIAN_POINT('Ctrl Pts',(-16.0069337839783,17.3804673298746,0.951326678324261));
#21575=CARTESIAN_POINT('Ctrl Pts',(-16.4699471299709,17.1903012304531,0.929930537938738));
#21576=CARTESIAN_POINT('Ctrl Pts',(-16.6843681043685,17.0476412723927,0.918844635164113));
#21577=CARTESIAN_POINT('Ctrl Pts',(-17.0422253707064,16.6904570711204,0.897774518665517));
#21578=CARTESIAN_POINT('Ctrl Pts',(-17.1834288053771,16.4806668481729,0.888672908979973));
#21579=CARTESIAN_POINT('Ctrl Pts',(-17.3770350149237,16.0208578484158,0.868840527314208));
#21580=CARTESIAN_POINT('Ctrl Pts',(-17.42837351161,15.7755220883528,0.858258758726811));
#21581=CARTESIAN_POINT('Ctrl Pts',(-17.4355092606312,15.2690019284845,0.836411641473291));
#21582=CARTESIAN_POINT('Ctrl Pts',(-17.3873412235869,15.0126438266187,0.825354459639089));
#21583=CARTESIAN_POINT('Ctrl Pts',(-17.1979533839632,14.5460700127244,0.805230299482811));
#21584=CARTESIAN_POINT('Ctrl Pts',(-17.063281790105,14.3384565933621,0.796385555323458));
#21585=CARTESIAN_POINT('Ctrl Pts',(-16.7193021674531,13.9803614873582,0.775814169018619));
#21586=CARTESIAN_POINT('Ctrl Pts',(-16.5115619839701,13.8348471766509,0.764916258632763));
#21587=CARTESIAN_POINT('Ctrl Pts',(-16.0477927715656,13.6296318245785,0.743167333659146));
#21588=CARTESIAN_POINT('Ctrl Pts',(-15.7954972631553,13.5735885359089,0.732534660777732));
#21589=CARTESIAN_POINT('Ctrl Pts',(-15.5263956112966,13.568071880497,0.722363876209219));
#21590=CARTESIAN_POINT('Ctrl Pts',(-15.5131950985184,13.5679367061317,0.721867879406689));
#21591=CARTESIAN_POINT('Ctrl Pts',(-15.5,13.5679367061317,0.721374999999882));
#21592=CARTESIAN_POINT('Origin',(-15.5,15.5,11.20575));
#21593=CARTESIAN_POINT('',(-15.5000000000001,13.5679367061317,0.22137499999988));
#21594=CARTESIAN_POINT('',(-15.5,13.5679367061317,0.69012499999983));
#21595=CARTESIAN_POINT('',(-15.5,13.5679367061317,11.20575));
#21596=CARTESIAN_POINT('Ctrl Pts',(-15.5,13.5679367061317,0.690124999999832));
#21597=CARTESIAN_POINT('Ctrl Pts',(-15.663197634803,13.5679367061317,0.696220957019179));
#21598=CARTESIAN_POINT('Ctrl Pts',(-15.8260698424807,13.5886111528802,0.702750621155672));
#21599=CARTESIAN_POINT('Ctrl Pts',(-16.2318407735952,13.6937750358444,0.720175424526367));
#21600=CARTESIAN_POINT('Ctrl Pts',(-16.4638288993578,13.8061679673983,0.731264781557265));
#21601=CARTESIAN_POINT('Ctrl Pts',(-16.8630470507188,14.108833797682,0.75270412300508));
#21602=CARTESIAN_POINT('Ctrl Pts',(-17.028761444196,14.2932884830899,0.762872018728106));
#21603=CARTESIAN_POINT('Ctrl Pts',(-17.2874053587738,14.7231251438683,0.781803012187292));
#21604=CARTESIAN_POINT('Ctrl Pts',(-17.3745003706305,14.9664736216104,0.79211305640892));
#21605=CARTESIAN_POINT('Ctrl Pts',(-17.4482099203794,15.4692792372004,0.813799958747375));
#21606=CARTESIAN_POINT('Ctrl Pts',(-17.4355847239787,15.723565875171,0.824767794651858));
#21607=CARTESIAN_POINT('Ctrl Pts',(-17.3151733744223,16.2055976541615,0.845558684393085));
#21608=CARTESIAN_POINT('Ctrl Pts',(-17.2113496874164,16.4295122772777,0.854579673980927));
#21609=CARTESIAN_POINT('Ctrl Pts',(-16.9190154733788,16.8359718966524,0.874264961849426));
#21610=CARTESIAN_POINT('Ctrl Pts',(-16.7296891979234,17.0120418978351,0.885134014187554));
#21611=CARTESIAN_POINT('Ctrl Pts',(-16.2991617620683,17.2766178136154,0.906921415251217));
#21612=CARTESIAN_POINT('Ctrl Pts',(-16.0634585876014,17.3648212635817,0.917627873583943));
#21613=CARTESIAN_POINT('Ctrl Pts',(-15.5727030691474,17.4465792698414,0.93772235628183));
#21614=CARTESIAN_POINT('Ctrl Pts',(-15.3223565583377,17.4398199793547,0.946593274573898));
#21615=CARTESIAN_POINT('Ctrl Pts',(-14.8300711076984,17.3302144103329,0.967345462670996));
#21616=CARTESIAN_POINT('Ctrl Pts',(-14.5935881752468,17.2253688342268,0.978439949755269));
#21617=CARTESIAN_POINT('Ctrl Pts',(-14.1832015334446,16.9351538432142,1.00002795682994));
#21618=CARTESIAN_POINT('Ctrl Pts',(-14.0110153602745,16.755615830377,1.01033156193278));
#21619=CARTESIAN_POINT('Ctrl Pts',(-13.7379425524706,16.3329965553295,1.02964587164791));
#21620=CARTESIAN_POINT('Ctrl Pts',(-13.6429845085471,16.0918227958046,1.03959862802551));
#21621=CARTESIAN_POINT('Ctrl Pts',(-13.5535333316269,15.5900949475556,1.06123904433767));
#21622=CARTESIAN_POINT('Ctrl Pts',(-13.5584675814187,15.3347633934782,1.07225194933617));
#21623=CARTESIAN_POINT('Ctrl Pts',(-13.6646353766633,14.8487842127048,1.09321309755165));
#21624=CARTESIAN_POINT('Ctrl Pts',(-13.761672278608,14.6220240391691,1.10246053097514));
#21625=CARTESIAN_POINT('Ctrl Pts',(-14.041585270235,14.2071591450873,1.12186311344001));
#21626=CARTESIAN_POINT('Ctrl Pts',(-14.2255255819044,14.0255156909769,1.13265117917155));
#21627=CARTESIAN_POINT('Ctrl Pts',(-14.648495420734,13.74776419308,1.1544404228268));
#21628=CARTESIAN_POINT('Ctrl Pts',(-14.8821830753995,13.6523788496886,1.16522647893842));
#21629=CARTESIAN_POINT('Ctrl Pts',(-15.2505243179915,13.5800170676889,1.18054575641211));
#21630=CARTESIAN_POINT('Ctrl Pts',(-15.3752528162562,13.5679367061317,1.18546529110574));
#21631=CARTESIAN_POINT('Ctrl Pts',(-15.5,13.5679367061317,1.19012499999984));
#21632=CARTESIAN_POINT('Ctrl Pts',(-15.5,13.5679367061317,0.721374999999882));
#21633=CARTESIAN_POINT('Ctrl Pts',(-15.2685828063486,13.5679367061317,0.712730822847808));
#21634=CARTESIAN_POINT('Ctrl Pts',(-15.0388969708039,13.6095133452991,0.703254680220421));
#21635=CARTESIAN_POINT('Ctrl Pts',(-14.5838672575743,13.7800568344395,0.682579933296358));
#21636=CARTESIAN_POINT('Ctrl Pts',(-14.3657373188852,13.9154007888411,0.67151326490416));
#21637=CARTESIAN_POINT('Ctrl Pts',(-13.9955563283149,14.2617096427834,0.650217354190035));
#21638=CARTESIAN_POINT('Ctrl Pts',(-13.8467023152938,14.4688321611842,0.640851106713065));
#21639=CARTESIAN_POINT('Ctrl Pts',(-13.6392165648734,14.9240794292194,0.621215480666726));
#21640=CARTESIAN_POINT('Ctrl Pts',(-13.5807974420006,15.1670698897687,0.610734869027327));
#21641=CARTESIAN_POINT('Ctrl Pts',(-13.5584324818228,15.6716078298641,0.588973248445474));
#21642=CARTESIAN_POINT('Ctrl Pts',(-13.598542278736,15.9284928588798,0.577893339304166));
#21643=CARTESIAN_POINT('Ctrl Pts',(-13.773173526214,16.4008511610958,0.557519683857022));
#21644=CARTESIAN_POINT('Ctrl Pts',(-13.9018579853462,16.6132862458172,0.54872840560789));
#21645=CARTESIAN_POINT('Ctrl Pts',(-14.2349802267053,16.9816699616753,0.528340694405922));
#21646=CARTESIAN_POINT('Ctrl Pts',(-14.4375333639109,17.1330265345501,0.517510543306561));
#21647=CARTESIAN_POINT('Ctrl Pts',(-14.8940137700958,17.3523384610088,0.495729873520459));
#21648=CARTESIAN_POINT('Ctrl Pts',(-15.1444779567369,17.4162475185621,0.484995974086985));
#21649=CARTESIAN_POINT('Ctrl Pts',(-15.644292945993,17.4421185607808,0.465768343173262));
#21650=CARTESIAN_POINT('Ctrl Pts',(-15.8886689106846,17.4083000037079,0.456344488469386));
#21651=CARTESIAN_POINT('Ctrl Pts',(-16.3602738338657,17.2484328206968,0.435280848151098));
#21652=CARTESIAN_POINT('Ctrl Pts',(-16.5819407282909,17.1206457359146,0.424245033703684));
#21653=CARTESIAN_POINT('Ctrl Pts',(-16.9645889726516,16.7856687238997,0.402727812195782));
#21654=CARTESIAN_POINT('Ctrl Pts',(-17.1213576046383,16.5812682862177,0.393012028302294));
#21655=CARTESIAN_POINT('Ctrl Pts',(-17.3428309783919,16.130730045467,0.373579510995516));
#21656=CARTESIAN_POINT('Ctrl Pts',(-17.4082697839647,15.8902976976571,0.363209235317829));
#21657=CARTESIAN_POINT('Ctrl Pts',(-17.4458200822696,15.3881980765453,0.341552783779496));
#21658=CARTESIAN_POINT('Ctrl Pts',(-17.4137884813012,15.1310281688062,0.330460587311118));
#21659=CARTESIAN_POINT('Ctrl Pts',(-17.2540504948445,14.6530287775216,0.309843621638471));
#21660=CARTESIAN_POINT('Ctrl Pts',(-17.1313390172738,14.4356759590614,0.301024334102504));
#21661=CARTESIAN_POINT('Ctrl Pts',(-16.8090342643691,14.0571971876884,0.280822982049281));
#21662=CARTESIAN_POINT('Ctrl Pts',(-16.6117620423532,13.9002426534532,0.27006936510708));
#21663=CARTESIAN_POINT('Ctrl Pts',(-16.1629040887197,13.6672548471105,0.248278485924882));
#21664=CARTESIAN_POINT('Ctrl Pts',(-15.9144966796287,13.5956339334636,0.237455100705018));
#21665=CARTESIAN_POINT('Ctrl Pts',(-15.6062624045507,13.5701259723312,0.225391456362187));
#21666=CARTESIAN_POINT('Ctrl Pts',(-15.5531033073173,13.5679367061317,0.223358579476269));
#21667=CARTESIAN_POINT('Ctrl Pts',(-15.5000000000001,13.5679367061317,0.221374999999879));
#21668=CARTESIAN_POINT('Origin',(-15.5,15.5,11.20575));
#21669=CARTESIAN_POINT('',(-15.5,13.5679367061317,-0.278625000000132));
#21670=CARTESIAN_POINT('',(-15.4999999999999,13.5679367061317,0.190124999999821));
#21671=CARTESIAN_POINT('',(-15.5,13.5679367061317,11.20575));
#21672=CARTESIAN_POINT('Ctrl Pts',(-15.4999999999999,13.5679367061317,0.190124999999821));
#21673=CARTESIAN_POINT('Ctrl Pts',(-15.7052232055908,13.5679367061317,0.197790747375166));
#21674=CARTESIAN_POINT('Ctrl Pts',(-15.9094431243975,13.6006312438211,0.206124105599975));
#21675=CARTESIAN_POINT('Ctrl Pts',(-16.3458500952319,13.7445092392223,0.225528168010864));
#21676=CARTESIAN_POINT('Ctrl Pts',(-16.5687690248994,13.8706006648951,0.236574181605322));
#21677=CARTESIAN_POINT('Ctrl Pts',(-16.9462938014503,14.1957983248931,0.257689124656267));
#21678=CARTESIAN_POINT('Ctrl Pts',(-17.0996068020759,14.3891741439698,0.267213101031684));
#21679=CARTESIAN_POINT('Ctrl Pts',(-17.3312210666002,14.8328987043052,0.286351732158294));
#21680=CARTESIAN_POINT('Ctrl Pts',(-17.403389189678,15.0810963874238,0.297056940587811));
#21681=CARTESIAN_POINT('Ctrl Pts',(-17.4463663432178,15.5859112111088,0.318830503652368));
#21682=CARTESIAN_POINT('Ctrl Pts',(-17.4188098289701,15.8374917549287,0.329681620893123));
#21683=CARTESIAN_POINT('Ctrl Pts',(-17.2705600347068,16.3114416099335,0.350123922848633));
#21684=CARTESIAN_POINT('Ctrl Pts',(-17.1530549287722,16.5299161239957,0.358922469304659));
#21685=CARTESIAN_POINT('Ctrl Pts',(-16.8349526369196,16.9202726297615,0.379222999836067));
#21686=CARTESIAN_POINT('Ctrl Pts',(-16.6338441663768,17.085451210082,0.390297271892839));
#21687=CARTESIAN_POINT('Ctrl Pts',(-16.1874197433205,17.3225641667436,0.412086213416755));
#21688=CARTESIAN_POINT('Ctrl Pts',(-15.9481982603318,17.3956324394973,0.422597688314654));
#21689=CARTESIAN_POINT('Ctrl Pts',(-15.4510757841914,17.4478128352924,0.442292129851002));
#21690=CARTESIAN_POINT('Ctrl Pts',(-15.1977325915627,17.4248413113895,0.451571409240313));
#21691=CARTESIAN_POINT('Ctrl Pts',(-14.7117348553567,17.2822086107985,0.472800990486173));
#21692=CARTESIAN_POINT('Ctrl Pts',(-14.4841033890512,17.1630032804563,0.483874527712213));
#21693=CARTESIAN_POINT('Ctrl Pts',(-14.0954494858794,16.8491384993429,0.505160775836598));
#21694=CARTESIAN_POINT('Ctrl Pts',(-13.935845283737,16.6603046231705,0.515078993620139));
#21695=CARTESIAN_POINT('Ctrl Pts',(-13.6903827463215,16.223642546113,0.533913007255683));
#21696=CARTESIAN_POINT('Ctrl Pts',(-13.6105539996563,15.9778499407052,0.544514480397023));
#21697=CARTESIAN_POINT('Ctrl Pts',(-13.5518158441316,15.4739117712167,0.566250231803642));
#21698=CARTESIAN_POINT('Ctrl Pts',(-13.571742794709,15.2208352901084,0.577165871485818));
#21699=CARTESIAN_POINT('Ctrl Pts',(-13.7057278794298,14.742684868917,0.597789351347523));
#21700=CARTESIAN_POINT('Ctrl Pts',(-13.8161488953126,14.5214408844327,0.606664573343451));
#21701=CARTESIAN_POINT('Ctrl Pts',(-14.1219606735895,14.1213400688706,0.626716158351945));
#21702=CARTESIAN_POINT('Ctrl Pts',(-14.318568611901,13.9495491173579,0.637764922719238));
#21703=CARTESIAN_POINT('Ctrl Pts',(-14.7590310485592,13.6984440207756,0.659632917824901));
#21704=CARTESIAN_POINT('Ctrl Pts',(-14.9966959458147,13.6181551918391,0.670241966963359));
#21705=CARTESIAN_POINT('Ctrl Pts',(-15.3284077888473,13.5736457522818,0.683592357862532));
#21706=CARTESIAN_POINT('Ctrl Pts',(-15.4142441778543,13.5679367061317,0.686921743980895));
#21707=CARTESIAN_POINT('Ctrl Pts',(-15.5,13.5679367061317,0.69012499999983));
#21708=CARTESIAN_POINT('Ctrl Pts',(-15.5000000000001,13.5679367061317,0.221374999999879));
#21709=CARTESIAN_POINT('Ctrl Pts',(-15.3093450221423,13.5679367061317,0.214253422827828));
#21710=CARTESIAN_POINT('Ctrl Pts',(-15.1194546083814,13.5961535790767,0.206551882575901));
#21711=CARTESIAN_POINT('Ctrl Pts',(-14.6948718232558,13.7256105046371,0.187900494787472));
#21712=CARTESIAN_POINT('Ctrl Pts',(-14.4700098904008,13.8459724738417,0.176905464603589));
#21713=CARTESIAN_POINT('Ctrl Pts',(-14.0753526090742,14.1696924217256,0.155182435525569));
#21714=CARTESIAN_POINT('Ctrl Pts',(-13.9107790537501,14.3714265999853,0.145052382171085));
#21715=CARTESIAN_POINT('Ctrl Pts',(-13.6758632413355,14.8173319838793,0.125819688237564));
#21716=CARTESIAN_POINT('Ctrl Pts',(-13.6037990124408,15.0551292052584,0.115563070259359));
#21717=CARTESIAN_POINT('Ctrl Pts',(-13.5518334963172,15.5544792850638,0.0940252113380078));
#21718=CARTESIAN_POINT('Ctrl Pts',(-13.5761558231528,15.8116932971635,0.0829311125699534));
#21719=CARTESIAN_POINT('Ctrl Pts',(-13.7215598037034,16.2949297857371,0.0620882615572829));
#21720=CARTESIAN_POINT('Ctrl Pts',(-13.8385708540846,16.5170608745389,0.0531675695736204));
#21721=CARTESIAN_POINT('Ctrl Pts',(-14.1505967901205,16.9049967004005,0.0331462146120232));
#21722=CARTESIAN_POINT('Ctrl Pts',(-14.3427581391604,17.0670614604204,0.0224732986552362));
#21723=CARTESIAN_POINT('Ctrl Pts',(-14.7840616507215,17.3126898337665,0.000691997111495622));
#21724=CARTESIAN_POINT('Ctrl Pts',(-15.0303088811274,17.3915129002971,-0.0102060193255635));
#21725=CARTESIAN_POINT('Ctrl Pts',(-15.5280187230135,17.4473055261743,-0.0300003018240521));
#21726=CARTESIAN_POINT('Ctrl Pts',(-15.7742335758728,17.4281050083783,-0.0389538708149526));
#21727=CARTESIAN_POINT('Ctrl Pts',(-16.2532901705975,17.296907710707,-0.0596775634273534));
#21728=CARTESIAN_POINT('Ctrl Pts',(-16.4808992967149,17.1834947938276,-0.0706253476172892));
#21729=CARTESIAN_POINT('Ctrl Pts',(-16.8829707781072,16.8732369847255,-0.0923349979158201));
#21730=CARTESIAN_POINT('Ctrl Pts',(-17.0524923783306,16.6781753243463,-0.102808198428218));
#21731=CARTESIAN_POINT('Ctrl Pts',(-17.3005030645304,16.2425026235966,-0.121599538500263));
#21732=CARTESIAN_POINT('Ctrl Pts',(-17.3801675176942,16.0080032121443,-0.131713916058721));
#21733=CARTESIAN_POINT('Ctrl Pts',(-17.4487724674381,15.5123656486931,-0.153091647532988));
#21734=CARTESIAN_POINT('Ctrl Pts',(-17.4333995515655,15.2553808907698,-0.164175858159823));
#21735=CARTESIAN_POINT('Ctrl Pts',(-17.3048200987405,14.7662503100071,-0.185272931873504));
#21736=CARTESIAN_POINT('Ctrl Pts',(-17.1944566843434,14.5384527982996,-0.194401543720054));
#21737=CARTESIAN_POINT('Ctrl Pts',(-16.894334784917,14.139727275418,-0.214210934024622));
#21738=CARTESIAN_POINT('Ctrl Pts',(-16.708188966555,13.9720032635188,-0.224781197355577));
#21739=CARTESIAN_POINT('Ctrl Pts',(-16.2741834170983,13.7111048249335,-0.246619209086019));
#21740=CARTESIAN_POINT('Ctrl Pts',(-16.0284985549801,13.6237773096857,-0.257679625272395));
#21741=CARTESIAN_POINT('Ctrl Pts',(-15.6823226738687,13.574383016875,-0.271675640769364));
#21742=CARTESIAN_POINT('Ctrl Pts',(-15.5911253193961,13.5679367061317,-0.275221175973618));
#21743=CARTESIAN_POINT('Ctrl Pts',(-15.5,13.5679367061317,-0.278625000000132));
#21744=CARTESIAN_POINT('Origin',(-15.5,15.5,11.20575));
#21745=CARTESIAN_POINT('',(-15.5,13.5679367061317,-0.778625000000138));
#21746=CARTESIAN_POINT('',(-15.5000000000213,13.5679367061317,-0.30987499999859));
#21747=CARTESIAN_POINT('',(-15.5,13.5679367061317,11.20575));
#21748=CARTESIAN_POINT('Ctrl Pts',(-15.5000000000426,13.5679367061317,-0.30987499999859));
#21749=CARTESIAN_POINT('Ctrl Pts',(-15.7451189900435,13.5679367061371,-0.300719016644455));
#21750=CARTESIAN_POINT('Ctrl Pts',(-15.9880788836297,13.6145849104549,-0.290637672395874));
#21751=CARTESIAN_POINT('Ctrl Pts',(-16.4525087353532,13.7998506160078,-0.269294302322051));
#21752=CARTESIAN_POINT('Ctrl Pts',(-16.6681650113368,13.9401358945745,-0.258213469136004));
#21753=CARTESIAN_POINT('Ctrl Pts',(-17.0300510391149,14.293798813587,-0.237068805018263));
#21754=CARTESIAN_POINT('Ctrl Pts',(-17.1737375672253,14.5027181075033,-0.227889545454448));
#21755=CARTESIAN_POINT('Ctrl Pts',(-17.3718881645073,14.9610456268797,-0.208121062677908));
#21756=CARTESIAN_POINT('Ctrl Pts',(-17.4255568606796,15.2056351161721,-0.197571482078929));
#21757=CARTESIAN_POINT('Ctrl Pts',(-17.437485526191,15.7028273877144,-0.176126693273793));
#21758=CARTESIAN_POINT('Ctrl Pts',(-17.3951930471992,15.9508283805331,-0.16542996844748));
#21759=CARTESIAN_POINT('Ctrl Pts',(-17.21903750586,16.416216845007,-0.145356934524323));
#21760=CARTESIAN_POINT('Ctrl Pts',(-17.087177913888,16.6293413959128,-0.136472617530199));
#21761=CARTESIAN_POINT('Ctrl Pts',(-16.7447233478944,16.9997020048593,-0.115693680499745));
#21762=CARTESIAN_POINT('Ctrl Pts',(-16.535223519972,17.1512859841674,-0.104599143917208));
#21763=CARTESIAN_POINT('Ctrl Pts',(-16.0781299074097,17.3599329092899,-0.0830255691567));
#21764=CARTESIAN_POINT('Ctrl Pts',(-15.8364334516315,17.4184418092008,-0.0727356319075368));
#21765=CARTESIAN_POINT('Ctrl Pts',(-15.3335771418074,17.4419572678446,-0.053445198139043));
#21766=CARTESIAN_POINT('Ctrl Pts',(-15.0770448720173,17.4026393126747,-0.0434417100341447));
#21767=CARTESIAN_POINT('Ctrl Pts',(-14.5982616364445,17.2273302215971,-0.0217769181315668));
#21768=CARTESIAN_POINT('Ctrl Pts',(-14.3801849192581,17.0946215718084,-0.010769070426221));
#21769=CARTESIAN_POINT('Ctrl Pts',(-14.0137016048736,16.7583973031524,0.0101712371105013));
#21770=CARTESIAN_POINT('Ctrl Pts',(-13.8665662971669,16.5604348396372,0.0193865553793818));
#21771=CARTESIAN_POINT('Ctrl Pts',(-13.648896034541,16.1097762694873,0.0388242627076077));
#21772=CARTESIAN_POINT('Ctrl Pts',(-13.5844810246986,15.8594139033154,0.0496228377752732));
#21773=CARTESIAN_POINT('Ctrl Pts',(-13.5572975229277,15.3542160204944,0.0714129228630835));
#21774=CARTESIAN_POINT('Ctrl Pts',(-13.5924291711366,15.1043600205154,0.0821896574543688));
#21775=CARTESIAN_POINT('Ctrl Pts',(-13.7549549306398,14.6347353821394,0.10244540510795));
#21776=CARTESIAN_POINT('Ctrl Pts',(-13.8797188217565,14.4190031858112,0.111248274994825));
#21777=CARTESIAN_POINT('Ctrl Pts',(-14.2102312356738,14.0387180251795,0.131795166002758));
#21778=CARTESIAN_POINT('Ctrl Pts',(-14.4157066951986,13.8803875205858,0.142884874300423));
#21779=CARTESIAN_POINT('Ctrl Pts',(-14.8677637645238,13.6576628179057,0.164573917775849));
#21780=CARTESIAN_POINT('Ctrl Pts',(-15.1083498919245,13.5919750720435,0.174977198896067));
#21781=CARTESIAN_POINT('Ctrl Pts',(-15.4031822744539,13.569754032749,0.186469354010824));
#21782=CARTESIAN_POINT('Ctrl Pts',(-15.4516175612204,13.5679367061317,0.188317760160552));
#21783=CARTESIAN_POINT('Ctrl Pts',(-15.4999999999999,13.5679367061317,0.190124999999822));
#21784=CARTESIAN_POINT('Ctrl Pts',(-15.5,13.5679367061317,-0.278625000000131));
#21785=CARTESIAN_POINT('Ctrl Pts',(-15.3467892597189,13.5679367061317,-0.284347914359666));
#21786=CARTESIAN_POINT('Ctrl Pts',(-15.1938118281016,13.5861582264254,-0.290455077212558));
#21787=CARTESIAN_POINT('Ctrl Pts',(-14.8002115590521,13.6816903721264,-0.30721755017852));
#21788=CARTESIAN_POINT('Ctrl Pts',(-14.5700164472504,13.7879612604545,-0.318107905048228));
#21789=CARTESIAN_POINT('Ctrl Pts',(-14.1593674324255,14.0854112710006,-0.339861742243558));
#21790=CARTESIAN_POINT('Ctrl Pts',(-13.9839732656644,14.2752366145712,-0.350507031688753));
#21791=CARTESIAN_POINT('Ctrl Pts',(-13.7231840673424,14.7026885542338,-0.369466729765817));
#21792=CARTESIAN_POINT('Ctrl Pts',(-13.6365422675758,14.9340075266013,-0.37921273586801));
#21793=CARTESIAN_POINT('Ctrl Pts',(-13.5527035685452,15.4259040924359,-0.400429111447581));
#21794=CARTESIAN_POINT('Ctrl Pts',(-13.5598498556332,15.6824101504194,-0.411492674857324));
#21795=CARTESIAN_POINT('Ctrl Pts',(-13.6708737217057,16.1685436044088,-0.432460477152238));
#21796=CARTESIAN_POINT('Ctrl Pts',(-13.7700581636469,16.3943923190575,-0.441627804171639));
#21797=CARTESIAN_POINT('Ctrl Pts',(-14.0539091255659,16.8066128735469,-0.46112045496409));
#21798=CARTESIAN_POINT('Ctrl Pts',(-14.2395717537967,16.9865111568954,-0.471935218600938));
#21799=CARTESIAN_POINT('Ctrl Pts',(-14.6649766982385,17.260117111467,-0.493726018953733));
#21800=CARTESIAN_POINT('Ctrl Pts',(-14.8993253045762,17.3532344934425,-0.50448785312903));
#21801=CARTESIAN_POINT('Ctrl Pts',(-15.3879151897707,17.4445879148856,-0.524708376132417));
#21802=CARTESIAN_POINT('Ctrl Pts',(-15.6373703514434,17.4429655287442,-0.533521108433316));
#21803=CARTESIAN_POINT('Ctrl Pts',(-16.1314699144086,17.3439130073667,-0.554113473589034));
#21804=CARTESIAN_POINT('Ctrl Pts',(-16.3705992585577,17.2437932713042,-0.565204895717519));
#21805=CARTESIAN_POINT('Ctrl Pts',(-16.7876645305446,16.9614315561499,-0.586873008236942));
#21806=CARTESIAN_POINT('Ctrl Pts',(-16.9637580966902,16.7850271274736,-0.597254988511056));
#21807=CARTESIAN_POINT('Ctrl Pts',(-17.2443400454302,16.3689556312255,-0.616708580128513));
#21808=CARTESIAN_POINT('Ctrl Pts',(-17.3436265737928,16.1315609718477,-0.626384649668764));
#21809=CARTESIAN_POINT('Ctrl Pts',(-17.4440644805083,15.6332086945697,-0.647879471588744));
#21810=CARTESIAN_POINT('Ctrl Pts',(-17.4447534368414,15.3772600500546,-0.658918992797644));
#21811=CARTESIAN_POINT('Ctrl Pts',(-17.3489811389163,14.8884838636653,-0.680000780850369));
#21812=CARTESIAN_POINT('Ctrl Pts',(-17.2568181639608,14.6596166093872,-0.689459136144938));
#21813=CARTESIAN_POINT('Ctrl Pts',(-16.9858620067821,14.238805099094,-0.708655396087524));
#21814=CARTESIAN_POINT('Ctrl Pts',(-16.8058878841893,14.0532686231487,-0.719379268374338));
#21815=CARTESIAN_POINT('Ctrl Pts',(-16.3885881553997,13.7662002686923,-0.741157641480895));
#21816=CARTESIAN_POINT('Ctrl Pts',(-16.1564785085564,13.665689225055,-0.751995294214013));
#21817=CARTESIAN_POINT('Ctrl Pts',(-15.7761115117429,13.5827427725166,-0.767992040173275));
#21818=CARTESIAN_POINT('Ctrl Pts',(-15.6381065100508,13.5679367061317,-0.773466277262654));
#21819=CARTESIAN_POINT('Ctrl Pts',(-15.5,13.5679367061317,-0.778625000000138));
#21820=CARTESIAN_POINT('Origin',(-15.5,15.5,11.20575));
#21821=CARTESIAN_POINT('',(-15.4999999999999,13.5679367061317,-1.27862500000015));
#21822=CARTESIAN_POINT('',(-15.5,13.5679367061317,-0.809875000000185));
#21823=CARTESIAN_POINT('',(-15.5,13.5679367061317,11.20575));
#21824=CARTESIAN_POINT('Ctrl Pts',(-15.5000000000001,13.5679367061317,-0.809875000000184));
#21825=CARTESIAN_POINT('Ctrl Pts',(-15.5387848588903,13.5679367061317,-0.808426260665929));
#21826=CARTESIAN_POINT('Ctrl Pts',(-15.5776081217821,13.569104553761,-0.806950901143725));
#21827=CARTESIAN_POINT('Ctrl Pts',(-15.8627498107999,13.5863172258654,-0.79592873452912));
#21828=CARTESIAN_POINT('Ctrl Pts',(-16.1039441624047,13.6482441649587,-0.785583839426258));
#21829=CARTESIAN_POINT('Ctrl Pts',(-16.5586938389718,13.8636040208236,-0.763953047887055));
#21830=CARTESIAN_POINT('Ctrl Pts',(-16.7663048606795,14.0184106751406,-0.752859564438582));
#21831=CARTESIAN_POINT('Ctrl Pts',(-17.1030886658293,14.3935142993235,-0.73219016123049));
#21832=CARTESIAN_POINT('Ctrl Pts',(-17.2315636886463,14.6078734364709,-0.723354008700342));
#21833=CARTESIAN_POINT('Ctrl Pts',(-17.4012591024431,15.0752831240919,-0.703193795820486));
#21834=CARTESIAN_POINT('Ctrl Pts',(-17.4401670421017,15.3241884796659,-0.692458064216697));
#21835=CARTESIAN_POINT('Ctrl Pts',(-17.4209116308134,15.8293918059367,-0.670667744343198));
#21836=CARTESIAN_POINT('Ctrl Pts',(-17.3604173282467,16.0807480284641,-0.659826302479591));
#21837=CARTESIAN_POINT('Ctrl Pts',(-17.1497816929781,16.5348352725858,-0.640240710332106));
#21838=CARTESIAN_POINT('Ctrl Pts',(-17.0057085011959,16.7351193667879,-0.631148276498292));
#21839=CARTESIAN_POINT('Ctrl Pts',(-16.6447314320371,17.0767669839641,-0.610296685602456));
#21840=CARTESIAN_POINT('Ctrl Pts',(-16.4291281586241,17.2126942752496,-0.599311816112351));
#21841=CARTESIAN_POINT('Ctrl Pts',(-15.9522914740593,17.396071415368,-0.577545739488896));
#21842=CARTESIAN_POINT('Ctrl Pts',(-15.6949512567242,17.4394863853226,-0.567317142600485));
#21843=CARTESIAN_POINT('Ctrl Pts',(-15.1907605692904,17.4229690903242,-0.548127787168027));
#21844=CARTESIAN_POINT('Ctrl Pts',(-14.9485965706545,17.3679857370151,-0.537896417242229));
#21845=CARTESIAN_POINT('Ctrl Pts',(-14.4891878782661,17.166282104194,-0.516386105083495));
#21846=CARTESIAN_POINT('Ctrl Pts',(-14.2777915836231,17.0180420352629,-0.505292843771063));
#21847=CARTESIAN_POINT('Ctrl Pts',(-13.9295152530061,16.6526099917286,-0.484402733995876));
#21848=CARTESIAN_POINT('Ctrl Pts',(-13.7941507738708,16.4407479085025,-0.475451133965662));
#21849=CARTESIAN_POINT('Ctrl Pts',(-13.611383887522,15.9774528011728,-0.455468390267086));
#21850=CARTESIAN_POINT('Ctrl Pts',(-13.5656468617909,15.7304237057034,-0.444813585105621));
#21851=CARTESIAN_POINT('Ctrl Pts',(-13.5704710073905,15.2255315160606,-0.423036685109424));
#21852=CARTESIAN_POINT('Ctrl Pts',(-13.623779229161,14.9725259783178,-0.412124105341039));
#21853=CARTESIAN_POINT('Ctrl Pts',(-13.8215336428728,14.5122846645607,-0.392273077201934));
#21854=CARTESIAN_POINT('Ctrl Pts',(-13.9600852553974,14.3077326406346,-0.383350131532038));
#21855=CARTESIAN_POINT('Ctrl Pts',(-14.311092329695,13.9563854884097,-0.362661772922335));
#21856=CARTESIAN_POINT('Ctrl Pts',(-14.5221235135244,13.814770334655,-0.351725021873647));
#21857=CARTESIAN_POINT('Ctrl Pts',(-14.9904064163151,13.6188695990394,-0.330008374038312));
#21858=CARTESIAN_POINT('Ctrl Pts',(-15.2437584839143,13.5679791180275,-0.319447360158956));
#21859=CARTESIAN_POINT('Ctrl Pts',(-15.4997866765027,13.5679367149642,-0.309882968509973));
#21860=CARTESIAN_POINT('Ctrl Pts',(-15.4998933384699,13.5679367061317,-0.309878984151688));
#21861=CARTESIAN_POINT('Ctrl Pts',(-15.5000000000426,13.5679367061317,-0.30987499999859));
#21862=CARTESIAN_POINT('Ctrl Pts',(-15.5,13.5679367061317,-0.778625000000138));
#21863=CARTESIAN_POINT('Ctrl Pts',(-15.3931460600035,13.5679367061317,-0.782616338639041));
#21864=CARTESIAN_POINT('Ctrl Pts',(-15.2862458066186,13.5768002208548,-0.786800556825666));
#21865=CARTESIAN_POINT('Ctrl Pts',(-14.9264097349309,13.6371564581267,-0.801543228515925));
#21866=CARTESIAN_POINT('Ctrl Pts',(-14.6835020776055,13.7301105172148,-0.812621248594988));
#21867=CARTESIAN_POINT('Ctrl Pts',(-14.2567488546817,14.0004851883713,-0.834392725983059));
#21868=CARTESIAN_POINT('Ctrl Pts',(-14.0749328111488,14.1720617647974,-0.844884342273106));
#21869=CARTESIAN_POINT('Ctrl Pts',(-13.7832732837112,14.5783544242248,-0.864540827785101));
#21870=CARTESIAN_POINT('Ctrl Pts',(-13.6776776440773,14.8102645186437,-0.873875479390643));
#21871=CARTESIAN_POINT('Ctrl Pts',(-13.5612057991943,15.3034623332341,-0.895147980148236));
#21872=CARTESIAN_POINT('Ctrl Pts',(-13.552197396611,15.5600993604861,-0.906217192531462));
#21873=CARTESIAN_POINT('Ctrl Pts',(-13.6325934592672,16.0528776431264,-0.927471598128334));
#21874=CARTESIAN_POINT('Ctrl Pts',(-13.7176559736562,16.2849105083636,-0.937309340873369));
#21875=CARTESIAN_POINT('Ctrl Pts',(-13.9755352339037,16.7142424065984,-0.956200886377741));
#21876=CARTESIAN_POINT('Ctrl Pts',(-14.1496041202698,16.9052695292978,-0.966822589771756));
#21877=CARTESIAN_POINT('Ctrl Pts',(-14.5583089435885,17.2056519897364,-0.988567046050803));
#21878=CARTESIAN_POINT('Ctrl Pts',(-14.7879324229243,17.3135593941174,-0.999471341534755));
#21879=CARTESIAN_POINT('Ctrl Pts',(-15.2696786466829,17.4338950578203,-1.02006125963416));
#21880=CARTESIAN_POINT('Ctrl Pts',(-15.5166980413127,17.4474891140478,-1.02891605403808));
#21881=CARTESIAN_POINT('Ctrl Pts',(-16.0156874195765,17.3798092848061,-1.04901448947301));
#21882=CARTESIAN_POINT('Ctrl Pts',(-16.2621352115938,17.2940873362134,-1.06006877807144));
#21883=CARTESIAN_POINT('Ctrl Pts',(-16.698154944133,17.0359029315518,-1.08192349546387));
#21884=CARTESIAN_POINT('Ctrl Pts',(-16.8855107789499,16.8692878721634,-1.09251504125555));
#21885=CARTESIAN_POINT('Ctrl Pts',(-17.1880123646469,16.472705598965,-1.11236709941354));
#21886=CARTESIAN_POINT('Ctrl Pts',(-17.2997096590055,16.2460520791468,-1.12144644415624));
#21887=CARTESIAN_POINT('Ctrl Pts',(-17.431671791372,15.7580841556283,-1.1424933703908));
#21888=CARTESIAN_POINT('Ctrl Pts',(-17.4488346169962,15.5010293356259,-1.15358060291997));
#21889=CARTESIAN_POINT('Ctrl Pts',(-17.383549418459,15.0046042925852,-1.17499229979244));
#21890=CARTESIAN_POINT('Ctrl Pts',(-17.3053971666591,14.7694246899964,-1.18513601520691));
#21891=CARTESIAN_POINT('Ctrl Pts',(-17.0601513563756,14.3319804120671,-1.20400376656016));
#21892=CARTESIAN_POINT('Ctrl Pts',(-16.8918928500653,14.1358043641068,-1.21438674923054));
#21893=CARTESIAN_POINT('Ctrl Pts',(-16.491712694381,13.8228284522729,-1.23608437073301));
#21894=CARTESIAN_POINT('Ctrl Pts',(-16.264686804895,13.7078902729296,-1.24704326280146));
#21895=CARTESIAN_POINT('Ctrl Pts',(-15.8517814524953,13.5920235017939,-1.26496537709516));
#21896=CARTESIAN_POINT('Ctrl Pts',(-15.676151507024,13.5679367061317,-1.27204517415274));
#21897=CARTESIAN_POINT('Ctrl Pts',(-15.4999999999999,13.5679367061317,-1.27862500000015));
#21898=CARTESIAN_POINT('Origin',(-15.5,15.5,11.20575));
#21899=CARTESIAN_POINT('',(-15.5,13.5679367061317,-1.77862500000015));
#21900=CARTESIAN_POINT('',(-15.5000000000001,13.5679367061317,-1.30987500000019));
#21901=CARTESIAN_POINT('',(-15.5,13.5679367061317,11.20575));
#21902=CARTESIAN_POINT('',(-16.6356236642092,13.9369173237082,-2.22824839960634));
#21903=CARTESIAN_POINT('Ctrl Pts',(-15.5,13.5679367061317,-1.77862500000015));
#21904=CARTESIAN_POINT('Ctrl Pts',(-15.4713110103049,13.5679367061317,-1.77969662611974));
#21905=CARTESIAN_POINT('Ctrl Pts',(-15.4425999921594,13.5685756992767,-1.78078285552937));
#21906=CARTESIAN_POINT('Ctrl Pts',(-15.1581590399474,13.5812658327421,-1.79168131479254));
#21907=CARTESIAN_POINT('Ctrl Pts',(-14.9072543398391,13.6433835357265,-1.80239303666449));
#21908=CARTESIAN_POINT('Ctrl Pts',(-14.4490712181685,13.8594981524984,-1.82416835552268));
#21909=CARTESIAN_POINT('Ctrl Pts',(-14.2453192502126,14.0095359244182,-1.83501484569199));
#21910=CARTESIAN_POINT('Ctrl Pts',(-13.9097095424868,14.3755767710421,-1.85544494570745));
#21911=CARTESIAN_POINT('Ctrl Pts',(-13.779653496445,14.5868970845778,-1.86424124385709));
#21912=CARTESIAN_POINT('Ctrl Pts',(-13.601624809573,15.0579406863098,-1.88455819392919));
#21913=CARTESIAN_POINT('Ctrl Pts',(-13.5596639923122,15.314726118177,-1.89563380726797));
#21914=CARTESIAN_POINT('Ctrl Pts',(-13.5785378997819,15.8197591251871,-1.9174167809682));
#21915=CARTESIAN_POINT('Ctrl Pts',(-13.635337470358,16.063306547793,-1.92792141537377));
#21916=CARTESIAN_POINT('Ctrl Pts',(-13.8396294894159,16.5196132324098,-1.94760273594545));
#21917=CARTESIAN_POINT('Ctrl Pts',(-13.98670541897,16.7273518608751,-1.95690084581238));
#21918=CARTESIAN_POINT('Ctrl Pts',(-14.3540458828622,17.0761951408069,-1.97814531086595));
#21919=CARTESIAN_POINT('Ctrl Pts',(-14.5713394118551,17.213239044857,-1.9892173975925));
#21920=CARTESIAN_POINT('Ctrl Pts',(-15.0377637904636,17.3918917772351,-2.01049265500658));
#21921=CARTESIAN_POINT('Ctrl Pts',(-15.2811490461273,17.4351931175239,-2.02038271492023));
#21922=CARTESIAN_POINT('Ctrl Pts',(-15.7819930616688,17.4284331863443,-2.03923663513813));
#21923=CARTESIAN_POINT('Ctrl Pts',(-16.0346645547899,17.3741617366328,-2.04984514097278));
#21924=CARTESIAN_POINT('Ctrl Pts',(-16.500008982865,17.1721421784805,-2.0715839851788));
#21925=CARTESIAN_POINT('Ctrl Pts',(-16.7088902825659,17.0279622254971,-2.08249574331544));
#21926=CARTESIAN_POINT('Ctrl Pts',(-17.055293507135,16.6721862680338,-2.10310764444889));
#21927=CARTESIAN_POINT('Ctrl Pts',(-17.191302469575,16.4656337932766,-2.11197549347074));
#21928=CARTESIAN_POINT('Ctrl Pts',(-17.383958897045,16.0003669873985,-2.13204328004182));
#21929=CARTESIAN_POINT('Ctrl Pts',(-17.4339176130592,15.7441588929761,-2.14309399178763));
#21930=CARTESIAN_POINT('Ctrl Pts',(-17.4301770605656,15.2372592429962,-2.16495747712602));
#21931=CARTESIAN_POINT('Ctrl Pts',(-17.3804225882662,14.9914303047801,-2.17556051736614));
#21932=CARTESIAN_POINT('Ctrl Pts',(-17.2188593063871,14.6006806202927,-2.19241424768163));
#21933=CARTESIAN_POINT('Ctrl Pts',(-17.1307744677382,14.4493679380718,-2.19870147391129));
#21934=CARTESIAN_POINT('Ctrl Pts',(-16.9124347549226,14.1693732822038,-2.21289549932321));
#21935=CARTESIAN_POINT('Ctrl Pts',(-16.78183780444,14.0431460180095,-2.22049591927456));
#21936=CARTESIAN_POINT('Ctrl Pts',(-16.6356236661869,13.9369173213456,-2.22824840453312));
#21937=CARTESIAN_POINT('',(-16.6356257705294,13.936918850212,-1.75949829183042));
#21938=CARTESIAN_POINT('',(-16.6356252385745,13.9369184637308,-1.75949832116282));
#21939=CARTESIAN_POINT('Ctrl Pts',(-16.6356257705685,13.9369188502404,-1.75949829295571));
#21940=CARTESIAN_POINT('Ctrl Pts',(-16.8232265616208,14.073216503712,-1.74955141913567));
#21941=CARTESIAN_POINT('Ctrl Pts',(-16.9847823163708,14.2421926306507,-1.73987267086338));
#21942=CARTESIAN_POINT('Ctrl Pts',(-17.2378815903649,14.625688547538,-1.72214816701709));
#21943=CARTESIAN_POINT('Ctrl Pts',(-17.3287014043758,14.8362794639401,-1.71350244965325));
#21944=CARTESIAN_POINT('Ctrl Pts',(-17.4385845729922,15.3036899854237,-1.69334220080741));
#21945=CARTESIAN_POINT('Ctrl Pts',(-17.447619886958,15.5584934383095,-1.68235207375453));
#21946=CARTESIAN_POINT('Ctrl Pts',(-17.366264820819,16.0626255591014,-1.66060795688251));
#21947=CARTESIAN_POINT('Ctrl Pts',(-17.2745029457006,16.306592918934,-1.65043016901723));
#21948=CARTESIAN_POINT('Ctrl Pts',(-17.0069230177962,16.7339605492266,-1.63121863353647));
#21949=CARTESIAN_POINT('Ctrl Pts',(-16.8376064327547,16.9157196559878,-1.62097431691814));
#21950=CARTESIAN_POINT('Ctrl Pts',(-16.4321558772125,17.2115388605548,-1.59944982869592));
#21951=CARTESIAN_POINT('Ctrl Pts',(-16.1976492003962,17.3197729456469,-1.58835608490562));
#21952=CARTESIAN_POINT('Ctrl Pts',(-15.7067373188973,17.4370349875308,-1.56749008537743));
#21953=CARTESIAN_POINT('Ctrl Pts',(-15.4557223788825,17.44753196976,-1.558554684095));
#21954=CARTESIAN_POINT('Ctrl Pts',(-14.9634366275307,17.3726902789252,-1.53855219877784));
#21955=CARTESIAN_POINT('Ctrl Pts',(-14.726821985697,17.2880297167385,-1.52788809973695));
#21956=CARTESIAN_POINT('Ctrl Pts',(-14.2927306055592,17.0300046441306,-1.50610884865212));
#21957=CARTESIAN_POINT('Ctrl Pts',(-14.1008202908091,16.8567343671546,-1.49520365267535));
#21958=CARTESIAN_POINT('Ctrl Pts',(-13.8024087055843,16.4544579219329,-1.47538156930738));
#21959=CARTESIAN_POINT('Ctrl Pts',(-13.6952482164322,16.2319055093249,-1.46644338907453));
#21960=CARTESIAN_POINT('Ctrl Pts',(-13.5679372308721,15.7518323297933,-1.44573697721874));
#21961=CARTESIAN_POINT('Ctrl Pts',(-13.5515962723608,15.4981347275301,-1.43479454747414));
#21962=CARTESIAN_POINT('Ctrl Pts',(-13.6177050294595,14.9946779887315,-1.41307956103121));
#21963=CARTESIAN_POINT('Ctrl Pts',(-13.7011232772003,14.7500889892398,-1.4025630039161));
#21964=CARTESIAN_POINT('Ctrl Pts',(-13.9530518157522,14.3167686917902,-1.38380772364012));
#21965=CARTESIAN_POINT('Ctrl Pts',(-14.1156697545305,14.1300765218333,-1.37370723711988));
#21966=CARTESIAN_POINT('Ctrl Pts',(-14.5094994028657,13.8216873535972,-1.35234574472332));
#21967=CARTESIAN_POINT('Ctrl Pts',(-14.7392900935943,13.7058009544622,-1.34126312922332));
#21968=CARTESIAN_POINT('Ctrl Pts',(-15.1530393767014,13.5913602763721,-1.32334024636833));
#21969=CARTESIAN_POINT('Ctrl Pts',(-15.3262907155805,13.5679367061317,-1.31636360097141));
#21970=CARTESIAN_POINT('Ctrl Pts',(-15.5000000000001,13.5679367061317,-1.30987500000019));
#21971=CARTESIAN_POINT('Origin',(15.4999999999998,15.5000000000002,11.20575));
#21972=CARTESIAN_POINT('',(13.5679367061315,15.5000000000002,1.22137499999984));
#21973=CARTESIAN_POINT('',(13.5679367061315,15.5000000000002,1.38580000000003));
#21974=CARTESIAN_POINT('',(13.5679367061315,15.5000000000002,11.20575));
#21975=CARTESIAN_POINT('',(16.4140591443296,17.2021646372137,1.3857999999999));
#21976=CARTESIAN_POINT('Origin',(15.4999999999998,15.5000000000002,1.3858));
#21977=CARTESIAN_POINT('Ctrl Pts',(16.4140591443296,17.2021646372137,1.38579999999989));
#21978=CARTESIAN_POINT('Ctrl Pts',(16.2625891375117,17.2835037402574,1.37926682864456));
#21979=CARTESIAN_POINT('Ctrl Pts',(16.1009499217413,17.3442553078036,1.37229504118279));
#21980=CARTESIAN_POINT('Ctrl Pts',(15.7606791264406,17.422586671179,1.35761855532521));
#21981=CARTESIAN_POINT('Ctrl Pts',(15.5832774891468,17.4383898562024,1.34996690653027));
#21982=CARTESIAN_POINT('Ctrl Pts',(15.1505459519398,17.4173618065492,1.33130242408378));
#21983=CARTESIAN_POINT('Ctrl Pts',(14.8998465930936,17.354246908948,1.32048931392145));
#21984=CARTESIAN_POINT('Ctrl Pts',(14.4480453997679,17.1389102319479,1.30100232321918));
#21985=CARTESIAN_POINT('Ctrl Pts',(14.2493134355933,16.9927945768321,1.29183017936196));
#21986=CARTESIAN_POINT('Ctrl Pts',(13.9112799546867,16.6281426360987,1.27091926225214));
#21987=CARTESIAN_POINT('Ctrl Pts',(13.7774947328739,16.4108843723267,1.25991876918149));
#21988=CARTESIAN_POINT('Ctrl Pts',(13.608962253039,15.9581594814273,1.23937348399882));
#21989=CARTESIAN_POINT('Ctrl Pts',(13.5679367061315,15.7298816359029,1.22996181912679));
#21990=CARTESIAN_POINT('Ctrl Pts',(13.5679367061316,15.5000000000002,1.22137499999984));
#21991=CARTESIAN_POINT('Origin',(15.4999999999998,15.5000000000002,11.20575));
#21992=CARTESIAN_POINT('',(13.5679367061316,15.5000000000002,0.721374999999831));
#21993=CARTESIAN_POINT('',(13.5679367061315,15.5000000000002,1.19012499999989));
#21994=CARTESIAN_POINT('',(13.5679367061315,15.5000000000002,11.20575));
#21995=CARTESIAN_POINT('',(17.0070594673501,16.7089831815966,1.3858));
#21996=CARTESIAN_POINT('Ctrl Pts',(13.5679367061316,15.5000000000002,1.19012499999989));
#21997=CARTESIAN_POINT('Ctrl Pts',(13.5679367061316,15.6209597157626,1.19464323477242));
#21998=CARTESIAN_POINT('Ctrl Pts',(13.5792946957062,15.7419184750208,1.19940637898304));
#21999=CARTESIAN_POINT('Ctrl Pts',(13.650067406739,16.1137167329625,1.21482051737726));
#22000=CARTESIAN_POINT('Ctrl Pts',(13.7479960405405,16.354030851272,1.22590894156177));
#22001=CARTESIAN_POINT('Ctrl Pts',(14.026702340502,16.7741136008835,1.2476109342981));
#22002=CARTESIAN_POINT('Ctrl Pts',(14.2016401214973,16.951982381632,1.2580275949881));
#22003=CARTESIAN_POINT('Ctrl Pts',(14.6147032779426,17.2359894885843,1.27754424976224));
#22004=CARTESIAN_POINT('Ctrl Pts',(14.8503902891229,17.3372359040127,1.2871061753863));
#22005=CARTESIAN_POINT('Ctrl Pts',(15.3471703745486,17.4426537117393,1.30853318586962));
#22006=CARTESIAN_POINT('Ctrl Pts',(15.6033601229598,17.4459126157985,1.31958310631927));
#22007=CARTESIAN_POINT('Ctrl Pts',(16.0780177664312,17.3577448351807,1.3400559364528));
#22008=CARTESIAN_POINT('Ctrl Pts',(16.2939199281618,17.2762233318698,1.34923226468184));
#22009=CARTESIAN_POINT('Ctrl Pts',(16.6881134566226,17.0408566361,1.36652510317408));
#22010=CARTESIAN_POINT('Ctrl Pts',(16.863050795795,16.8884973676924,1.37598889193061));
#22011=CARTESIAN_POINT('Ctrl Pts',(17.0070594673508,16.7089831815957,1.38580000000003));
#22012=CARTESIAN_POINT('Origin',(15.4999999999998,15.5000000000002,1.3858));
#22013=CARTESIAN_POINT('Ctrl Pts',(13.5679367061315,15.5000000000002,1.22137499999984));
#22014=CARTESIAN_POINT('Ctrl Pts',(13.5679367061315,15.472934163652,1.22036400388295));
#22015=CARTESIAN_POINT('Ctrl Pts',(13.5685054395939,15.445846997633,1.21933994579038));
#22016=CARTESIAN_POINT('Ctrl Pts',(13.5800041738241,15.1726369385485,1.2088866901258));
#22017=CARTESIAN_POINT('Ctrl Pts',(13.6373364196653,14.9307787642574,1.19861608776315));
#22018=CARTESIAN_POINT('Ctrl Pts',(13.8436681824179,14.4729009298073,1.17706314833023));
#22019=CARTESIAN_POINT('Ctrl Pts',(13.9941383692371,14.2627623230356,1.16596877122891));
#22020=CARTESIAN_POINT('Ctrl Pts',(14.3628583037133,13.9183617244766,1.14515252622457));
#22021=CARTESIAN_POINT('Ctrl Pts',(14.5755603825233,13.785334043101,1.1362477283077));
#22022=CARTESIAN_POINT('Ctrl Pts',(15.0402511771328,13.6069662799688,1.11620478612924));
#22023=CARTESIAN_POINT('Ctrl Pts',(15.2879321567374,13.5635189852419,1.10552186404319));
#22024=CARTESIAN_POINT('Ctrl Pts',(15.7929752641122,13.573195404212,1.08373845469624));
#22025=CARTESIAN_POINT('Ctrl Pts',(16.0454493144931,13.6289269314022,1.07284879892505));
#22026=CARTESIAN_POINT('Ctrl Pts',(16.5036338507401,13.8310245098165,1.05308648326572));
#22027=CARTESIAN_POINT('Ctrl Pts',(16.7067442549318,13.9714260898445,1.04411430770358));
#22028=CARTESIAN_POINT('Ctrl Pts',(17.0548537164756,14.3257784405245,1.02337081593677));
#22029=CARTESIAN_POINT('Ctrl Pts',(17.1945806684026,14.5383567468982,1.01241699563566));
#22030=CARTESIAN_POINT('Ctrl Pts',(17.3860429606825,15.008844336194,0.990713714647896));
#22031=CARTESIAN_POINT('Ctrl Pts',(17.4344332047204,15.2627143705022,0.980289491361847));
#22032=CARTESIAN_POINT('Ctrl Pts',(17.4296140644269,15.764107690739,0.961456907730253));
#22033=CARTESIAN_POINT('Ctrl Pts',(17.3804673298212,16.0069337841767,0.951326678315792));
#22034=CARTESIAN_POINT('Ctrl Pts',(17.1903012303483,16.4699471301539,0.929930537929737));
#22035=CARTESIAN_POINT('Ctrl Pts',(17.0476412722629,16.6843681045384,0.918844635155068));
#22036=CARTESIAN_POINT('Ctrl Pts',(16.6904570709538,17.0422253708337,0.897774518657255));
#22037=CARTESIAN_POINT('Ctrl Pts',(16.4806668479972,17.1834288054785,0.888672908972444));
#22038=CARTESIAN_POINT('Ctrl Pts',(16.0208578482245,17.3770350149772,0.868840527305979));
#22039=CARTESIAN_POINT('Ctrl Pts',(15.7755220881537,17.4283735116388,0.858258758718241));
#22040=CARTESIAN_POINT('Ctrl Pts',(15.2690019282793,17.4355092606072,0.836411641464455));
#22041=CARTESIAN_POINT('Ctrl Pts',(15.0126438264158,17.387341223535,0.825354459630359));
#22042=CARTESIAN_POINT('Ctrl Pts',(14.5460700125418,17.1979533838604,0.805230299474962));
#22043=CARTESIAN_POINT('Ctrl Pts',(14.3384565931961,17.0632817899814,0.796385555315291));
#22044=CARTESIAN_POINT('Ctrl Pts',(13.9803614872282,16.7193021672918,0.775814169009818));
#22045=CARTESIAN_POINT('Ctrl Pts',(13.8348471765416,16.5115619837911,0.764916258623728));
#22046=CARTESIAN_POINT('Ctrl Pts',(13.6296318245187,16.047792771362,0.743167333650249));
#22047=CARTESIAN_POINT('Ctrl Pts',(13.5735885358767,15.7954972629457,0.732534660769201));
#22048=CARTESIAN_POINT('Ctrl Pts',(13.5680718804954,15.5263956111567,0.722363876203961));
#22049=CARTESIAN_POINT('Ctrl Pts',(13.5679367061315,15.5131950984485,0.721867879404021));
#22050=CARTESIAN_POINT('Ctrl Pts',(13.5679367061315,15.5000000000002,0.72137499999983));
#22051=CARTESIAN_POINT('Origin',(15.4999999999998,15.5000000000002,11.20575));
#22052=CARTESIAN_POINT('',(13.5679367061315,15.5000000000002,0.221374999999826));
#22053=CARTESIAN_POINT('',(13.5679367061316,15.5000000000002,0.690124999999888));
#22054=CARTESIAN_POINT('',(13.5679367061315,15.5000000000002,11.20575));
#22055=CARTESIAN_POINT('Ctrl Pts',(13.5679367061316,15.5000000000001,0.690124999999887));
#22056=CARTESIAN_POINT('Ctrl Pts',(13.5679367061315,15.6631976348036,0.696220957019254));
#22057=CARTESIAN_POINT('Ctrl Pts',(13.5886111528802,15.8260698424817,0.702750621155699));
#22058=CARTESIAN_POINT('Ctrl Pts',(13.6937750358448,16.2318407735967,0.720175424526415));
#22059=CARTESIAN_POINT('Ctrl Pts',(13.8061679673989,16.4638288993592,0.731264781557297));
#22060=CARTESIAN_POINT('Ctrl Pts',(14.1088337976828,16.8630470507198,0.752704123005099));
#22061=CARTESIAN_POINT('Ctrl Pts',(14.2932884830908,17.028761444197,0.762872018728113));
#22062=CARTESIAN_POINT('Ctrl Pts',(14.7231251438693,17.2874053587743,0.781803012187303));
#22063=CARTESIAN_POINT('Ctrl Pts',(14.9664736216112,17.374500370631,0.79211305640897));
#22064=CARTESIAN_POINT('Ctrl Pts',(15.4692792372015,17.4482099203795,0.81379995874744));
#22065=CARTESIAN_POINT('Ctrl Pts',(15.7235658751721,17.4355847239787,0.824767794651923));
#22066=CARTESIAN_POINT('Ctrl Pts',(16.2055976541626,17.3151733744219,0.845558684393129));
#22067=CARTESIAN_POINT('Ctrl Pts',(16.4295122772787,17.2113496874159,0.854579673980942));
#22068=CARTESIAN_POINT('Ctrl Pts',(16.8359718966532,16.919015473378,0.874264961849427));
#22069=CARTESIAN_POINT('Ctrl Pts',(17.0120418978357,16.7296891979224,0.885134014187555));
#22070=CARTESIAN_POINT('Ctrl Pts',(17.2766178136157,16.2991617620672,0.906921415251218));
#22071=CARTESIAN_POINT('Ctrl Pts',(17.3648212635818,16.0634585876003,0.917627873583951));
#22072=CARTESIAN_POINT('Ctrl Pts',(17.4465792698412,15.5727030691462,0.937722356281839));
#22073=CARTESIAN_POINT('Ctrl Pts',(17.4398199793544,15.3223565583365,0.946593274573915));
#22074=CARTESIAN_POINT('Ctrl Pts',(17.3302144103321,14.8300711076972,0.967345462671009));
#22075=CARTESIAN_POINT('Ctrl Pts',(17.2253688342258,14.5935881752457,0.978439949755262));
#22076=CARTESIAN_POINT('Ctrl Pts',(16.9351538432129,14.1832015334437,1.00002795682992));
#22077=CARTESIAN_POINT('Ctrl Pts',(16.7556158303756,14.0110153602739,1.01033156193274));
#22078=CARTESIAN_POINT('Ctrl Pts',(16.332996555328,13.7379425524703,1.02964587164789));
#22079=CARTESIAN_POINT('Ctrl Pts',(16.0918227958031,13.6429845085469,1.03959862802553));
#22080=CARTESIAN_POINT('Ctrl Pts',(15.5900949475536,13.5535333316271,1.06123904433773));
#22081=CARTESIAN_POINT('Ctrl Pts',(15.3347633934763,13.5584675814191,1.07225194933623));
#22082=CARTESIAN_POINT('Ctrl Pts',(14.8487842127029,13.6646353766641,1.09321309755172));
#22083=CARTESIAN_POINT('Ctrl Pts',(14.6220240391674,13.761672278609,1.10246053097519));
#22084=CARTESIAN_POINT('Ctrl Pts',(14.2071591450859,14.0415852702364,1.12186311344006));
#22085=CARTESIAN_POINT('Ctrl Pts',(14.0255156909756,14.2255255819059,1.13265117917161));
#22086=CARTESIAN_POINT('Ctrl Pts',(13.7477641930791,14.6484954207358,1.15444042282688));
#22087=CARTESIAN_POINT('Ctrl Pts',(13.6523788496879,14.8821830754014,1.16522647893853));
#22088=CARTESIAN_POINT('Ctrl Pts',(13.5800170676886,15.2505243179928,1.1805457564122));
#22089=CARTESIAN_POINT('Ctrl Pts',(13.5679367061316,15.375252816257,1.18546529110582));
#22090=CARTESIAN_POINT('Ctrl Pts',(13.5679367061316,15.5000000000002,1.19012499999989));
#22091=CARTESIAN_POINT('Ctrl Pts',(13.5679367061316,15.5000000000002,0.721374999999831));
#22092=CARTESIAN_POINT('Ctrl Pts',(13.5679367061316,15.2685828062759,0.71273082284504));
#22093=CARTESIAN_POINT('Ctrl Pts',(13.6095133453252,15.0388969706604,0.703254680214518));
#22094=CARTESIAN_POINT('Ctrl Pts',(13.7800568345428,14.5838672573797,0.682579933286903));
#22095=CARTESIAN_POINT('Ctrl Pts',(13.9154007889708,14.3657373187035,0.671513264894632));
#22096=CARTESIAN_POINT('Ctrl Pts',(14.2617096429524,13.9955563281774,0.650217354181319));
#22097=CARTESIAN_POINT('Ctrl Pts',(14.4688321613627,13.8467023151839,0.640851106705407));
#22098=CARTESIAN_POINT('Ctrl Pts',(14.9240794294144,13.6392165648129,0.62121548065835));
#22099=CARTESIAN_POINT('Ctrl Pts',(15.1670698899724,13.5807974419652,0.610734869018579));
#22100=CARTESIAN_POINT('Ctrl Pts',(15.6716078300757,13.5584324818414,0.588973248436394));
#22101=CARTESIAN_POINT('Ctrl Pts',(15.92849285909,13.5985422787833,0.577893339295162));
#22102=CARTESIAN_POINT('Ctrl Pts',(16.4008511612857,13.773173526314,0.557519683848905));
#22103=CARTESIAN_POINT('Ctrl Pts',(16.6132862459897,13.9018579854675,0.548728405599746));
#22104=CARTESIAN_POINT('Ctrl Pts',(16.9816699618116,14.2349802268651,0.52834069439712));
#22105=CARTESIAN_POINT('Ctrl Pts',(17.1330265346661,14.4375333640891,0.517510543297487));
#22106=CARTESIAN_POINT('Ctrl Pts',(17.3523384610754,14.8940137703006,0.495729873511439));
#22107=CARTESIAN_POINT('Ctrl Pts',(17.4162475186011,15.1444779569485,0.484995974078288));
#22108=CARTESIAN_POINT('Ctrl Pts',(17.4421185607647,15.6442929462081,0.465768343165624));
#22109=CARTESIAN_POINT('Ctrl Pts',(17.4083000036646,15.8886689108966,0.456344488460597));
#22110=CARTESIAN_POINT('Ctrl Pts',(17.2484328205998,16.3602738340633,0.435280848141696));
#22111=CARTESIAN_POINT('Ctrl Pts',(17.120645735791,16.5819407284765,0.424245033694158));
#22112=CARTESIAN_POINT('Ctrl Pts',(16.7856687237361,16.9645889727935,0.402727812187014));
#22113=CARTESIAN_POINT('Ctrl Pts',(16.5812682860446,17.1213576047524,0.393012028294842));
#22114=CARTESIAN_POINT('Ctrl Pts',(16.1307300452772,17.3428309784573,0.373579510987316));
#22115=CARTESIAN_POINT('Ctrl Pts',(15.8902976974581,17.4082697840059,0.363209235309224));
#22116=CARTESIAN_POINT('Ctrl Pts',(15.388198076337,17.4458200822582,0.341552783770483));
#22117=CARTESIAN_POINT('Ctrl Pts',(15.1310281685985,17.4137884812617,0.330460587302136));
#22118=CARTESIAN_POINT('Ctrl Pts',(14.6530287773331,17.254050494753,0.309843621630324));
#22119=CARTESIAN_POINT('Ctrl Pts',(14.4356759588901,17.1313390171616,0.301024334094614));
#22120=CARTESIAN_POINT('Ctrl Pts',(14.0571971875519,16.8090342642195,0.280822982040742));
#22121=CARTESIAN_POINT('Ctrl Pts',(13.9002426533357,16.6117620421852,0.270069365098247));
#22122=CARTESIAN_POINT('Ctrl Pts',(13.6672548470398,16.1629040885246,0.248278485916038));
#22123=CARTESIAN_POINT('Ctrl Pts',(13.5956339334193,15.9144966794261,0.237455100696454));
#22124=CARTESIAN_POINT('Ctrl Pts',(13.5701259723254,15.606262404414,0.22539145635692));
#22125=CARTESIAN_POINT('Ctrl Pts',(13.5679367061316,15.5531033072491,0.22335857947366));
#22126=CARTESIAN_POINT('Ctrl Pts',(13.5679367061315,15.5000000000003,0.221374999999826));
#22127=CARTESIAN_POINT('Origin',(15.4999999999998,15.5000000000002,11.20575));
#22128=CARTESIAN_POINT('',(13.5679367061315,15.5000000000002,-0.278625000000181));
#22129=CARTESIAN_POINT('',(13.5679367061316,15.5000000000001,0.190124999999878));
#22130=CARTESIAN_POINT('',(13.5679367061315,15.5000000000002,11.20575));
#22131=CARTESIAN_POINT('Ctrl Pts',(13.5679367061316,15.5000000000001,0.190124999999878));
#22132=CARTESIAN_POINT('Ctrl Pts',(13.5679367061315,15.7052232055912,0.197790747375235));
#22133=CARTESIAN_POINT('Ctrl Pts',(13.6006312438211,15.909443124398,0.206124105599977));
#22134=CARTESIAN_POINT('Ctrl Pts',(13.7445092392225,16.3458500952327,0.225528168010872));
#22135=CARTESIAN_POINT('Ctrl Pts',(13.8706006648954,16.5687690249,0.236574181605313));
#22136=CARTESIAN_POINT('Ctrl Pts',(14.1957983248935,16.9462938014509,0.25768912465625));
#22137=CARTESIAN_POINT('Ctrl Pts',(14.3891741439702,17.0996068020763,0.267213101031667));
#22138=CARTESIAN_POINT('Ctrl Pts',(14.8328987043057,17.3312210666005,0.286351732158286));
#22139=CARTESIAN_POINT('Ctrl Pts',(15.0810963874242,17.4033891896782,0.29705694058781));
#22140=CARTESIAN_POINT('Ctrl Pts',(15.5859112111093,17.4463663432178,0.318830503652366));
#22141=CARTESIAN_POINT('Ctrl Pts',(15.8374917549291,17.41880982897,0.32968162089312));
#22142=CARTESIAN_POINT('Ctrl Pts',(16.311441609934,17.2705600347065,0.35012392284861));
#22143=CARTESIAN_POINT('Ctrl Pts',(16.5299161239961,17.1530549287718,0.358922469304605));
#22144=CARTESIAN_POINT('Ctrl Pts',(16.9202726297617,16.8349526369191,0.379222999835996));
#22145=CARTESIAN_POINT('Ctrl Pts',(17.0854512100821,16.6338441663763,0.39029727189277));
#22146=CARTESIAN_POINT('Ctrl Pts',(17.3225641667435,16.1874197433199,0.412086213416689));
#22147=CARTESIAN_POINT('Ctrl Pts',(17.3956324394972,15.9481982603312,0.422597688314598));
#22148=CARTESIAN_POINT('Ctrl Pts',(17.4478128352921,15.4510757841907,0.442292129850948));
#22149=CARTESIAN_POINT('Ctrl Pts',(17.4248413113891,15.197732591562,0.451571409240266));
#22150=CARTESIAN_POINT('Ctrl Pts',(17.2822086107977,14.711734855356,0.472800990486119));
#22151=CARTESIAN_POINT('Ctrl Pts',(17.1630032804554,14.4841033890506,0.48387452771214));
#22152=CARTESIAN_POINT('Ctrl Pts',(16.8491384993419,14.0954494858789,0.505160775836514));
#22153=CARTESIAN_POINT('Ctrl Pts',(16.6603046231694,13.9358452837368,0.51507899362005));
#22154=CARTESIAN_POINT('Ctrl Pts',(16.2236425461118,13.6903827463215,0.533913007255612));
#22155=CARTESIAN_POINT('Ctrl Pts',(15.977849940704,13.6105539996564,0.544514480396965));
#22156=CARTESIAN_POINT('Ctrl Pts',(15.4739117712155,13.551815844132,0.5662502318036));
#22157=CARTESIAN_POINT('Ctrl Pts',(15.2208352901073,13.5717427947095,0.577165871485784));
#22158=CARTESIAN_POINT('Ctrl Pts',(14.7426848689158,13.7057278794306,0.597789351347489));
#22159=CARTESIAN_POINT('Ctrl Pts',(14.5214408844316,13.8161488953135,0.606664573343399));
#22160=CARTESIAN_POINT('Ctrl Pts',(14.1213400688697,14.1219606735906,0.626716158351901));
#22161=CARTESIAN_POINT('Ctrl Pts',(13.9495491173572,14.3185686119022,0.637764922719205));
#22162=CARTESIAN_POINT('Ctrl Pts',(13.6984440207751,14.7590310485604,0.659632917824892));
#22163=CARTESIAN_POINT('Ctrl Pts',(13.6181551918388,14.996695945816,0.670241966963368));
#22164=CARTESIAN_POINT('Ctrl Pts',(13.5736457522817,15.3284077888483,0.683592357862537));
#22165=CARTESIAN_POINT('Ctrl Pts',(13.5679367061315,15.4142441778549,0.686921743980967));
#22166=CARTESIAN_POINT('Ctrl Pts',(13.5679367061315,15.5000000000001,0.690124999999889));
#22167=CARTESIAN_POINT('Ctrl Pts',(13.5679367061315,15.5000000000003,0.221374999999828));
#22168=CARTESIAN_POINT('Ctrl Pts',(13.5679367061315,15.3093450220739,0.214253422825221));
#22169=CARTESIAN_POINT('Ctrl Pts',(13.5961535790968,15.1194546082456,0.206551882570376));
#22170=CARTESIAN_POINT('Ctrl Pts',(13.7256105047228,14.6948718230659,0.187900494778529));
#22171=CARTESIAN_POINT('Ctrl Pts',(13.845972473953,14.4700098902214,0.176905464594504));
#22172=CARTESIAN_POINT('Ctrl Pts',(14.1696924218756,14.075352608936,0.155182435517201));
#22173=CARTESIAN_POINT('Ctrl Pts',(14.3714266001445,13.9107790536386,0.145052382164217));
#22174=CARTESIAN_POINT('Ctrl Pts',(14.8173319840546,13.6758632412697,0.125819688229996));
#22175=CARTESIAN_POINT('Ctrl Pts',(15.0551292054429,13.6037990123974,0.115563070251393));
#22176=CARTESIAN_POINT('Ctrl Pts',(15.5544792852584,13.5518334963225,0.0940252113296194));
#22177=CARTESIAN_POINT('Ctrl Pts',(15.8116932973583,13.5761558231843,0.082931112561566));
#22178=CARTESIAN_POINT('Ctrl Pts',(16.2949297859146,13.7215598037838,0.0620882615496575));
#22179=CARTESIAN_POINT('Ctrl Pts',(16.5170608746999,13.8385708541843,0.0531675695664913));
#22180=CARTESIAN_POINT('Ctrl Pts',(16.9049967005296,14.150596790255,0.0331462146042882));
#22181=CARTESIAN_POINT('Ctrl Pts',(17.0670614605326,14.3427581393122,0.0224732986472017));
#22182=CARTESIAN_POINT('Ctrl Pts',(17.3126898338364,14.7840616508994,0.000691997103376874));
#22183=CARTESIAN_POINT('Ctrl Pts',(17.3915129003429,15.030308881313,-0.0102060193334657));
#22184=CARTESIAN_POINT('Ctrl Pts',(17.4473055261712,15.5280187232032,-0.0300003018310558));
#22185=CARTESIAN_POINT('Ctrl Pts',(17.4281050083514,15.7742335760592,-0.0389538708224634));
#22186=CARTESIAN_POINT('Ctrl Pts',(17.2969077106339,16.2532901707722,-0.0596775634354227));
#22187=CARTESIAN_POINT('Ctrl Pts',(17.1834947937312,16.4808992968809,-0.0706253476255288));
#22188=CARTESIAN_POINT('Ctrl Pts',(16.8732369845877,16.882970778244,-0.0923349979238737));
#22189=CARTESIAN_POINT('Ctrl Pts',(16.6781753241914,17.0524923784484,-0.102808198434923));
#22190=CARTESIAN_POINT('Ctrl Pts',(16.2425026234143,17.3005030646061,-0.121599538508183));
#22191=CARTESIAN_POINT('Ctrl Pts',(16.0080032119515,17.3801675177468,-0.131713916067101));
#22192=CARTESIAN_POINT('Ctrl Pts',(15.512365648488,17.44877246744,-0.153091647541905));
#22193=CARTESIAN_POINT('Ctrl Pts',(15.2553808905635,17.43339955154,-0.164175858168785));
#22194=CARTESIAN_POINT('Ctrl Pts',(14.7662503098183,17.3048200986632,-0.185272931881702));
#22195=CARTESIAN_POINT('Ctrl Pts',(14.5384527981285,17.1944566842457,-0.194401543727441));
#22196=CARTESIAN_POINT('Ctrl Pts',(14.1397272752797,16.8943347847829,-0.214210934032653));
#22197=CARTESIAN_POINT('Ctrl Pts',(13.9720032633974,16.7081889664025,-0.224781197363946));
#22198=CARTESIAN_POINT('Ctrl Pts',(13.7111048248534,16.2741834169149,-0.246619209094661));
#22199=CARTESIAN_POINT('Ctrl Pts',(13.6237773096301,16.028498554785,-0.257679625280961));
#22200=CARTESIAN_POINT('Ctrl Pts',(13.5743830168652,15.6823226737332,-0.271675640774711));
#22201=CARTESIAN_POINT('Ctrl Pts',(13.5679367061315,15.5911253193284,-0.275221175976205));
#22202=CARTESIAN_POINT('Ctrl Pts',(13.5679367061315,15.5000000000002,-0.278625000000181));
#22203=CARTESIAN_POINT('Origin',(15.4999999999998,15.5000000000002,11.20575));
#22204=CARTESIAN_POINT('',(13.5679367061315,15.5000000000002,-0.778625000000188));
#22205=CARTESIAN_POINT('',(13.5679367061315,15.5000000000215,-0.309874999998533));
#22206=CARTESIAN_POINT('',(13.5679367061315,15.5000000000002,11.20575));
#22207=CARTESIAN_POINT('Ctrl Pts',(13.5679367061315,15.5000000000427,-0.309874999998534));
#22208=CARTESIAN_POINT('Ctrl Pts',(13.5679367061369,15.7451189900437,-0.300719016644392));
#22209=CARTESIAN_POINT('Ctrl Pts',(13.6145849104547,15.9880788836299,-0.290637672395828));
#22210=CARTESIAN_POINT('Ctrl Pts',(13.7998506160076,16.4525087353534,-0.269294302322016));
#22211=CARTESIAN_POINT('Ctrl Pts',(13.9401358945743,16.6681650113369,-0.258213469135985));
#22212=CARTESIAN_POINT('Ctrl Pts',(14.2937988135868,17.030051039115,-0.23706880501825));
#22213=CARTESIAN_POINT('Ctrl Pts',(14.5027181075031,17.1737375672255,-0.227889545454423));
#22214=CARTESIAN_POINT('Ctrl Pts',(14.9610456268795,17.3718881645075,-0.208121062677875));
#22215=CARTESIAN_POINT('Ctrl Pts',(15.2056351161719,17.4255568606797,-0.197571482078912));
#22216=CARTESIAN_POINT('Ctrl Pts',(15.7028273877143,17.4374855261911,-0.1761266932738));
#22217=CARTESIAN_POINT('Ctrl Pts',(15.9508283805329,17.3951930471992,-0.165429968447515));
#22218=CARTESIAN_POINT('Ctrl Pts',(16.4162168450068,17.2190375058601,-0.145356934524384));
#22219=CARTESIAN_POINT('Ctrl Pts',(16.6293413959125,17.087177913888,-0.136472617530292));
#22220=CARTESIAN_POINT('Ctrl Pts',(16.9997020048589,16.7447233478946,-0.115693680499858));
#22221=CARTESIAN_POINT('Ctrl Pts',(17.151285984167,16.5352235199722,-0.104599143917318));
#22222=CARTESIAN_POINT('Ctrl Pts',(17.3599329092895,16.0781299074099,-0.0830255691568057));
#22223=CARTESIAN_POINT('Ctrl Pts',(17.4184418092005,15.8364334516317,-0.0727356319076326));
#22224=CARTESIAN_POINT('Ctrl Pts',(17.4419572678442,15.3335771418076,-0.0534451981391343));
#22225=CARTESIAN_POINT('Ctrl Pts',(17.4026393126743,15.0770448720175,-0.0434417100342342));
#22226=CARTESIAN_POINT('Ctrl Pts',(17.2273302215967,14.5982616364446,-0.0217769181316676));
#22227=CARTESIAN_POINT('Ctrl Pts',(17.094621571808,14.3801849192583,-0.0107690704263424));
#22228=CARTESIAN_POINT('Ctrl Pts',(16.7583973031519,14.0137016048738,0.0101712371103755));
#22229=CARTESIAN_POINT('Ctrl Pts',(16.5604348396368,13.8665662971672,0.019386555379266));
#22230=CARTESIAN_POINT('Ctrl Pts',(16.1097762694868,13.6488960345413,0.0388242627075083));
#22231=CARTESIAN_POINT('Ctrl Pts',(15.859413903315,13.584481024699,0.0496228377751859));
#22232=CARTESIAN_POINT('Ctrl Pts',(15.354216020494,13.5572975229281,0.0714129228630083));
#22233=CARTESIAN_POINT('Ctrl Pts',(15.104360020515,13.592429171137,0.0821896574543013));
#22234=CARTESIAN_POINT('Ctrl Pts',(14.634735382139,13.7549549306403,0.102445405107882));
#22235=CARTESIAN_POINT('Ctrl Pts',(14.4190031858108,13.8797188217571,0.11124827499474));
#22236=CARTESIAN_POINT('Ctrl Pts',(14.0387180251792,14.2102312356744,0.131795166002679));
#22237=CARTESIAN_POINT('Ctrl Pts',(13.8803875205855,14.4157066951992,0.142884874300359));
#22238=CARTESIAN_POINT('Ctrl Pts',(13.6576628179055,14.8677637645245,0.164573917775808));
#22239=CARTESIAN_POINT('Ctrl Pts',(13.5919750720433,15.1083498919251,0.174977198896046));
#22240=CARTESIAN_POINT('Ctrl Pts',(13.5697540327489,15.4031822744544,0.186469354010808));
#22241=CARTESIAN_POINT('Ctrl Pts',(13.5679367061315,15.4516175612208,0.188317760160613));
#22242=CARTESIAN_POINT('Ctrl Pts',(13.5679367061315,15.5000000000001,0.190124999999879));
#22243=CARTESIAN_POINT('Ctrl Pts',(13.5679367061315,15.5000000000002,-0.278625000000181));
#22244=CARTESIAN_POINT('Ctrl Pts',(13.5679367061315,15.3467892596533,-0.284347914362165));
#22245=CARTESIAN_POINT('Ctrl Pts',(13.5861582264408,15.193811827971,-0.290455077217825));
#22246=CARTESIAN_POINT('Ctrl Pts',(13.681690372198,14.8002115588649,-0.307217550187096));
#22247=CARTESIAN_POINT('Ctrl Pts',(13.7879612605511,14.5700164470718,-0.318107905057002));
#22248=CARTESIAN_POINT('Ctrl Pts',(14.085411271142,14.1593674322763,-0.339861742252181));
#22249=CARTESIAN_POINT('Ctrl Pts',(14.2752366147309,13.9839732655354,-0.350507031697016));
#22250=CARTESIAN_POINT('Ctrl Pts',(14.7026885544222,13.7231840672578,-0.369466729773054));
#22251=CARTESIAN_POINT('Ctrl Pts',(14.9340075268005,13.6365422675152,-0.379212735876613));
#22252=CARTESIAN_POINT('Ctrl Pts',(15.4259040926485,13.552703568537,-0.400429111456754));
#22253=CARTESIAN_POINT('Ctrl Pts',(15.6824101506341,13.5598498556532,-0.411492674866595));
#22254=CARTESIAN_POINT('Ctrl Pts',(16.1685436046143,13.670873721781,-0.432460477161097));
#22255=CARTESIAN_POINT('Ctrl Pts',(16.3943923192522,13.7700581637479,-0.441627804179568));
#22256=CARTESIAN_POINT('Ctrl Pts',(16.80661287371,14.0539091257136,-0.461120454973073));
#22257=CARTESIAN_POINT('Ctrl Pts',(16.9865111570376,14.2395717539648,-0.471935218610241));
#22258=CARTESIAN_POINT('Ctrl Pts',(17.2601171115597,14.6649766984353,-0.493726018963056));
#22259=CARTESIAN_POINT('Ctrl Pts',(17.3532344935082,14.8993253047808,-0.504487853138082));
#22260=CARTESIAN_POINT('Ctrl Pts',(17.4445879148985,15.3879151899874,-0.524708376140794));
#22261=CARTESIAN_POINT('Ctrl Pts',(17.442965528729,15.6373703516649,-0.533521108441911));
#22262=CARTESIAN_POINT('Ctrl Pts',(17.3439130072936,16.1314699146203,-0.55411347359851));
#22263=CARTESIAN_POINT('Ctrl Pts',(17.2437932712051,16.3705992587551,-0.565204895727018));
#22264=CARTESIAN_POINT('Ctrl Pts',(16.9614315560074,16.7876645307058,-0.586873008246029));
#22265=CARTESIAN_POINT('Ctrl Pts',(16.7850271273137,16.9637580968302,-0.597254988519727));
#22266=CARTESIAN_POINT('Ctrl Pts',(16.3689556310297,17.2443400455292,-0.616708580136453));
#22267=CARTESIAN_POINT('Ctrl Pts',(16.1315609716315,17.3436265738683,-0.626384649678148));
#22268=CARTESIAN_POINT('Ctrl Pts',(15.6332086943346,17.4440644805243,-0.647879471598956));
#22269=CARTESIAN_POINT('Ctrl Pts',(15.3772600498225,17.4447534368266,-0.658918992807723));
#22270=CARTESIAN_POINT('Ctrl Pts',(14.8884838634483,17.3489811388447,-0.680000780859792));
#22271=CARTESIAN_POINT('Ctrl Pts',(14.6596166091818,17.2568181638627,-0.6894591361531));
#22272=CARTESIAN_POINT('Ctrl Pts',(14.2388050989207,16.9858620066354,-0.7086553960968));
#22273=CARTESIAN_POINT('Ctrl Pts',(14.0532686229962,16.8058878840209,-0.719379268383982));
#22274=CARTESIAN_POINT('Ctrl Pts',(13.7662002685901,16.3885881552,-0.741157641490634));
#22275=CARTESIAN_POINT('Ctrl Pts',(13.6656892249804,16.1564785083478,-0.751995294223503));
#22276=CARTESIAN_POINT('Ctrl Pts',(13.5827427725009,15.7761115115987,-0.767992040179092));
#22277=CARTESIAN_POINT('Ctrl Pts',(13.5679367061315,15.6381065099785,-0.773466277265415));
#22278=CARTESIAN_POINT('Ctrl Pts',(13.5679367061315,15.5000000000002,-0.778625000000189));
#22279=CARTESIAN_POINT('Origin',(15.4999999999998,15.5000000000002,11.20575));
#22280=CARTESIAN_POINT('',(13.5679367061315,15.5000000000001,-1.2786250000002));
#22281=CARTESIAN_POINT('',(13.5679367061315,15.5000000000002,-0.809875000000126));
#22282=CARTESIAN_POINT('',(13.5679367061315,15.5000000000002,11.20575));
#22283=CARTESIAN_POINT('Ctrl Pts',(13.5679367061315,15.5000000000003,-0.809875000000126));
#22284=CARTESIAN_POINT('Ctrl Pts',(13.5679367061316,15.5387848588904,-0.808426260665874));
#22285=CARTESIAN_POINT('Ctrl Pts',(13.5691045537608,15.5776081217821,-0.806950901143693));
#22286=CARTESIAN_POINT('Ctrl Pts',(13.5863172258652,15.8627498107998,-0.795928734529088));
#22287=CARTESIAN_POINT('Ctrl Pts',(13.6482441649584,16.1039441624046,-0.785583839426238));
#22288=CARTESIAN_POINT('Ctrl Pts',(13.8636040208233,16.5586938389718,-0.763953047887043));
#22289=CARTESIAN_POINT('Ctrl Pts',(14.0184106751403,16.7663048606795,-0.752859564438586));
#22290=CARTESIAN_POINT('Ctrl Pts',(14.3935142993231,17.1030886658294,-0.732190161230492));
#22291=CARTESIAN_POINT('Ctrl Pts',(14.6078734364705,17.2315636886463,-0.723354008700334));
#22292=CARTESIAN_POINT('Ctrl Pts',(15.0752831240914,17.4012591024431,-0.703193795820476));
#22293=CARTESIAN_POINT('Ctrl Pts',(15.3241884796655,17.4401670421019,-0.692458064216684));
#22294=CARTESIAN_POINT('Ctrl Pts',(15.8293918059363,17.4209116308136,-0.67066774434319));
#22295=CARTESIAN_POINT('Ctrl Pts',(16.0807480284636,17.3604173282469,-0.659826302479593));
#22296=CARTESIAN_POINT('Ctrl Pts',(16.5348352725854,17.1497816929783,-0.640240710332137));
#22297=CARTESIAN_POINT('Ctrl Pts',(16.7351193667875,17.0057085011961,-0.631148276498336));
#22298=CARTESIAN_POINT('Ctrl Pts',(17.0767669839638,16.6447314320374,-0.61029668560251));
#22299=CARTESIAN_POINT('Ctrl Pts',(17.2126942752492,16.4291281586245,-0.599311816112398));
#22300=CARTESIAN_POINT('Ctrl Pts',(17.3960714153677,15.9522914740598,-0.577545739488941));
#22301=CARTESIAN_POINT('Ctrl Pts',(17.4394863853224,15.6949512567246,-0.567317142600507));
#22302=CARTESIAN_POINT('Ctrl Pts',(17.422969090324,15.1907605692907,-0.548127787168051));
#22303=CARTESIAN_POINT('Ctrl Pts',(17.3679857370148,14.9485965706548,-0.537896417242269));
#22304=CARTESIAN_POINT('Ctrl Pts',(17.1662821041939,14.4891878782663,-0.516386105083552));
#22305=CARTESIAN_POINT('Ctrl Pts',(17.0180420352627,14.2777915836234,-0.505292843771136));
#22306=CARTESIAN_POINT('Ctrl Pts',(16.6526099917284,13.9295152530064,-0.484402733995948));
#22307=CARTESIAN_POINT('Ctrl Pts',(16.4407479085024,13.7941507738711,-0.47545113396572));
#22308=CARTESIAN_POINT('Ctrl Pts',(15.9774528011727,13.6113838875223,-0.45546839026713));
#22309=CARTESIAN_POINT('Ctrl Pts',(15.7304237057033,13.5656468617912,-0.444813585105653));
#22310=CARTESIAN_POINT('Ctrl Pts',(15.2255315160606,13.5704710073907,-0.423036685109443));
#22311=CARTESIAN_POINT('Ctrl Pts',(14.9725259783177,13.6237792291612,-0.412124105341057));
#22312=CARTESIAN_POINT('Ctrl Pts',(14.5122846645605,13.821533642873,-0.392273077201959));
#22313=CARTESIAN_POINT('Ctrl Pts',(14.3077326406345,13.9600852553975,-0.383350131532067));
#22314=CARTESIAN_POINT('Ctrl Pts',(13.9563854884096,14.3110923296951,-0.362661772922356));
#22315=CARTESIAN_POINT('Ctrl Pts',(13.8147703346549,14.5221235135245,-0.351725021873652));
#22316=CARTESIAN_POINT('Ctrl Pts',(13.6188695990393,14.9904064163151,-0.330008374038293));
#22317=CARTESIAN_POINT('Ctrl Pts',(13.5679791180273,15.2437584839144,-0.31944736015892));
#22318=CARTESIAN_POINT('Ctrl Pts',(13.567936714964,15.4997866765028,-0.309882968509927));
#22319=CARTESIAN_POINT('Ctrl Pts',(13.5679367061315,15.4998933384701,-0.309878984151632));
#22320=CARTESIAN_POINT('Ctrl Pts',(13.5679367061315,15.5000000000427,-0.309874999998532));
#22321=CARTESIAN_POINT('Ctrl Pts',(13.5679367061316,15.5000000000002,-0.778625000000188));
#22322=CARTESIAN_POINT('Ctrl Pts',(13.5679367061316,15.3931460599276,-0.782616338641927));
#22323=CARTESIAN_POINT('Ctrl Pts',(13.5768002208671,15.2862458064669,-0.786800556831684));
#22324=CARTESIAN_POINT('Ctrl Pts',(13.6371564581937,14.9264097347141,-0.801543228525542));
#22325=CARTESIAN_POINT('Ctrl Pts',(13.7301105173089,14.6835020774024,-0.812621248604655));
#22326=CARTESIAN_POINT('Ctrl Pts',(14.0004851885106,14.2567488545141,-0.834392725992354));
#22327=CARTESIAN_POINT('Ctrl Pts',(14.172061764955,14.0749328110024,-0.844884342281997));
#22328=CARTESIAN_POINT('Ctrl Pts',(14.5783544244189,13.7832732836059,-0.864540827793249));
#22329=CARTESIAN_POINT('Ctrl Pts',(14.8102645188579,13.6776776439952,-0.873875479399929));
#22330=CARTESIAN_POINT('Ctrl Pts',(15.3034623334679,13.5612057991712,-0.895147980158364));
#22331=CARTESIAN_POINT('Ctrl Pts',(15.5600993607178,13.5521973966187,-0.906217192541493));
#22332=CARTESIAN_POINT('Ctrl Pts',(16.0528776433435,13.632593459332,-0.92747159813772));
#22333=CARTESIAN_POINT('Ctrl Pts',(16.2849105085688,13.7176559737471,-0.937309340881192));
#22334=CARTESIAN_POINT('Ctrl Pts',(16.7142424067725,13.9755352340427,-0.956200886386672));
#22335=CARTESIAN_POINT('Ctrl Pts',(16.9052695294522,14.1496041204308,-0.966822589781085));
#22336=CARTESIAN_POINT('Ctrl Pts',(17.2056519898425,14.5583089437818,-0.98856704606031));
#22337=CARTESIAN_POINT('Ctrl Pts',(17.3135593941965,14.7879324231272,-0.999471341544057));
#22338=CARTESIAN_POINT('Ctrl Pts',(17.4338950578462,15.2696786468988,-1.02006125964282));
#22339=CARTESIAN_POINT('Ctrl Pts',(17.4474891140461,15.5166980415326,-1.02891605404637));
#22340=CARTESIAN_POINT('Ctrl Pts',(17.3798092847476,16.0156874197882,-1.04901448948222));
#22341=CARTESIAN_POINT('Ctrl Pts',(17.2940873361283,16.262135211793,-1.06006877808074));
#22342=CARTESIAN_POINT('Ctrl Pts',(17.0359029314218,16.6981549442992,-1.0819234954729));
#22343=CARTESIAN_POINT('Ctrl Pts',(16.869287872015,16.8855107790962,-1.09251504126423));
#22344=CARTESIAN_POINT('Ctrl Pts',(16.4727055987813,17.1880123647539,-1.11236709942155));
#22345=CARTESIAN_POINT('Ctrl Pts',(16.2460520789443,17.2997096590906,-1.12144644416506));
#22346=CARTESIAN_POINT('Ctrl Pts',(15.7580841554065,17.4316717914015,-1.14249337040046));
#22347=CARTESIAN_POINT('Ctrl Pts',(15.5010293354052,17.4488346169962,-1.15358060292959));
#22348=CARTESIAN_POINT('Ctrl Pts',(15.0046042923773,17.3835494184043,-1.1749922998015));
#22349=CARTESIAN_POINT('Ctrl Pts',(14.7694246897996,17.3053971665795,-1.18513601521548));
#22350=CARTESIAN_POINT('Ctrl Pts',(14.3319804118993,17.0601513562503,-1.20400376656747));
#22351=CARTESIAN_POINT('Ctrl Pts',(14.1358043639573,16.8918928499191,-1.21438674923931));
#22352=CARTESIAN_POINT('Ctrl Pts',(13.822828452168,16.4917126942036,-1.23608437074198));
#22353=CARTESIAN_POINT('Ctrl Pts',(13.7078902728498,16.2646868047079,-1.24704326281027));
#22354=CARTESIAN_POINT('Ctrl Pts',(13.5920235017753,15.8517814523629,-1.26496537710061));
#22355=CARTESIAN_POINT('Ctrl Pts',(13.5679367061315,15.6761515069574,-1.27204517415529));
#22356=CARTESIAN_POINT('Ctrl Pts',(13.5679367061315,15.5000000000001,-1.2786250000002));
#22357=CARTESIAN_POINT('Origin',(15.4999999999998,15.5000000000002,11.20575));
#22358=CARTESIAN_POINT('',(13.5679367061315,15.5000000000002,-1.7786250000002));
#22359=CARTESIAN_POINT('',(13.5679367061315,15.5000000000002,-1.30987500000013));
#22360=CARTESIAN_POINT('',(13.5679367061315,15.5000000000002,11.20575));
#22361=CARTESIAN_POINT('',(13.936917323708,16.6356236642094,-2.22824839960636));
#22362=CARTESIAN_POINT('Ctrl Pts',(13.5679367061315,15.5000000000002,-1.7786250000002));
#22363=CARTESIAN_POINT('Ctrl Pts',(13.5679367061315,15.4713110102307,-1.77969662612257));
#22364=CARTESIAN_POINT('Ctrl Pts',(13.5685756992797,15.4425999920107,-1.78078285553511));
#22365=CARTESIAN_POINT('Ctrl Pts',(13.5812658327813,15.1581590397254,-1.79168131480178));
#22366=CARTESIAN_POINT('Ctrl Pts',(13.6433835357949,14.9072543396241,-1.80239303667409));
#22367=CARTESIAN_POINT('Ctrl Pts',(13.8594981526188,14.449071217981,-1.82416835553235));
#22368=CARTESIAN_POINT('Ctrl Pts',(14.0095359245601,14.2453192500445,-1.83501484570138));
#22369=CARTESIAN_POINT('Ctrl Pts',(14.375576771222,13.9097095423591,-1.85544494571614));
#22370=CARTESIAN_POINT('Ctrl Pts',(14.5868970847757,13.7796534963394,-1.86424124386568));
#22371=CARTESIAN_POINT('Ctrl Pts',(15.057940686529,13.6016248095225,-1.8845581939387));
#22372=CARTESIAN_POINT('Ctrl Pts',(15.3147261183979,13.5596639922916,-1.89563380727755));
#22373=CARTESIAN_POINT('Ctrl Pts',(15.8197591254003,13.5785378998179,-1.91741678097743));
#22374=CARTESIAN_POINT('Ctrl Pts',(16.0633065479973,13.6353374704203,-1.9279214153826));
#22375=CARTESIAN_POINT('Ctrl Pts',(16.519613232597,13.8396294895299,-1.94760273595353));
#22376=CARTESIAN_POINT('Ctrl Pts',(16.7273518610523,13.9867054191127,-1.95690084582151));
#22377=CARTESIAN_POINT('Ctrl Pts',(17.0761951409432,14.3540458830506,-1.97814531087592));
#22378=CARTESIAN_POINT('Ctrl Pts',(17.2132390449659,14.5713394120571,-1.98921739760241));
#22379=CARTESIAN_POINT('Ctrl Pts',(17.3918917772879,15.0377637906816,-2.0104926550159));
#22380=CARTESIAN_POINT('Ctrl Pts',(17.4351931175485,15.281149046348,-2.02038271492798));
#22381=CARTESIAN_POINT('Ctrl Pts',(17.4284331863123,15.7819930618869,-2.039236635147));
#22382=CARTESIAN_POINT('Ctrl Pts',(17.3741617365723,16.034664555002,-2.04984514098204));
#22383=CARTESIAN_POINT('Ctrl Pts',(17.1721421783683,16.500008983052,-2.07158398518824));
#22384=CARTESIAN_POINT('Ctrl Pts',(17.0279622253633,16.7088902827345,-2.08249574332465));
#22385=CARTESIAN_POINT('Ctrl Pts',(16.6721862678626,17.0552935072645,-2.10310764445746));
#22386=CARTESIAN_POINT('Ctrl Pts',(16.4656337930884,17.191302469683,-2.11197549347892));
#22387=CARTESIAN_POINT('Ctrl Pts',(16.0003669871892,17.3839588971004,-2.13204328005094));
#22388=CARTESIAN_POINT('Ctrl Pts',(15.7441588927643,17.4339176130858,-2.14309399179686));
#22389=CARTESIAN_POINT('Ctrl Pts',(15.2372592427903,17.4301770605375,-2.164957477135));
#22390=CARTESIAN_POINT('Ctrl Pts',(14.9914303045821,17.3804225882126,-2.17556051737478));
#22391=CARTESIAN_POINT('Ctrl Pts',(14.6006806201442,17.2188593063065,-2.19241424768811));
#22392=CARTESIAN_POINT('Ctrl Pts',(14.4493679379594,17.1307744676622,-2.19870147391655));
#22393=CARTESIAN_POINT('Ctrl Pts',(14.1693732821569,16.9124347548744,-2.21289549932602));
#22394=CARTESIAN_POINT('Ctrl Pts',(14.0431460179899,16.7818378044134,-2.22049591927601));
#22395=CARTESIAN_POINT('Ctrl Pts',(13.9369173213454,16.6356236661871,-2.22824840453314));
#22396=CARTESIAN_POINT('',(13.9369188502118,16.6356257705296,-1.75949829183043));
#22397=CARTESIAN_POINT('',(13.9369184637306,16.6356252385746,-1.75949832116282));
#22398=CARTESIAN_POINT('Ctrl Pts',(13.9369188502402,16.6356257705687,-1.75949829295567));
#22399=CARTESIAN_POINT('Ctrl Pts',(14.0732165037117,16.8232265616208,-1.74955141913567));
#22400=CARTESIAN_POINT('Ctrl Pts',(14.2421926306503,16.9847823163708,-1.73987267086338));
#22401=CARTESIAN_POINT('Ctrl Pts',(14.6256885475373,17.2378815903649,-1.72214816701704));
#22402=CARTESIAN_POINT('Ctrl Pts',(14.8362794639394,17.3287014043758,-1.71350244965322));
#22403=CARTESIAN_POINT('Ctrl Pts',(15.3036899854226,17.4385845729923,-1.69334220080739));
#22404=CARTESIAN_POINT('Ctrl Pts',(15.5584934383084,17.4476198869582,-1.68235207375451));
#22405=CARTESIAN_POINT('Ctrl Pts',(16.0626255591007,17.3662648208194,-1.6606079568825));
#22406=CARTESIAN_POINT('Ctrl Pts',(16.3065929189333,17.274502945701,-1.65043016901725));
#22407=CARTESIAN_POINT('Ctrl Pts',(16.733960549226,17.0069230177967,-1.63121863353652));
#22408=CARTESIAN_POINT('Ctrl Pts',(16.9157196559872,16.8376064327553,-1.6209743169182));
#22409=CARTESIAN_POINT('Ctrl Pts',(17.2115388605543,16.4321558772132,-1.59944982869598));
#22410=CARTESIAN_POINT('Ctrl Pts',(17.3197729456465,16.197649200397,-1.58835608490567));
#22411=CARTESIAN_POINT('Ctrl Pts',(17.4370349875305,15.7067373188981,-1.56749008537747));
#22412=CARTESIAN_POINT('Ctrl Pts',(17.4475319697598,15.4557223788833,-1.55855468409504));
#22413=CARTESIAN_POINT('Ctrl Pts',(17.3726902789251,14.9634366275315,-1.53855219877789));
#22414=CARTESIAN_POINT('Ctrl Pts',(17.2880297167384,14.7268219856976,-1.52788809973701));
#22415=CARTESIAN_POINT('Ctrl Pts',(17.0300046441306,14.2927306055598,-1.5061088486522));
#22416=CARTESIAN_POINT('Ctrl Pts',(16.8567343671547,14.1008202908097,-1.49520365267544));
#22417=CARTESIAN_POINT('Ctrl Pts',(16.4544579219332,13.8024087055848,-1.47538156930746));
#22418=CARTESIAN_POINT('Ctrl Pts',(16.2319055093252,13.6952482164326,-1.4664433890746));
#22419=CARTESIAN_POINT('Ctrl Pts',(15.7518323297936,13.5679372308724,-1.44573697721879));
#22420=CARTESIAN_POINT('Ctrl Pts',(15.4981347275305,13.551596272361,-1.43479454747419));
#22421=CARTESIAN_POINT('Ctrl Pts',(14.9946779887316,13.6177050294597,-1.41307956103124));
#22422=CARTESIAN_POINT('Ctrl Pts',(14.7500889892401,13.7011232772005,-1.40256300391617));
#22423=CARTESIAN_POINT('Ctrl Pts',(14.3167686917906,13.9530518157521,-1.3838077236402));
#22424=CARTESIAN_POINT('Ctrl Pts',(14.1300765218336,14.1156697545303,-1.37370723711996));
#22425=CARTESIAN_POINT('Ctrl Pts',(13.8216873535974,14.5094994028654,-1.35234574472338));
#22426=CARTESIAN_POINT('Ctrl Pts',(13.7058009544624,14.7392900935939,-1.34126312922336));
#22427=CARTESIAN_POINT('Ctrl Pts',(13.591360276372,15.1530393767012,-1.32334024636834));
#22428=CARTESIAN_POINT('Ctrl Pts',(13.5679367061315,15.3262907155804,-1.31636360097137));
#22429=CARTESIAN_POINT('Ctrl Pts',(13.5679367061315,15.5000000000003,-1.30987500000013));
#22430=CARTESIAN_POINT('Origin',(15.5,-15.5,11.20575));
#22431=CARTESIAN_POINT('',(15.5,-13.5679367061317,1.22137499999989));
#22432=CARTESIAN_POINT('',(15.5,-13.5679367061317,1.3858));
#22433=CARTESIAN_POINT('',(15.5,-13.5679367061317,11.20575));
#22434=CARTESIAN_POINT('',(17.2021646372135,-16.4140591443298,1.3857999999999));
#22435=CARTESIAN_POINT('Origin',(15.5,-15.5,1.3858));
#22436=CARTESIAN_POINT('Ctrl Pts',(17.2021646372131,-16.4140591443306,1.38579999999995));
#22437=CARTESIAN_POINT('Ctrl Pts',(17.2835044921692,-16.2625877372984,1.3792667682509));
#22438=CARTESIAN_POINT('Ctrl Pts',(17.3442533198926,-16.1009564770173,1.37229532392361));
#22439=CARTESIAN_POINT('Ctrl Pts',(17.4225863575886,-15.7606826337724,1.35761870660277));
#22440=CARTESIAN_POINT('Ctrl Pts',(17.4383899414388,-15.583279243606,1.3499669822032));
#22441=CARTESIAN_POINT('Ctrl Pts',(17.4173618065871,-15.150545952148,1.33130242409274));
#22442=CARTESIAN_POINT('Ctrl Pts',(17.354246909013,-14.8998465932948,1.32048931393011));
#22443=CARTESIAN_POINT('Ctrl Pts',(17.1389102320616,-14.4480453999454,1.30100232322681));
#22444=CARTESIAN_POINT('Ctrl Pts',(16.9927945769671,-14.2493134357546,1.29183017937045));
#22445=CARTESIAN_POINT('Ctrl Pts',(16.6281426362718,-13.9112799548102,1.27091926226126));
#22446=CARTESIAN_POINT('Ctrl Pts',(16.410884372517,-13.7774947329751,1.25991876919078));
#22447=CARTESIAN_POINT('Ctrl Pts',(15.9581594815713,-13.6089622530652,1.23937348400477));
#22448=CARTESIAN_POINT('Ctrl Pts',(15.7298816359758,-13.5679367061317,1.22996181912958));
#22449=CARTESIAN_POINT('Ctrl Pts',(15.5,-13.5679367061317,1.22137499999989));
#22450=CARTESIAN_POINT('Origin',(15.5,-15.5,11.20575));
#22451=CARTESIAN_POINT('',(15.5,-13.5679367061317,0.721374999999882));
#22452=CARTESIAN_POINT('',(15.5,-13.5679367061317,1.19012499999984));
#22453=CARTESIAN_POINT('',(15.5,-13.5679367061317,11.20575));
#22454=CARTESIAN_POINT('',(16.7089831815964,-17.0070594673503,1.3858));
#22455=CARTESIAN_POINT('Ctrl Pts',(15.5,-13.5679367061317,1.19012499999984));
#22456=CARTESIAN_POINT('Ctrl Pts',(15.6209597157618,-13.5679367061317,1.19464323477234));
#22457=CARTESIAN_POINT('Ctrl Pts',(15.7419184750194,-13.5792946957063,1.19940637898293));
#22458=CARTESIAN_POINT('Ctrl Pts',(16.1137167329605,-13.6500674067386,1.21482051737712));
#22459=CARTESIAN_POINT('Ctrl Pts',(16.3540308512701,-13.7479960405399,1.22590894156164));
#22460=CARTESIAN_POINT('Ctrl Pts',(16.7741136008819,-14.026702340501,1.24761093429799));
#22461=CARTESIAN_POINT('Ctrl Pts',(16.9519823816307,-14.2016401214962,1.258027594988));
#22462=CARTESIAN_POINT('Ctrl Pts',(17.2359894885833,-14.6147032779413,1.27754424976214));
#22463=CARTESIAN_POINT('Ctrl Pts',(17.3372359040119,-14.8503902891215,1.28710617538617));
#22464=CARTESIAN_POINT('Ctrl Pts',(17.4426537117389,-15.3471703745469,1.30853318586947));
#22465=CARTESIAN_POINT('Ctrl Pts',(17.4459126157984,-15.6033601229582,1.31958310631912));
#22466=CARTESIAN_POINT('Ctrl Pts',(17.357744835181,-16.0780177664297,1.34005593645267));
#22467=CARTESIAN_POINT('Ctrl Pts',(17.2762233318702,-16.2939199281608,1.34923226468177));
#22468=CARTESIAN_POINT('Ctrl Pts',(17.0408566361002,-16.6881134566224,1.36652510317405));
#22469=CARTESIAN_POINT('Ctrl Pts',(16.8884973676933,-16.8630507957942,1.37598889193056));
#22470=CARTESIAN_POINT('Ctrl Pts',(16.7089831815964,-17.0070594673503,1.38579999999999));
#22471=CARTESIAN_POINT('Origin',(15.5,-15.5,1.3858));
#22472=CARTESIAN_POINT('Ctrl Pts',(15.5,-13.5679367061317,1.22137499999989));
#22473=CARTESIAN_POINT('Ctrl Pts',(15.4729341637143,-13.5679367061317,1.22036400388534));
#22474=CARTESIAN_POINT('Ctrl Pts',(15.4458469977579,-13.5685054395913,1.2193399457951));
#22475=CARTESIAN_POINT('Ctrl Pts',(15.1726369387374,-13.5800041737923,1.20888669013352));
#22476=CARTESIAN_POINT('Ctrl Pts',(14.9307787644431,-13.6373364196089,1.19861608777127));
#22477=CARTESIAN_POINT('Ctrl Pts',(14.4729009299767,-13.8436681823131,1.17706314833877));
#22478=CARTESIAN_POINT('Ctrl Pts',(14.2627623231917,-13.9941383691091,1.16596877123743));
#22479=CARTESIAN_POINT('Ctrl Pts',(13.9183617245921,-14.3628583035511,1.14515252623231));
#22480=CARTESIAN_POINT('Ctrl Pts',(13.7853340431921,-14.5755603823523,1.13624772831502));
#22481=CARTESIAN_POINT('Ctrl Pts',(13.6069662800139,-15.0402511769473,1.11620478613719));
#22482=CARTESIAN_POINT('Ctrl Pts',(13.563518985263,-15.2879321565451,1.10552186405143));
#22483=CARTESIAN_POINT('Ctrl Pts',(13.5731954041822,-15.7929752639186,1.08373845470453));
#22484=CARTESIAN_POINT('Ctrl Pts',(13.628926931347,-16.0454493143052,1.07284879893307));
#22485=CARTESIAN_POINT('Ctrl Pts',(13.8310245097158,-16.5036338505738,1.05308648327279));
#22486=CARTESIAN_POINT('Ctrl Pts',(13.9714260897244,-16.7067442547807,1.0441143077112));
#22487=CARTESIAN_POINT('Ctrl Pts',(14.3257784403693,-17.0548537163586,1.02337081594498));
#22488=CARTESIAN_POINT('Ctrl Pts',(14.5383567467269,-17.1945806683055,1.01241699564406));
#22489=CARTESIAN_POINT('Ctrl Pts',(15.0088443360005,-17.3860429606324,0.990713714656131));
#22490=CARTESIAN_POINT('Ctrl Pts',(15.2627143703035,-17.4344332046964,0.980289491368659));
#22491=CARTESIAN_POINT('Ctrl Pts',(15.764107690538,-17.4296140644544,0.961456907738265));
#22492=CARTESIAN_POINT('Ctrl Pts',(16.0069337839783,-17.3804673298746,0.951326678324261));
#22493=CARTESIAN_POINT('Ctrl Pts',(16.4699471299709,-17.1903012304531,0.929930537938738));
#22494=CARTESIAN_POINT('Ctrl Pts',(16.6843681043685,-17.0476412723927,0.918844635164113));
#22495=CARTESIAN_POINT('Ctrl Pts',(17.0422253707064,-16.6904570711204,0.897774518665517));
#22496=CARTESIAN_POINT('Ctrl Pts',(17.1834288053771,-16.4806668481729,0.888672908979973));
#22497=CARTESIAN_POINT('Ctrl Pts',(17.3770350149237,-16.0208578484158,0.868840527314208));
#22498=CARTESIAN_POINT('Ctrl Pts',(17.42837351161,-15.7755220883528,0.858258758726811));
#22499=CARTESIAN_POINT('Ctrl Pts',(17.4355092606312,-15.2690019284845,0.836411641473291));
#22500=CARTESIAN_POINT('Ctrl Pts',(17.3873412235869,-15.0126438266187,0.825354459639089));
#22501=CARTESIAN_POINT('Ctrl Pts',(17.1979533839632,-14.5460700127244,0.805230299482811));
#22502=CARTESIAN_POINT('Ctrl Pts',(17.063281790105,-14.3384565933621,0.796385555323458));
#22503=CARTESIAN_POINT('Ctrl Pts',(16.7193021674531,-13.9803614873582,0.775814169018619));
#22504=CARTESIAN_POINT('Ctrl Pts',(16.5115619839701,-13.8348471766509,0.764916258632763));
#22505=CARTESIAN_POINT('Ctrl Pts',(16.0477927715656,-13.6296318245785,0.743167333659146));
#22506=CARTESIAN_POINT('Ctrl Pts',(15.7954972631553,-13.5735885359089,0.732534660777732));
#22507=CARTESIAN_POINT('Ctrl Pts',(15.5263956112966,-13.568071880497,0.722363876209219));
#22508=CARTESIAN_POINT('Ctrl Pts',(15.5131950985184,-13.5679367061317,0.721867879406689));
#22509=CARTESIAN_POINT('Ctrl Pts',(15.5,-13.5679367061317,0.721374999999882));
#22510=CARTESIAN_POINT('Origin',(15.5,-15.5,11.20575));
#22511=CARTESIAN_POINT('',(15.5000000000001,-13.5679367061317,0.22137499999988));
#22512=CARTESIAN_POINT('',(15.5,-13.5679367061317,0.690124999999829));
#22513=CARTESIAN_POINT('',(15.5,-13.5679367061317,11.20575));
#22514=CARTESIAN_POINT('Ctrl Pts',(15.4999999999999,-13.5679367061317,0.69012499999983));
#22515=CARTESIAN_POINT('Ctrl Pts',(15.663197634803,-13.5679367061317,0.696220957019176));
#22516=CARTESIAN_POINT('Ctrl Pts',(15.8260698424807,-13.5886111528802,0.702750621155672));
#22517=CARTESIAN_POINT('Ctrl Pts',(16.2318407735952,-13.6937750358444,0.720175424526367));
#22518=CARTESIAN_POINT('Ctrl Pts',(16.4638288993578,-13.8061679673983,0.731264781557265));
#22519=CARTESIAN_POINT('Ctrl Pts',(16.8630470507188,-14.108833797682,0.75270412300508));
#22520=CARTESIAN_POINT('Ctrl Pts',(17.028761444196,-14.2932884830899,0.762872018728106));
#22521=CARTESIAN_POINT('Ctrl Pts',(17.2874053587738,-14.7231251438683,0.781803012187292));
#22522=CARTESIAN_POINT('Ctrl Pts',(17.3745003706305,-14.9664736216104,0.79211305640892));
#22523=CARTESIAN_POINT('Ctrl Pts',(17.4482099203794,-15.4692792372004,0.813799958747375));
#22524=CARTESIAN_POINT('Ctrl Pts',(17.4355847239787,-15.723565875171,0.824767794651858));
#22525=CARTESIAN_POINT('Ctrl Pts',(17.3151733744223,-16.2055976541615,0.845558684393085));
#22526=CARTESIAN_POINT('Ctrl Pts',(17.2113496874164,-16.4295122772777,0.854579673980927));
#22527=CARTESIAN_POINT('Ctrl Pts',(16.9190154733788,-16.8359718966524,0.874264961849426));
#22528=CARTESIAN_POINT('Ctrl Pts',(16.7296891979234,-17.0120418978351,0.885134014187554));
#22529=CARTESIAN_POINT('Ctrl Pts',(16.2991617620683,-17.2766178136154,0.906921415251217));
#22530=CARTESIAN_POINT('Ctrl Pts',(16.0634585876014,-17.3648212635817,0.917627873583943));
#22531=CARTESIAN_POINT('Ctrl Pts',(15.5727030691474,-17.4465792698414,0.93772235628183));
#22532=CARTESIAN_POINT('Ctrl Pts',(15.3223565583377,-17.4398199793547,0.946593274573899));
#22533=CARTESIAN_POINT('Ctrl Pts',(14.8300711076984,-17.3302144103329,0.967345462670997));
#22534=CARTESIAN_POINT('Ctrl Pts',(14.5935881752468,-17.2253688342268,0.978439949755269));
#22535=CARTESIAN_POINT('Ctrl Pts',(14.1832015334446,-16.9351538432142,1.00002795682994));
#22536=CARTESIAN_POINT('Ctrl Pts',(14.0110153602745,-16.755615830377,1.01033156193278));
#22537=CARTESIAN_POINT('Ctrl Pts',(13.7379425524706,-16.3329965553295,1.02964587164791));
#22538=CARTESIAN_POINT('Ctrl Pts',(13.6429845085471,-16.0918227958046,1.03959862802551));
#22539=CARTESIAN_POINT('Ctrl Pts',(13.5535333316269,-15.5900949475556,1.06123904433767));
#22540=CARTESIAN_POINT('Ctrl Pts',(13.5584675814187,-15.3347633934782,1.07225194933617));
#22541=CARTESIAN_POINT('Ctrl Pts',(13.6646353766633,-14.8487842127048,1.09321309755165));
#22542=CARTESIAN_POINT('Ctrl Pts',(13.761672278608,-14.6220240391691,1.10246053097514));
#22543=CARTESIAN_POINT('Ctrl Pts',(14.041585270235,-14.2071591450873,1.12186311344001));
#22544=CARTESIAN_POINT('Ctrl Pts',(14.2255255819044,-14.0255156909769,1.13265117917155));
#22545=CARTESIAN_POINT('Ctrl Pts',(14.648495420734,-13.74776419308,1.1544404228268));
#22546=CARTESIAN_POINT('Ctrl Pts',(14.8821830753995,-13.6523788496886,1.16522647893842));
#22547=CARTESIAN_POINT('Ctrl Pts',(15.2505243179915,-13.5800170676889,1.18054575641211));
#22548=CARTESIAN_POINT('Ctrl Pts',(15.3752528162562,-13.5679367061317,1.18546529110574));
#22549=CARTESIAN_POINT('Ctrl Pts',(15.5,-13.5679367061317,1.19012499999984));
#22550=CARTESIAN_POINT('Ctrl Pts',(15.5,-13.5679367061317,0.721374999999882));
#22551=CARTESIAN_POINT('Ctrl Pts',(15.2685828063486,-13.5679367061317,0.712730822847808));
#22552=CARTESIAN_POINT('Ctrl Pts',(15.0388969708039,-13.6095133452991,0.703254680220421));
#22553=CARTESIAN_POINT('Ctrl Pts',(14.5838672575743,-13.7800568344395,0.682579933296358));
#22554=CARTESIAN_POINT('Ctrl Pts',(14.3657373188852,-13.9154007888411,0.67151326490416));
#22555=CARTESIAN_POINT('Ctrl Pts',(13.9955563283149,-14.2617096427834,0.650217354190035));
#22556=CARTESIAN_POINT('Ctrl Pts',(13.8467023152938,-14.4688321611842,0.640851106713065));
#22557=CARTESIAN_POINT('Ctrl Pts',(13.6392165648734,-14.9240794292194,0.621215480666726));
#22558=CARTESIAN_POINT('Ctrl Pts',(13.5807974420006,-15.1670698897687,0.610734869027327));
#22559=CARTESIAN_POINT('Ctrl Pts',(13.5584324818228,-15.6716078298641,0.588973248445474));
#22560=CARTESIAN_POINT('Ctrl Pts',(13.598542278736,-15.9284928588798,0.577893339304166));
#22561=CARTESIAN_POINT('Ctrl Pts',(13.773173526214,-16.4008511610958,0.557519683857022));
#22562=CARTESIAN_POINT('Ctrl Pts',(13.9018579853462,-16.6132862458172,0.54872840560789));
#22563=CARTESIAN_POINT('Ctrl Pts',(14.2349802267053,-16.9816699616753,0.528340694405922));
#22564=CARTESIAN_POINT('Ctrl Pts',(14.4375333639109,-17.1330265345501,0.517510543306561));
#22565=CARTESIAN_POINT('Ctrl Pts',(14.8940137700958,-17.3523384610088,0.495729873520459));
#22566=CARTESIAN_POINT('Ctrl Pts',(15.1444779567369,-17.4162475185621,0.484995974086985));
#22567=CARTESIAN_POINT('Ctrl Pts',(15.644292945993,-17.4421185607808,0.465768343173262));
#22568=CARTESIAN_POINT('Ctrl Pts',(15.8886689106846,-17.4083000037079,0.456344488469386));
#22569=CARTESIAN_POINT('Ctrl Pts',(16.3602738338657,-17.2484328206968,0.435280848151098));
#22570=CARTESIAN_POINT('Ctrl Pts',(16.5819407282909,-17.1206457359146,0.424245033703684));
#22571=CARTESIAN_POINT('Ctrl Pts',(16.9645889726516,-16.7856687238997,0.402727812195782));
#22572=CARTESIAN_POINT('Ctrl Pts',(17.1213576046383,-16.5812682862177,0.393012028302294));
#22573=CARTESIAN_POINT('Ctrl Pts',(17.3428309783919,-16.130730045467,0.373579510995516));
#22574=CARTESIAN_POINT('Ctrl Pts',(17.4082697839647,-15.8902976976571,0.363209235317829));
#22575=CARTESIAN_POINT('Ctrl Pts',(17.4458200822696,-15.3881980765453,0.341552783779496));
#22576=CARTESIAN_POINT('Ctrl Pts',(17.4137884813012,-15.1310281688062,0.330460587311118));
#22577=CARTESIAN_POINT('Ctrl Pts',(17.2540504948445,-14.6530287775216,0.309843621638471));
#22578=CARTESIAN_POINT('Ctrl Pts',(17.1313390172738,-14.4356759590614,0.301024334102504));
#22579=CARTESIAN_POINT('Ctrl Pts',(16.8090342643691,-14.0571971876884,0.280822982049281));
#22580=CARTESIAN_POINT('Ctrl Pts',(16.6117620423532,-13.9002426534532,0.27006936510708));
#22581=CARTESIAN_POINT('Ctrl Pts',(16.1629040887197,-13.6672548471105,0.248278485924882));
#22582=CARTESIAN_POINT('Ctrl Pts',(15.9144966796287,-13.5956339334636,0.237455100705018));
#22583=CARTESIAN_POINT('Ctrl Pts',(15.6062624045507,-13.5701259723312,0.225391456362187));
#22584=CARTESIAN_POINT('Ctrl Pts',(15.5531033073173,-13.5679367061317,0.223358579476269));
#22585=CARTESIAN_POINT('Ctrl Pts',(15.5000000000001,-13.5679367061317,0.221374999999879));
#22586=CARTESIAN_POINT('Origin',(15.5,-15.5,11.20575));
#22587=CARTESIAN_POINT('',(15.5,-13.5679367061317,-0.278625000000132));
#22588=CARTESIAN_POINT('',(15.4999999999999,-13.5679367061317,0.190124999999821));
#22589=CARTESIAN_POINT('',(15.5,-13.5679367061317,11.20575));
#22590=CARTESIAN_POINT('Ctrl Pts',(15.4999999999999,-13.5679367061317,0.190124999999821));
#22591=CARTESIAN_POINT('Ctrl Pts',(15.7052232055908,-13.5679367061317,0.197790747375166));
#22592=CARTESIAN_POINT('Ctrl Pts',(15.9094431243975,-13.6006312438211,0.206124105599974));
#22593=CARTESIAN_POINT('Ctrl Pts',(16.3458500952319,-13.7445092392223,0.225528168010863));
#22594=CARTESIAN_POINT('Ctrl Pts',(16.5687690248994,-13.8706006648951,0.236574181605321));
#22595=CARTESIAN_POINT('Ctrl Pts',(16.9462938014503,-14.1957983248931,0.257689124656267));
#22596=CARTESIAN_POINT('Ctrl Pts',(17.0996068020759,-14.3891741439698,0.267213101031684));
#22597=CARTESIAN_POINT('Ctrl Pts',(17.3312210666002,-14.8328987043052,0.286351732158293));
#22598=CARTESIAN_POINT('Ctrl Pts',(17.403389189678,-15.0810963874238,0.297056940587811));
#22599=CARTESIAN_POINT('Ctrl Pts',(17.4463663432178,-15.5859112111088,0.318830503652366));
#22600=CARTESIAN_POINT('Ctrl Pts',(17.4188098289701,-15.8374917549286,0.329681620893121));
#22601=CARTESIAN_POINT('Ctrl Pts',(17.2705600347068,-16.3114416099335,0.350123922848632));
#22602=CARTESIAN_POINT('Ctrl Pts',(17.1530549287722,-16.5299161239957,0.358922469304659));
#22603=CARTESIAN_POINT('Ctrl Pts',(16.8349526369196,-16.9202726297615,0.379222999836066));
#22604=CARTESIAN_POINT('Ctrl Pts',(16.6338441663768,-17.085451210082,0.390297271892839));
#22605=CARTESIAN_POINT('Ctrl Pts',(16.1874197433205,-17.3225641667436,0.412086213416755));
#22606=CARTESIAN_POINT('Ctrl Pts',(15.9481982603318,-17.3956324394973,0.422597688314654));
#22607=CARTESIAN_POINT('Ctrl Pts',(15.4510757841914,-17.4478128352924,0.442292129851002));
#22608=CARTESIAN_POINT('Ctrl Pts',(15.1977325915627,-17.4248413113895,0.451571409240313));
#22609=CARTESIAN_POINT('Ctrl Pts',(14.7117348553567,-17.2822086107985,0.472800990486173));
#22610=CARTESIAN_POINT('Ctrl Pts',(14.4841033890512,-17.1630032804563,0.483874527712213));
#22611=CARTESIAN_POINT('Ctrl Pts',(14.0954494858794,-16.8491384993429,0.505160775836598));
#22612=CARTESIAN_POINT('Ctrl Pts',(13.935845283737,-16.6603046231705,0.515078993620139));
#22613=CARTESIAN_POINT('Ctrl Pts',(13.6903827463215,-16.223642546113,0.533913007255683));
#22614=CARTESIAN_POINT('Ctrl Pts',(13.6105539996563,-15.9778499407052,0.544514480397023));
#22615=CARTESIAN_POINT('Ctrl Pts',(13.5518158441316,-15.4739117712167,0.566250231803642));
#22616=CARTESIAN_POINT('Ctrl Pts',(13.571742794709,-15.2208352901084,0.577165871485818));
#22617=CARTESIAN_POINT('Ctrl Pts',(13.7057278794298,-14.742684868917,0.597789351347523));
#22618=CARTESIAN_POINT('Ctrl Pts',(13.8161488953126,-14.5214408844327,0.606664573343451));
#22619=CARTESIAN_POINT('Ctrl Pts',(14.1219606735895,-14.1213400688706,0.626716158351945));
#22620=CARTESIAN_POINT('Ctrl Pts',(14.318568611901,-13.9495491173579,0.637764922719238));
#22621=CARTESIAN_POINT('Ctrl Pts',(14.7590310485592,-13.6984440207756,0.659632917824901));
#22622=CARTESIAN_POINT('Ctrl Pts',(14.9966959458147,-13.6181551918391,0.670241966963359));
#22623=CARTESIAN_POINT('Ctrl Pts',(15.3284077888473,-13.5736457522818,0.683592357862532));
#22624=CARTESIAN_POINT('Ctrl Pts',(15.4142441778543,-13.5679367061317,0.686921743980895));
#22625=CARTESIAN_POINT('Ctrl Pts',(15.4999999999999,-13.5679367061317,0.690124999999829));
#22626=CARTESIAN_POINT('Ctrl Pts',(15.5000000000001,-13.5679367061317,0.221374999999879));
#22627=CARTESIAN_POINT('Ctrl Pts',(15.3093450221423,-13.5679367061317,0.214253422827828));
#22628=CARTESIAN_POINT('Ctrl Pts',(15.1194546083814,-13.5961535790767,0.206551882575901));
#22629=CARTESIAN_POINT('Ctrl Pts',(14.6948718232558,-13.7256105046371,0.187900494787472));
#22630=CARTESIAN_POINT('Ctrl Pts',(14.4700098904008,-13.8459724738417,0.176905464603589));
#22631=CARTESIAN_POINT('Ctrl Pts',(14.0753526090742,-14.1696924217256,0.155182435525569));
#22632=CARTESIAN_POINT('Ctrl Pts',(13.9107790537501,-14.3714265999853,0.145052382171085));
#22633=CARTESIAN_POINT('Ctrl Pts',(13.6758632413355,-14.8173319838793,0.125819688237564));
#22634=CARTESIAN_POINT('Ctrl Pts',(13.6037990124408,-15.0551292052584,0.115563070259359));
#22635=CARTESIAN_POINT('Ctrl Pts',(13.5518334963172,-15.5544792850638,0.0940252113380078));
#22636=CARTESIAN_POINT('Ctrl Pts',(13.5761558231528,-15.8116932971635,0.0829311125699534));
#22637=CARTESIAN_POINT('Ctrl Pts',(13.7215598037034,-16.2949297857371,0.0620882615572829));
#22638=CARTESIAN_POINT('Ctrl Pts',(13.8385708540846,-16.5170608745389,0.0531675695736204));
#22639=CARTESIAN_POINT('Ctrl Pts',(14.1505967901205,-16.9049967004005,0.0331462146120232));
#22640=CARTESIAN_POINT('Ctrl Pts',(14.3427581391604,-17.0670614604204,0.0224732986552362));
#22641=CARTESIAN_POINT('Ctrl Pts',(14.7840616507215,-17.3126898337665,0.000691997111495622));
#22642=CARTESIAN_POINT('Ctrl Pts',(15.0303088811274,-17.3915129002971,-0.0102060193255635));
#22643=CARTESIAN_POINT('Ctrl Pts',(15.5280187230135,-17.4473055261743,-0.0300003018240521));
#22644=CARTESIAN_POINT('Ctrl Pts',(15.7742335758728,-17.4281050083783,-0.0389538708149526));
#22645=CARTESIAN_POINT('Ctrl Pts',(16.2532901705975,-17.296907710707,-0.0596775634273534));
#22646=CARTESIAN_POINT('Ctrl Pts',(16.4808992967149,-17.1834947938276,-0.0706253476172892));
#22647=CARTESIAN_POINT('Ctrl Pts',(16.8829707781072,-16.8732369847255,-0.0923349979158201));
#22648=CARTESIAN_POINT('Ctrl Pts',(17.0524923783306,-16.6781753243463,-0.102808198428218));
#22649=CARTESIAN_POINT('Ctrl Pts',(17.3005030645304,-16.2425026235966,-0.121599538500263));
#22650=CARTESIAN_POINT('Ctrl Pts',(17.3801675176942,-16.0080032121443,-0.131713916058721));
#22651=CARTESIAN_POINT('Ctrl Pts',(17.4487724674381,-15.5123656486931,-0.153091647532988));
#22652=CARTESIAN_POINT('Ctrl Pts',(17.4333995515655,-15.2553808907698,-0.164175858159823));
#22653=CARTESIAN_POINT('Ctrl Pts',(17.3048200987405,-14.7662503100071,-0.185272931873504));
#22654=CARTESIAN_POINT('Ctrl Pts',(17.1944566843434,-14.5384527982996,-0.194401543720054));
#22655=CARTESIAN_POINT('Ctrl Pts',(16.894334784917,-14.139727275418,-0.214210934024622));
#22656=CARTESIAN_POINT('Ctrl Pts',(16.708188966555,-13.9720032635188,-0.224781197355577));
#22657=CARTESIAN_POINT('Ctrl Pts',(16.2741834170983,-13.7111048249335,-0.246619209086019));
#22658=CARTESIAN_POINT('Ctrl Pts',(16.0284985549801,-13.6237773096857,-0.257679625272395));
#22659=CARTESIAN_POINT('Ctrl Pts',(15.6823226738687,-13.574383016875,-0.271675640769364));
#22660=CARTESIAN_POINT('Ctrl Pts',(15.5911253193961,-13.5679367061317,-0.275221175973618));
#22661=CARTESIAN_POINT('Ctrl Pts',(15.5,-13.5679367061317,-0.278625000000132));
#22662=CARTESIAN_POINT('Origin',(15.5,-15.5,11.20575));
#22663=CARTESIAN_POINT('',(15.5,-13.5679367061317,-0.778625000000138));
#22664=CARTESIAN_POINT('',(15.5000000000213,-13.5679367061317,-0.30987499999859));
#22665=CARTESIAN_POINT('',(15.5,-13.5679367061317,11.20575));
#22666=CARTESIAN_POINT('Ctrl Pts',(15.5000000000426,-13.5679367061317,-0.30987499999859));
#22667=CARTESIAN_POINT('Ctrl Pts',(15.7451189900435,-13.5679367061371,-0.300719016644455));
#22668=CARTESIAN_POINT('Ctrl Pts',(15.9880788836297,-13.6145849104549,-0.290637672395874));
#22669=CARTESIAN_POINT('Ctrl Pts',(16.4525087353532,-13.7998506160078,-0.269294302322051));
#22670=CARTESIAN_POINT('Ctrl Pts',(16.6681650113368,-13.9401358945745,-0.258213469136004));
#22671=CARTESIAN_POINT('Ctrl Pts',(17.0300510391149,-14.293798813587,-0.237068805018263));
#22672=CARTESIAN_POINT('Ctrl Pts',(17.1737375672253,-14.5027181075033,-0.227889545454448));
#22673=CARTESIAN_POINT('Ctrl Pts',(17.3718881645073,-14.9610456268797,-0.208121062677908));
#22674=CARTESIAN_POINT('Ctrl Pts',(17.4255568606796,-15.2056351161721,-0.19757148207893));
#22675=CARTESIAN_POINT('Ctrl Pts',(17.437485526191,-15.7028273877144,-0.176126693273793));
#22676=CARTESIAN_POINT('Ctrl Pts',(17.3951930471992,-15.9508283805331,-0.16542996844748));
#22677=CARTESIAN_POINT('Ctrl Pts',(17.21903750586,-16.416216845007,-0.145356934524323));
#22678=CARTESIAN_POINT('Ctrl Pts',(17.087177913888,-16.6293413959128,-0.1364726175302));
#22679=CARTESIAN_POINT('Ctrl Pts',(16.7447233478944,-16.9997020048593,-0.115693680499745));
#22680=CARTESIAN_POINT('Ctrl Pts',(16.535223519972,-17.1512859841674,-0.104599143917209));
#22681=CARTESIAN_POINT('Ctrl Pts',(16.0781299074097,-17.3599329092899,-0.0830255691567002));
#22682=CARTESIAN_POINT('Ctrl Pts',(15.8364334516315,-17.4184418092008,-0.072735631907537));
#22683=CARTESIAN_POINT('Ctrl Pts',(15.3335771418074,-17.4419572678446,-0.0534451981390429));
#22684=CARTESIAN_POINT('Ctrl Pts',(15.0770448720173,-17.4026393126747,-0.0434417100341444));
#22685=CARTESIAN_POINT('Ctrl Pts',(14.5982616364445,-17.2273302215971,-0.0217769181315674));
#22686=CARTESIAN_POINT('Ctrl Pts',(14.3801849192581,-17.0946215718084,-0.0107690704262214));
#22687=CARTESIAN_POINT('Ctrl Pts',(14.0137016048736,-16.7583973031524,0.010171237110501));
#22688=CARTESIAN_POINT('Ctrl Pts',(13.8665662971669,-16.5604348396372,0.0193865553793814));
#22689=CARTESIAN_POINT('Ctrl Pts',(13.648896034541,-16.1097762694873,0.0388242627076073));
#22690=CARTESIAN_POINT('Ctrl Pts',(13.5844810246986,-15.8594139033154,0.0496228377752729));
#22691=CARTESIAN_POINT('Ctrl Pts',(13.5572975229277,-15.3542160204943,0.0714129228630833));
#22692=CARTESIAN_POINT('Ctrl Pts',(13.5924291711366,-15.1043600205154,0.0821896574543681));
#22693=CARTESIAN_POINT('Ctrl Pts',(13.7549549306398,-14.6347353821395,0.102445405107949));
#22694=CARTESIAN_POINT('Ctrl Pts',(13.8797188217565,-14.4190031858112,0.111248274994824));
#22695=CARTESIAN_POINT('Ctrl Pts',(14.2102312356738,-14.0387180251795,0.131795166002757));
#22696=CARTESIAN_POINT('Ctrl Pts',(14.4157066951986,-13.8803875205858,0.142884874300422));
#22697=CARTESIAN_POINT('Ctrl Pts',(14.8677637645239,-13.6576628179057,0.164573917775848));
#22698=CARTESIAN_POINT('Ctrl Pts',(15.1083498919245,-13.5919750720435,0.174977198896065));
#22699=CARTESIAN_POINT('Ctrl Pts',(15.4031822744539,-13.569754032749,0.186469354010822));
#22700=CARTESIAN_POINT('Ctrl Pts',(15.4516175612204,-13.5679367061317,0.188317760160551));
#22701=CARTESIAN_POINT('Ctrl Pts',(15.4999999999999,-13.5679367061317,0.190124999999821));
#22702=CARTESIAN_POINT('Ctrl Pts',(15.5,-13.5679367061317,-0.278625000000131));
#22703=CARTESIAN_POINT('Ctrl Pts',(15.3467892597189,-13.5679367061317,-0.284347914359666));
#22704=CARTESIAN_POINT('Ctrl Pts',(15.1938118281016,-13.5861582264254,-0.290455077212558));
#22705=CARTESIAN_POINT('Ctrl Pts',(14.8002115590521,-13.6816903721264,-0.30721755017852));
#22706=CARTESIAN_POINT('Ctrl Pts',(14.5700164472504,-13.7879612604545,-0.318107905048228));
#22707=CARTESIAN_POINT('Ctrl Pts',(14.1593674324255,-14.0854112710006,-0.339861742243558));
#22708=CARTESIAN_POINT('Ctrl Pts',(13.9839732656644,-14.2752366145712,-0.350507031688753));
#22709=CARTESIAN_POINT('Ctrl Pts',(13.7231840673424,-14.7026885542338,-0.369466729765817));
#22710=CARTESIAN_POINT('Ctrl Pts',(13.6365422675758,-14.9340075266013,-0.37921273586801));
#22711=CARTESIAN_POINT('Ctrl Pts',(13.5527035685452,-15.4259040924359,-0.400429111447581));
#22712=CARTESIAN_POINT('Ctrl Pts',(13.5598498556332,-15.6824101504194,-0.411492674857324));
#22713=CARTESIAN_POINT('Ctrl Pts',(13.6708737217057,-16.1685436044088,-0.432460477152238));
#22714=CARTESIAN_POINT('Ctrl Pts',(13.7700581636469,-16.3943923190575,-0.441627804171639));
#22715=CARTESIAN_POINT('Ctrl Pts',(14.0539091255659,-16.8066128735469,-0.46112045496409));
#22716=CARTESIAN_POINT('Ctrl Pts',(14.2395717537967,-16.9865111568954,-0.471935218600938));
#22717=CARTESIAN_POINT('Ctrl Pts',(14.6649766982385,-17.260117111467,-0.493726018953733));
#22718=CARTESIAN_POINT('Ctrl Pts',(14.8993253045762,-17.3532344934425,-0.50448785312903));
#22719=CARTESIAN_POINT('Ctrl Pts',(15.3879151897707,-17.4445879148856,-0.524708376132417));
#22720=CARTESIAN_POINT('Ctrl Pts',(15.6373703514434,-17.4429655287442,-0.533521108433316));
#22721=CARTESIAN_POINT('Ctrl Pts',(16.1314699144086,-17.3439130073667,-0.554113473589034));
#22722=CARTESIAN_POINT('Ctrl Pts',(16.3705992585577,-17.2437932713042,-0.565204895717519));
#22723=CARTESIAN_POINT('Ctrl Pts',(16.7876645305446,-16.9614315561499,-0.586873008236942));
#22724=CARTESIAN_POINT('Ctrl Pts',(16.9637580966902,-16.7850271274736,-0.597254988511056));
#22725=CARTESIAN_POINT('Ctrl Pts',(17.2443400454302,-16.3689556312255,-0.616708580128513));
#22726=CARTESIAN_POINT('Ctrl Pts',(17.3436265737928,-16.1315609718477,-0.626384649668764));
#22727=CARTESIAN_POINT('Ctrl Pts',(17.4440644805083,-15.6332086945697,-0.647879471588744));
#22728=CARTESIAN_POINT('Ctrl Pts',(17.4447534368414,-15.3772600500546,-0.658918992797644));
#22729=CARTESIAN_POINT('Ctrl Pts',(17.3489811389163,-14.8884838636653,-0.680000780850369));
#22730=CARTESIAN_POINT('Ctrl Pts',(17.2568181639608,-14.6596166093872,-0.689459136144938));
#22731=CARTESIAN_POINT('Ctrl Pts',(16.9858620067821,-14.238805099094,-0.708655396087524));
#22732=CARTESIAN_POINT('Ctrl Pts',(16.8058878841893,-14.0532686231487,-0.719379268374338));
#22733=CARTESIAN_POINT('Ctrl Pts',(16.3885881553997,-13.7662002686923,-0.741157641480895));
#22734=CARTESIAN_POINT('Ctrl Pts',(16.1564785085564,-13.665689225055,-0.751995294214013));
#22735=CARTESIAN_POINT('Ctrl Pts',(15.7761115117429,-13.5827427725166,-0.767992040173275));
#22736=CARTESIAN_POINT('Ctrl Pts',(15.6381065100508,-13.5679367061317,-0.773466277262654));
#22737=CARTESIAN_POINT('Ctrl Pts',(15.5,-13.5679367061317,-0.778625000000138));
#22738=CARTESIAN_POINT('Origin',(15.5,-15.5,11.20575));
#22739=CARTESIAN_POINT('',(15.4999999999999,-13.5679367061317,-1.27862500000015));
#22740=CARTESIAN_POINT('',(15.5,-13.5679367061317,-0.809875000000185));
#22741=CARTESIAN_POINT('',(15.5,-13.5679367061317,11.20575));
#22742=CARTESIAN_POINT('Ctrl Pts',(15.5000000000001,-13.5679367061317,-0.809875000000184));
#22743=CARTESIAN_POINT('Ctrl Pts',(15.5387848588903,-13.5679367061317,-0.808426260665929));
#22744=CARTESIAN_POINT('Ctrl Pts',(15.5776081217821,-13.569104553761,-0.806950901143725));
#22745=CARTESIAN_POINT('Ctrl Pts',(15.8627498107999,-13.5863172258654,-0.79592873452912));
#22746=CARTESIAN_POINT('Ctrl Pts',(16.1039441624047,-13.6482441649587,-0.785583839426259));
#22747=CARTESIAN_POINT('Ctrl Pts',(16.5586938389718,-13.8636040208236,-0.763953047887055));
#22748=CARTESIAN_POINT('Ctrl Pts',(16.7663048606795,-14.0184106751406,-0.752859564438582));
#22749=CARTESIAN_POINT('Ctrl Pts',(17.1030886658293,-14.3935142993235,-0.73219016123049));
#22750=CARTESIAN_POINT('Ctrl Pts',(17.2315636886463,-14.6078734364709,-0.723354008700342));
#22751=CARTESIAN_POINT('Ctrl Pts',(17.4012591024431,-15.0752831240919,-0.703193795820486));
#22752=CARTESIAN_POINT('Ctrl Pts',(17.4401670421017,-15.3241884796659,-0.692458064216697));
#22753=CARTESIAN_POINT('Ctrl Pts',(17.4209116308134,-15.8293918059367,-0.670667744343198));
#22754=CARTESIAN_POINT('Ctrl Pts',(17.3604173282467,-16.0807480284641,-0.659826302479591));
#22755=CARTESIAN_POINT('Ctrl Pts',(17.1497816929781,-16.5348352725858,-0.640240710332106));
#22756=CARTESIAN_POINT('Ctrl Pts',(17.0057085011959,-16.7351193667879,-0.631148276498292));
#22757=CARTESIAN_POINT('Ctrl Pts',(16.6447314320371,-17.0767669839641,-0.610296685602457));
#22758=CARTESIAN_POINT('Ctrl Pts',(16.4291281586241,-17.2126942752496,-0.599311816112351));
#22759=CARTESIAN_POINT('Ctrl Pts',(15.9522914740593,-17.396071415368,-0.577545739488896));
#22760=CARTESIAN_POINT('Ctrl Pts',(15.6949512567242,-17.4394863853226,-0.567317142600485));
#22761=CARTESIAN_POINT('Ctrl Pts',(15.1907605692904,-17.4229690903241,-0.548127787168027));
#22762=CARTESIAN_POINT('Ctrl Pts',(14.9485965706545,-17.3679857370151,-0.53789641724223));
#22763=CARTESIAN_POINT('Ctrl Pts',(14.4891878782661,-17.166282104194,-0.516386105083495));
#22764=CARTESIAN_POINT('Ctrl Pts',(14.2777915836231,-17.0180420352629,-0.505292843771063));
#22765=CARTESIAN_POINT('Ctrl Pts',(13.9295152530061,-16.6526099917286,-0.484402733995875));
#22766=CARTESIAN_POINT('Ctrl Pts',(13.7941507738708,-16.4407479085025,-0.475451133965662));
#22767=CARTESIAN_POINT('Ctrl Pts',(13.611383887522,-15.9774528011728,-0.455468390267086));
#22768=CARTESIAN_POINT('Ctrl Pts',(13.5656468617909,-15.7304237057034,-0.444813585105621));
#22769=CARTESIAN_POINT('Ctrl Pts',(13.5704710073905,-15.2255315160606,-0.423036685109424));
#22770=CARTESIAN_POINT('Ctrl Pts',(13.623779229161,-14.9725259783178,-0.412124105341039));
#22771=CARTESIAN_POINT('Ctrl Pts',(13.8215336428728,-14.5122846645607,-0.392273077201934));
#22772=CARTESIAN_POINT('Ctrl Pts',(13.9600852553974,-14.3077326406346,-0.383350131532038));
#22773=CARTESIAN_POINT('Ctrl Pts',(14.311092329695,-13.9563854884097,-0.362661772922335));
#22774=CARTESIAN_POINT('Ctrl Pts',(14.5221235135244,-13.814770334655,-0.351725021873647));
#22775=CARTESIAN_POINT('Ctrl Pts',(14.9904064163151,-13.6188695990394,-0.330008374038312));
#22776=CARTESIAN_POINT('Ctrl Pts',(15.2437584839143,-13.5679791180275,-0.319447360158956));
#22777=CARTESIAN_POINT('Ctrl Pts',(15.4997866765027,-13.5679367149642,-0.309882968509973));
#22778=CARTESIAN_POINT('Ctrl Pts',(15.4998933384699,-13.5679367061317,-0.309878984151688));
#22779=CARTESIAN_POINT('Ctrl Pts',(15.5000000000426,-13.5679367061317,-0.30987499999859));
#22780=CARTESIAN_POINT('Ctrl Pts',(15.5,-13.5679367061317,-0.778625000000138));
#22781=CARTESIAN_POINT('Ctrl Pts',(15.3931460600035,-13.5679367061317,-0.782616338639041));
#22782=CARTESIAN_POINT('Ctrl Pts',(15.2862458066186,-13.5768002208548,-0.786800556825666));
#22783=CARTESIAN_POINT('Ctrl Pts',(14.9264097349309,-13.6371564581267,-0.801543228515925));
#22784=CARTESIAN_POINT('Ctrl Pts',(14.6835020776055,-13.7301105172148,-0.812621248594988));
#22785=CARTESIAN_POINT('Ctrl Pts',(14.2567488546817,-14.0004851883713,-0.834392725983059));
#22786=CARTESIAN_POINT('Ctrl Pts',(14.0749328111488,-14.1720617647974,-0.844884342273106));
#22787=CARTESIAN_POINT('Ctrl Pts',(13.7832732837112,-14.5783544242248,-0.864540827785101));
#22788=CARTESIAN_POINT('Ctrl Pts',(13.6776776440773,-14.8102645186437,-0.873875479390643));
#22789=CARTESIAN_POINT('Ctrl Pts',(13.5612057991943,-15.3034623332341,-0.895147980148236));
#22790=CARTESIAN_POINT('Ctrl Pts',(13.552197396611,-15.5600993604861,-0.906217192531462));
#22791=CARTESIAN_POINT('Ctrl Pts',(13.6325934592672,-16.0528776431264,-0.927471598128334));
#22792=CARTESIAN_POINT('Ctrl Pts',(13.7176559736562,-16.2849105083636,-0.937309340873369));
#22793=CARTESIAN_POINT('Ctrl Pts',(13.9755352339037,-16.7142424065984,-0.956200886377741));
#22794=CARTESIAN_POINT('Ctrl Pts',(14.1496041202698,-16.9052695292978,-0.966822589771756));
#22795=CARTESIAN_POINT('Ctrl Pts',(14.5583089435885,-17.2056519897364,-0.988567046050803));
#22796=CARTESIAN_POINT('Ctrl Pts',(14.7879324229243,-17.3135593941174,-0.999471341534755));
#22797=CARTESIAN_POINT('Ctrl Pts',(15.2696786466829,-17.4338950578203,-1.02006125963416));
#22798=CARTESIAN_POINT('Ctrl Pts',(15.5166980413127,-17.4474891140478,-1.02891605403808));
#22799=CARTESIAN_POINT('Ctrl Pts',(16.0156874195765,-17.3798092848061,-1.04901448947301));
#22800=CARTESIAN_POINT('Ctrl Pts',(16.2621352115938,-17.2940873362134,-1.06006877807144));
#22801=CARTESIAN_POINT('Ctrl Pts',(16.698154944133,-17.0359029315518,-1.08192349546387));
#22802=CARTESIAN_POINT('Ctrl Pts',(16.8855107789499,-16.8692878721634,-1.09251504125555));
#22803=CARTESIAN_POINT('Ctrl Pts',(17.1880123646469,-16.472705598965,-1.11236709941354));
#22804=CARTESIAN_POINT('Ctrl Pts',(17.2997096590055,-16.2460520791468,-1.12144644415624));
#22805=CARTESIAN_POINT('Ctrl Pts',(17.431671791372,-15.7580841556283,-1.1424933703908));
#22806=CARTESIAN_POINT('Ctrl Pts',(17.4488346169962,-15.5010293356259,-1.15358060291997));
#22807=CARTESIAN_POINT('Ctrl Pts',(17.383549418459,-15.0046042925852,-1.17499229979244));
#22808=CARTESIAN_POINT('Ctrl Pts',(17.3053971666591,-14.7694246899964,-1.18513601520691));
#22809=CARTESIAN_POINT('Ctrl Pts',(17.0601513563756,-14.3319804120671,-1.20400376656016));
#22810=CARTESIAN_POINT('Ctrl Pts',(16.8918928500653,-14.1358043641068,-1.21438674923054));
#22811=CARTESIAN_POINT('Ctrl Pts',(16.491712694381,-13.8228284522729,-1.23608437073301));
#22812=CARTESIAN_POINT('Ctrl Pts',(16.264686804895,-13.7078902729296,-1.24704326280146));
#22813=CARTESIAN_POINT('Ctrl Pts',(15.8517814524953,-13.5920235017939,-1.26496537709516));
#22814=CARTESIAN_POINT('Ctrl Pts',(15.676151507024,-13.5679367061317,-1.27204517415274));
#22815=CARTESIAN_POINT('Ctrl Pts',(15.4999999999999,-13.5679367061317,-1.27862500000015));
#22816=CARTESIAN_POINT('Origin',(15.5,-15.5,11.20575));
#22817=CARTESIAN_POINT('',(15.5,-13.5679367061317,-1.77862500000015));
#22818=CARTESIAN_POINT('',(15.5,-13.5679367061317,-1.30987500000019));
#22819=CARTESIAN_POINT('',(15.5,-13.5679367061317,11.20575));
#22820=CARTESIAN_POINT('',(16.6356236642092,-13.9369173237082,-2.22824839960634));
#22821=CARTESIAN_POINT('Ctrl Pts',(15.5,-13.5679367061317,-1.77862500000015));
#22822=CARTESIAN_POINT('Ctrl Pts',(15.4713110103049,-13.5679367061317,-1.77969662611974));
#22823=CARTESIAN_POINT('Ctrl Pts',(15.4425999921594,-13.5685756992767,-1.78078285552937));
#22824=CARTESIAN_POINT('Ctrl Pts',(15.1581590399474,-13.5812658327421,-1.79168131479254));
#22825=CARTESIAN_POINT('Ctrl Pts',(14.9072543398391,-13.6433835357265,-1.80239303666449));
#22826=CARTESIAN_POINT('Ctrl Pts',(14.4490712181685,-13.8594981524984,-1.82416835552268));
#22827=CARTESIAN_POINT('Ctrl Pts',(14.2453192502126,-14.0095359244182,-1.83501484569199));
#22828=CARTESIAN_POINT('Ctrl Pts',(13.9097095424868,-14.3755767710421,-1.85544494570745));
#22829=CARTESIAN_POINT('Ctrl Pts',(13.779653496445,-14.5868970845778,-1.86424124385709));
#22830=CARTESIAN_POINT('Ctrl Pts',(13.601624809573,-15.0579406863098,-1.88455819392919));
#22831=CARTESIAN_POINT('Ctrl Pts',(13.5596639923122,-15.314726118177,-1.89563380726797));
#22832=CARTESIAN_POINT('Ctrl Pts',(13.5785378997819,-15.8197591251871,-1.9174167809682));
#22833=CARTESIAN_POINT('Ctrl Pts',(13.635337470358,-16.063306547793,-1.92792141537377));
#22834=CARTESIAN_POINT('Ctrl Pts',(13.8396294894159,-16.5196132324098,-1.94760273594545));
#22835=CARTESIAN_POINT('Ctrl Pts',(13.98670541897,-16.7273518608751,-1.95690084581238));
#22836=CARTESIAN_POINT('Ctrl Pts',(14.3540458828622,-17.0761951408069,-1.97814531086595));
#22837=CARTESIAN_POINT('Ctrl Pts',(14.5713394118551,-17.213239044857,-1.9892173975925));
#22838=CARTESIAN_POINT('Ctrl Pts',(15.0377637904636,-17.3918917772351,-2.01049265500658));
#22839=CARTESIAN_POINT('Ctrl Pts',(15.2811490461273,-17.4351931175239,-2.02038271492023));
#22840=CARTESIAN_POINT('Ctrl Pts',(15.7819930616688,-17.4284331863443,-2.03923663513813));
#22841=CARTESIAN_POINT('Ctrl Pts',(16.0346645547899,-17.3741617366328,-2.04984514097278));
#22842=CARTESIAN_POINT('Ctrl Pts',(16.500008982865,-17.1721421784805,-2.0715839851788));
#22843=CARTESIAN_POINT('Ctrl Pts',(16.7088902825659,-17.0279622254971,-2.08249574331544));
#22844=CARTESIAN_POINT('Ctrl Pts',(17.055293507135,-16.6721862680338,-2.10310764444889));
#22845=CARTESIAN_POINT('Ctrl Pts',(17.191302469575,-16.4656337932766,-2.11197549347074));
#22846=CARTESIAN_POINT('Ctrl Pts',(17.383958897045,-16.0003669873985,-2.13204328004182));
#22847=CARTESIAN_POINT('Ctrl Pts',(17.4339176130592,-15.7441588929761,-2.14309399178763));
#22848=CARTESIAN_POINT('Ctrl Pts',(17.4301770605656,-15.2372592429962,-2.16495747712602));
#22849=CARTESIAN_POINT('Ctrl Pts',(17.3804225882662,-14.9914303047801,-2.17556051736614));
#22850=CARTESIAN_POINT('Ctrl Pts',(17.2188593063871,-14.6006806202927,-2.19241424768163));
#22851=CARTESIAN_POINT('Ctrl Pts',(17.1307744677382,-14.4493679380718,-2.19870147391129));
#22852=CARTESIAN_POINT('Ctrl Pts',(16.9124347549226,-14.1693732822038,-2.21289549932321));
#22853=CARTESIAN_POINT('Ctrl Pts',(16.78183780444,-14.0431460180095,-2.22049591927456));
#22854=CARTESIAN_POINT('Ctrl Pts',(16.6356236661869,-13.9369173213456,-2.22824840453312));
#22855=CARTESIAN_POINT('',(16.6356257705294,-13.936918850212,-1.75949829183042));
#22856=CARTESIAN_POINT('',(16.6356252385745,-13.9369184637308,-1.75949832116282));
#22857=CARTESIAN_POINT('Ctrl Pts',(16.6356257705685,-13.9369188502404,-1.75949829295571));
#22858=CARTESIAN_POINT('Ctrl Pts',(16.8232265616208,-14.0732165037121,-1.74955141913566));
#22859=CARTESIAN_POINT('Ctrl Pts',(16.9847823163708,-14.2421926306508,-1.73987267086339));
#22860=CARTESIAN_POINT('Ctrl Pts',(17.2378815903649,-14.625688547538,-1.72214816701709));
#22861=CARTESIAN_POINT('Ctrl Pts',(17.3287014043758,-14.8362794639401,-1.71350244965325));
#22862=CARTESIAN_POINT('Ctrl Pts',(17.4385845729922,-15.3036899854237,-1.69334220080742));
#22863=CARTESIAN_POINT('Ctrl Pts',(17.447619886958,-15.5584934383095,-1.68235207375453));
#22864=CARTESIAN_POINT('Ctrl Pts',(17.366264820819,-16.0626255591014,-1.66060795688252));
#22865=CARTESIAN_POINT('Ctrl Pts',(17.2745029457006,-16.306592918934,-1.65043016901723));
#22866=CARTESIAN_POINT('Ctrl Pts',(17.0069230177962,-16.7339605492266,-1.63121863353648));
#22867=CARTESIAN_POINT('Ctrl Pts',(16.8376064327547,-16.9157196559878,-1.62097431691815));
#22868=CARTESIAN_POINT('Ctrl Pts',(16.4321558772125,-17.2115388605548,-1.59944982869592));
#22869=CARTESIAN_POINT('Ctrl Pts',(16.1976492003963,-17.3197729456469,-1.58835608490563));
#22870=CARTESIAN_POINT('Ctrl Pts',(15.7067373188974,-17.4370349875308,-1.56749008537744));
#22871=CARTESIAN_POINT('Ctrl Pts',(15.4557223788825,-17.44753196976,-1.55855468409501));
#22872=CARTESIAN_POINT('Ctrl Pts',(14.9634366275308,-17.3726902789252,-1.53855219877784));
#22873=CARTESIAN_POINT('Ctrl Pts',(14.726821985697,-17.2880297167385,-1.52788809973695));
#22874=CARTESIAN_POINT('Ctrl Pts',(14.2927306055592,-17.0300046441306,-1.50610884865212));
#22875=CARTESIAN_POINT('Ctrl Pts',(14.1008202908092,-16.8567343671546,-1.49520365267535));
#22876=CARTESIAN_POINT('Ctrl Pts',(13.8024087055843,-16.454457921933,-1.47538156930739));
#22877=CARTESIAN_POINT('Ctrl Pts',(13.6952482164322,-16.2319055093249,-1.46644338907454));
#22878=CARTESIAN_POINT('Ctrl Pts',(13.5679372308721,-15.7518323297933,-1.44573697721874));
#22879=CARTESIAN_POINT('Ctrl Pts',(13.5515962723608,-15.4981347275301,-1.43479454747415));
#22880=CARTESIAN_POINT('Ctrl Pts',(13.6177050294595,-14.9946779887315,-1.41307956103122));
#22881=CARTESIAN_POINT('Ctrl Pts',(13.7011232772003,-14.7500889892398,-1.4025630039161));
#22882=CARTESIAN_POINT('Ctrl Pts',(13.9530518157521,-14.3167686917903,-1.38380772364012));
#22883=CARTESIAN_POINT('Ctrl Pts',(14.1156697545305,-14.1300765218334,-1.37370723711989));
#22884=CARTESIAN_POINT('Ctrl Pts',(14.5094994028657,-13.8216873535972,-1.35234574472332));
#22885=CARTESIAN_POINT('Ctrl Pts',(14.7392900935943,-13.7058009544623,-1.34126312922332));
#22886=CARTESIAN_POINT('Ctrl Pts',(15.1530393767014,-13.5913602763721,-1.32334024636833));
#22887=CARTESIAN_POINT('Ctrl Pts',(15.3262907155804,-13.5679367061317,-1.31636360097141));
#22888=CARTESIAN_POINT('Ctrl Pts',(15.5000000000001,-13.5679367061317,-1.30987500000019));
#22889=CARTESIAN_POINT('Origin',(-15.5,-15.5000000000001,11.20575));
#22890=CARTESIAN_POINT('',(-13.5679367061318,-15.5000000000001,1.22137499999992));
#22891=CARTESIAN_POINT('',(-13.5679367061318,-15.5000000000001,1.38580000000001));
#22892=CARTESIAN_POINT('',(-13.5679367061318,-15.5000000000001,11.20575));
#22893=CARTESIAN_POINT('',(-16.4140591443297,-17.2021646372136,1.3857999999999));
#22894=CARTESIAN_POINT('Origin',(-15.5,-15.5000000000001,1.3858));
#22895=CARTESIAN_POINT('Ctrl Pts',(-16.4140591443298,-17.2021646372136,
1.38579999999988));
#22896=CARTESIAN_POINT('Ctrl Pts',(-16.2625891374719,-17.2835037402787,
1.37926682864284));
#22897=CARTESIAN_POINT('Ctrl Pts',(-16.1009499216563,-17.3442553078355,
1.37229504117912));
#22898=CARTESIAN_POINT('Ctrl Pts',(-15.7606791262596,-17.4225866712077,
1.35761855531741));
#22899=CARTESIAN_POINT('Ctrl Pts',(-15.5832774889169,-17.4383898562165,
1.34996690652036));
#22900=CARTESIAN_POINT('Ctrl Pts',(-15.1505459516663,-17.4173618064992,
1.33130242407199));
#22901=CARTESIAN_POINT('Ctrl Pts',(-14.8998465928292,-17.3542469088622,
1.32048931391007));
#22902=CARTESIAN_POINT('Ctrl Pts',(-14.4480453995349,-17.138910231798,1.30100232320917));
#22903=CARTESIAN_POINT('Ctrl Pts',(-14.2493134353814,-16.9927945766542,
1.29183017935079));
#22904=CARTESIAN_POINT('Ctrl Pts',(-13.9112799545244,-16.6281426358706,
1.27091926224018));
#22905=CARTESIAN_POINT('Ctrl Pts',(-13.7774947327411,-16.4108843720761,
1.25991876916933));
#22906=CARTESIAN_POINT('Ctrl Pts',(-13.608962253005,-15.9581594812378,1.23937348399107));
#22907=CARTESIAN_POINT('Ctrl Pts',(-13.5679367061318,-15.7298816358067,
1.22996181912328));
#22908=CARTESIAN_POINT('Ctrl Pts',(-13.5679367061318,-15.5000000000001,
1.22137499999992));
#22909=CARTESIAN_POINT('Origin',(-15.5,-15.5000000000001,11.20575));
#22910=CARTESIAN_POINT('',(-13.5679367061318,-15.5000000000001,0.721374999999908));
#22911=CARTESIAN_POINT('',(-13.5679367061318,-15.5000000000001,1.19012499999982));
#22912=CARTESIAN_POINT('',(-13.5679367061318,-15.5000000000001,11.20575));
#22913=CARTESIAN_POINT('',(-17.0070594673502,-16.7089831815964,1.3858));
#22914=CARTESIAN_POINT('Ctrl Pts',(-13.5679367061318,-15.5000000000001,
1.19012499999982));
#22915=CARTESIAN_POINT('Ctrl Pts',(-13.5679367061318,-15.6209597157623,
1.19464323477233));
#22916=CARTESIAN_POINT('Ctrl Pts',(-13.5792946957064,-15.7419184750203,
1.19940637898297));
#22917=CARTESIAN_POINT('Ctrl Pts',(-13.650067406739,-16.1137167329617,1.21482051737718));
#22918=CARTESIAN_POINT('Ctrl Pts',(-13.7479960405404,-16.3540308512713,
1.22590894156169));
#22919=CARTESIAN_POINT('Ctrl Pts',(-14.0267023405018,-16.7741136008829,
1.24761093429803));
#22920=CARTESIAN_POINT('Ctrl Pts',(-14.201640121497,-16.9519823816315,1.25802759498804));
#22921=CARTESIAN_POINT('Ctrl Pts',(-14.6147032779422,-17.2359894885839,
1.2775442497622));
#22922=CARTESIAN_POINT('Ctrl Pts',(-14.8503902891224,-17.3372359040124,
1.28710617538626));
#22923=CARTESIAN_POINT('Ctrl Pts',(-15.3471703745481,-17.4426537117391,
1.30853318586959));
#22924=CARTESIAN_POINT('Ctrl Pts',(-15.6033601229594,-17.4459126157984,
1.31958310631925));
#22925=CARTESIAN_POINT('Ctrl Pts',(-16.0780162130539,-17.3577451237209,
1.34005586945288));
#22926=CARTESIAN_POINT('Ctrl Pts',(-16.2939169603254,-17.2762244544319,
1.3492321587465));
#22927=CARTESIAN_POINT('Ctrl Pts',(-16.6881081787936,-17.0408604404304,
1.36652484724902));
#22928=CARTESIAN_POINT('Ctrl Pts',(-16.8630519069466,-16.8884959825849,
1.37598896763183));
#22929=CARTESIAN_POINT('Ctrl Pts',(-17.0070594673503,-16.7089831815965,
1.38580000000001));
#22930=CARTESIAN_POINT('Origin',(-15.5,-15.5000000000001,1.3858));
#22931=CARTESIAN_POINT('Ctrl Pts',(-13.5679367061318,-15.5000000000001,
1.22137499999992));
#22932=CARTESIAN_POINT('Ctrl Pts',(-13.5679367061318,-15.4729341635697,
1.22036400387996));
#22933=CARTESIAN_POINT('Ctrl Pts',(-13.5685054395976,-15.4458469974684,
1.21933994578423));
#22934=CARTESIAN_POINT('Ctrl Pts',(-13.5800041738663,-15.1726369382998,
1.20888669011567));
#22935=CARTESIAN_POINT('Ctrl Pts',(-13.6373364197397,-14.9307787640132,
1.1986160877525));
#22936=CARTESIAN_POINT('Ctrl Pts',(-13.8436681825557,-14.4729009295844,
1.177063148319));
#22937=CARTESIAN_POINT('Ctrl Pts',(-13.9941383694055,-14.2627623228301,
1.16596877121766));
#22938=CARTESIAN_POINT('Ctrl Pts',(-14.3628583039267,-13.9183617243244,
1.14515252621433));
#22939=CARTESIAN_POINT('Ctrl Pts',(-14.5755603827482,-13.7853340429807,
1.13624772829804));
#22940=CARTESIAN_POINT('Ctrl Pts',(-15.0402511773768,-13.6069662799091,
1.11620478611874));
#22941=CARTESIAN_POINT('Ctrl Pts',(-15.2879321569902,-13.5635189852138,
1.10552186403231));
#22942=CARTESIAN_POINT('Ctrl Pts',(-15.7929752643667,-13.5731954042506,
1.08373845468527));
#22943=CARTESIAN_POINT('Ctrl Pts',(-16.0454493147401,-13.6289269314741,
1.07284879891439));
#22944=CARTESIAN_POINT('Ctrl Pts',(-16.5036338509587,-13.831024509948,1.05308648325627));
#22945=CARTESIAN_POINT('Ctrl Pts',(-16.7067442551307,-13.9714260900016,
1.0441143076934));
#22946=CARTESIAN_POINT('Ctrl Pts',(-17.0548537166298,-14.3257784407275,
1.02337081592583));
#22947=CARTESIAN_POINT('Ctrl Pts',(-17.1945806685306,-14.5383567471224,
1.01241699562448));
#22948=CARTESIAN_POINT('Ctrl Pts',(-17.3860429607487,-15.0088443364473,
0.99071371463696));
#22949=CARTESIAN_POINT('Ctrl Pts',(-17.4344332047526,-15.2627143707624,
0.980289491352765));
#22950=CARTESIAN_POINT('Ctrl Pts',(-17.4296140643915,-15.7641076910023,
0.961456907719596));
#22951=CARTESIAN_POINT('Ctrl Pts',(-17.3804673297517,-16.0069337844365,
0.951326678304535));
#22952=CARTESIAN_POINT('Ctrl Pts',(-17.1903012302114,-16.4699471303935,
0.929930537917788));
#22953=CARTESIAN_POINT('Ctrl Pts',(-17.0476412720934,-16.6843681047608,
0.918844635143063));
#22954=CARTESIAN_POINT('Ctrl Pts',(-16.6904570707359,-17.0422253710005,
0.897774518646293));
#22955=CARTESIAN_POINT('Ctrl Pts',(-16.4806668477673,-17.1834288056111,
0.888672908962502));
#22956=CARTESIAN_POINT('Ctrl Pts',(-16.0208578479742,-17.377035015047,0.868840527295173));
#22957=CARTESIAN_POINT('Ctrl Pts',(-15.7755220878932,-17.4283735116763,
0.858258758707007));
#22958=CARTESIAN_POINT('Ctrl Pts',(-15.2690019280109,-17.4355092605755,
0.836411641452892));
#22959=CARTESIAN_POINT('Ctrl Pts',(-15.0126438261503,-17.3873412234668,
0.82535445961893));
#22960=CARTESIAN_POINT('Ctrl Pts',(-14.5460700123029,-17.1979533837254,
0.805230299464693));
#22961=CARTESIAN_POINT('Ctrl Pts',(-14.3384565929788,-17.0632817898192,
0.796385555304599));
#22962=CARTESIAN_POINT('Ctrl Pts',(-13.9803614870582,-16.7193021670802,
0.775814168998308));
#22963=CARTESIAN_POINT('Ctrl Pts',(-13.8348471763986,-16.5115619835562,
0.764916258611936));
#22964=CARTESIAN_POINT('Ctrl Pts',(-13.6296318244408,-16.0477927710948,
0.743167333638657));
#22965=CARTESIAN_POINT('Ctrl Pts',(-13.5735885358348,-15.7954972626707,
0.732534660758096));
#22966=CARTESIAN_POINT('Ctrl Pts',(-13.5680718804938,-15.526395610973,0.722363876197133));
#22967=CARTESIAN_POINT('Ctrl Pts',(-13.5679367061318,-15.5131950983567,
0.721867879400674));
#22968=CARTESIAN_POINT('Ctrl Pts',(-13.5679367061318,-15.5000000000001,
0.72137499999991));
#22969=CARTESIAN_POINT('Origin',(-15.5,-15.5000000000001,11.20575));
#22970=CARTESIAN_POINT('',(-13.5679367061318,-15.5000000000002,0.221374999999906));
#22971=CARTESIAN_POINT('',(-13.5679367061318,-15.5000000000001,0.690124999999812));
#22972=CARTESIAN_POINT('',(-13.5679367061318,-15.5000000000001,11.20575));
#22973=CARTESIAN_POINT('Ctrl Pts',(-13.5679367061318,-15.5,0.690124999999811));
#22974=CARTESIAN_POINT('Ctrl Pts',(-13.5679367061318,-15.6631976348033,
0.696220957019171));
#22975=CARTESIAN_POINT('Ctrl Pts',(-13.5886111528804,-15.8260698424813,
0.702750621155628));
#22976=CARTESIAN_POINT('Ctrl Pts',(-13.6937750358448,-16.231840773596,0.720175424526339));
#22977=CARTESIAN_POINT('Ctrl Pts',(-13.8061679673988,-16.4638288993586,
0.731264781557226));
#22978=CARTESIAN_POINT('Ctrl Pts',(-14.1088337976827,-16.8630470507194,
0.75270412300504));
#22979=CARTESIAN_POINT('Ctrl Pts',(-14.2932884830906,-17.0287614441965,
0.762872018728063));
#22980=CARTESIAN_POINT('Ctrl Pts',(-14.723125143869,-17.287405358774,0.781803012187269));
#22981=CARTESIAN_POINT('Ctrl Pts',(-14.9664736216109,-17.3745003706307,
0.79211305640894));
#22982=CARTESIAN_POINT('Ctrl Pts',(-15.4692792372012,-17.4482099203794,
0.813799958747424));
#22983=CARTESIAN_POINT('Ctrl Pts',(-15.7235658751718,-17.4355847239786,
0.824767794651914));
#22984=CARTESIAN_POINT('Ctrl Pts',(-16.2055976541623,-17.315173374422,0.845558684393136));
#22985=CARTESIAN_POINT('Ctrl Pts',(-16.4295122772784,-17.211349687416,0.854579673980957));
#22986=CARTESIAN_POINT('Ctrl Pts',(-16.835971896653,-16.9190154733783,0.874264961849451));
#22987=CARTESIAN_POINT('Ctrl Pts',(-17.0120418978356,-16.7296891979227,
0.885134014187586));
#22988=CARTESIAN_POINT('Ctrl Pts',(-17.2766178136157,-16.2991617620676,
0.906921415251255));
#22989=CARTESIAN_POINT('Ctrl Pts',(-17.3648212635819,-16.0634585876007,
0.917627873583991));
#22990=CARTESIAN_POINT('Ctrl Pts',(-17.4465792698413,-15.5727030691466,
0.937722356281882));
#22991=CARTESIAN_POINT('Ctrl Pts',(-17.4398199793546,-15.3223565583369,
0.946593274573956));
#22992=CARTESIAN_POINT('Ctrl Pts',(-17.3302144103325,-14.8300711076976,
0.96734546267104));
#22993=CARTESIAN_POINT('Ctrl Pts',(-17.2253688342262,-14.5935881752461,
0.978439949755289));
#22994=CARTESIAN_POINT('Ctrl Pts',(-16.9351538432135,-14.183201533444,1.00002795682994));
#22995=CARTESIAN_POINT('Ctrl Pts',(-16.7556158303762,-14.0110153602741,
1.01033156193276));
#22996=CARTESIAN_POINT('Ctrl Pts',(-16.3329965553288,-13.7379425524705,
1.02964587164789));
#22997=CARTESIAN_POINT('Ctrl Pts',(-16.0918227958039,-13.6429845085469,
1.03959862802553));
#22998=CARTESIAN_POINT('Ctrl Pts',(-15.5900949475545,-13.553533331627,1.06123904433771));
#22999=CARTESIAN_POINT('Ctrl Pts',(-15.3347633934771,-13.5584675814189,
1.0722519493362));
#23000=CARTESIAN_POINT('Ctrl Pts',(-14.8487842127037,-13.6646353766638,
1.09321309755167));
#23001=CARTESIAN_POINT('Ctrl Pts',(-14.6220240391682,-13.7616722786086,
1.10246053097514));
#23002=CARTESIAN_POINT('Ctrl Pts',(-14.2071591450865,-14.0415852702359,
1.12186311344));
#23003=CARTESIAN_POINT('Ctrl Pts',(-14.0255156909762,-14.2255255819053,
1.13265117917154));
#23004=CARTESIAN_POINT('Ctrl Pts',(-13.7477641930796,-14.6484954207351,
1.1544404228268));
#23005=CARTESIAN_POINT('Ctrl Pts',(-13.6523788496883,-14.8821830754006,
1.16522647893844));
#23006=CARTESIAN_POINT('Ctrl Pts',(-13.5800170676888,-15.2505243179923,
1.18054575641213));
#23007=CARTESIAN_POINT('Ctrl Pts',(-13.5679367061318,-15.3752528162567,
1.18546529110573));
#23008=CARTESIAN_POINT('Ctrl Pts',(-13.5679367061318,-15.5000000000001,
1.19012499999982));
#23009=CARTESIAN_POINT('Ctrl Pts',(-13.5679367061318,-15.5000000000001,
0.721374999999909));
#23010=CARTESIAN_POINT('Ctrl Pts',(-13.5679367061318,-15.2685828061803,
0.712730822841552));
#23011=CARTESIAN_POINT('Ctrl Pts',(-13.6095133453597,-15.0388969704722,
0.703254680206819));
#23012=CARTESIAN_POINT('Ctrl Pts',(-13.7800568346783,-14.5838672571245,
0.682579933274515));
#23013=CARTESIAN_POINT('Ctrl Pts',(-13.9154007891409,-14.3657373184651,
0.671513264882122));
#23014=CARTESIAN_POINT('Ctrl Pts',(-14.2617096431742,-13.9955563279968,
0.65021735416984));
#23015=CARTESIAN_POINT('Ctrl Pts',(-14.468832161597,-13.8467023150394,0.64085110669535));
#23016=CARTESIAN_POINT('Ctrl Pts',(-14.9240794296703,-13.6392165647333,
0.621215480647348));
#23017=CARTESIAN_POINT('Ctrl Pts',(-15.1670698902397,-13.5807974419184,
0.610734869007077));
#23018=CARTESIAN_POINT('Ctrl Pts',(-15.6716078303532,-13.5584324818654,
0.588973248424435));
#23019=CARTESIAN_POINT('Ctrl Pts',(-15.9284928593656,-13.5985422788448,
0.577893339283274));
#23020=CARTESIAN_POINT('Ctrl Pts',(-16.4008511615348,-13.7731735264444,
0.55751968383815));
#23021=CARTESIAN_POINT('Ctrl Pts',(-16.6132862462162,-13.9018579856258,
0.548728405588926));
#23022=CARTESIAN_POINT('Ctrl Pts',(-16.9816699619906,-14.2349802270737,
0.52834069438543));
#23023=CARTESIAN_POINT('Ctrl Pts',(-17.1330265348185,-14.4375333643221,
0.517510543285457));
#23024=CARTESIAN_POINT('Ctrl Pts',(-17.3523384611631,-14.8940137705683,
0.495729873499502));
#23025=CARTESIAN_POINT('Ctrl Pts',(-17.4162475186526,-15.1444779572253,
0.484995974066794));
#23026=CARTESIAN_POINT('Ctrl Pts',(-17.4421185607441,-15.6442929464891,
0.465768343155524));
#23027=CARTESIAN_POINT('Ctrl Pts',(-17.4083000036084,-15.8886689111737,
0.456344488448985));
#23028=CARTESIAN_POINT('Ctrl Pts',(-17.2484328204734,-16.3602738343215,
0.43528084812928));
#23029=CARTESIAN_POINT('Ctrl Pts',(-17.1206457356298,-16.581940728719,0.42424503368158));
#23030=CARTESIAN_POINT('Ctrl Pts',(-16.7856687235223,-16.9645889729791,
0.40272781217544));
#23031=CARTESIAN_POINT('Ctrl Pts',(-16.5812682858183,-17.1213576049014,
0.393012028285058));
#23032=CARTESIAN_POINT('Ctrl Pts',(-16.1307300450291,-17.3428309785426,
0.373579510976611));
#23033=CARTESIAN_POINT('Ctrl Pts',(-15.8902976971979,-17.4082697840594,
0.363209235298005));
#23034=CARTESIAN_POINT('Ctrl Pts',(-15.3881980760648,-17.4458200822429,
0.341552783758757));
#23035=CARTESIAN_POINT('Ctrl Pts',(-15.131028168327,-17.4137884812097,0.33046058729045));
#23036=CARTESIAN_POINT('Ctrl Pts',(-14.6530287770869,-17.2540504946331,
0.309843621619741));
#23037=CARTESIAN_POINT('Ctrl Pts',(-14.4356759586665,-17.1313390170145,
0.301024334084349));
#23038=CARTESIAN_POINT('Ctrl Pts',(-14.0571971873737,-16.8090342640234,
0.280822982029637));
#23039=CARTESIAN_POINT('Ctrl Pts',(-13.9002426531824,-16.6117620419649,
0.270069365086781));
#23040=CARTESIAN_POINT('Ctrl Pts',(-13.6672548469476,-16.162904088269,0.248278485904575));
#23041=CARTESIAN_POINT('Ctrl Pts',(-13.5956339333618,-15.9144966791606,
0.237455100685372));
#23042=CARTESIAN_POINT('Ctrl Pts',(-13.5701259723183,-15.6062624042348,
0.225391456350146));
#23043=CARTESIAN_POINT('Ctrl Pts',(-13.5679367061318,-15.5531033071595,
0.223358579470397));
#23044=CARTESIAN_POINT('Ctrl Pts',(-13.5679367061318,-15.5000000000002,
0.221374999999906));
#23045=CARTESIAN_POINT('Origin',(-15.5,-15.5000000000001,11.20575));
#23046=CARTESIAN_POINT('',(-13.5679367061318,-15.5000000000001,-0.278625000000104));
#23047=CARTESIAN_POINT('',(-13.5679367061318,-15.5000000000001,0.190124999999801));
#23048=CARTESIAN_POINT('',(-13.5679367061318,-15.5000000000001,11.20575));
#23049=CARTESIAN_POINT('Ctrl Pts',(-13.5679367061318,-15.5,0.190124999999802));
#23050=CARTESIAN_POINT('Ctrl Pts',(-13.5679367061318,-15.7052232055909,
0.197790747375155));
#23051=CARTESIAN_POINT('Ctrl Pts',(-13.6006312438213,-15.9094431243977,
0.206124105599912));
#23052=CARTESIAN_POINT('Ctrl Pts',(-13.7445092392226,-16.3458500952323,
0.225528168010807));
#23053=CARTESIAN_POINT('Ctrl Pts',(-13.8706006648954,-16.5687690248997,
0.236574181605254));
#23054=CARTESIAN_POINT('Ctrl Pts',(-14.1957983248934,-16.9462938014505,
0.257689124656201));
#23055=CARTESIAN_POINT('Ctrl Pts',(-14.3891741439701,-17.099606802076,0.267213101031626));
#23056=CARTESIAN_POINT('Ctrl Pts',(-14.8328987043056,-17.3312210666003,
0.286351732158258));
#23057=CARTESIAN_POINT('Ctrl Pts',(-15.0810963874241,-17.4033891896781,
0.297056940587791));
#23058=CARTESIAN_POINT('Ctrl Pts',(-15.5859112111092,-17.4463663432178,
0.318830503652362));
#23059=CARTESIAN_POINT('Ctrl Pts',(-15.837491754929,-17.4188098289699,0.329681620893124));
#23060=CARTESIAN_POINT('Ctrl Pts',(-16.3114416099339,-17.2705600347065,
0.350123922848628));
#23061=CARTESIAN_POINT('Ctrl Pts',(-16.529916123996,-17.1530549287719,0.35892246930463));
#23062=CARTESIAN_POINT('Ctrl Pts',(-16.9202726297616,-16.8349526369193,
0.379222999836032));
#23063=CARTESIAN_POINT('Ctrl Pts',(-17.0854512100821,-16.6338441663765,
0.39029727189281));
#23064=CARTESIAN_POINT('Ctrl Pts',(-17.3225641667436,-16.1874197433201,
0.412086213416735));
#23065=CARTESIAN_POINT('Ctrl Pts',(-17.3956324394973,-15.9481982603314,
0.422597688314646));
#23066=CARTESIAN_POINT('Ctrl Pts',(-17.4478128352923,-15.451075784191,0.442292129850996));
#23067=CARTESIAN_POINT('Ctrl Pts',(-17.4248413113893,-15.1977325915623,
0.451571409240311));
#23068=CARTESIAN_POINT('Ctrl Pts',(-17.2822086107981,-14.7117348553562,
0.472800990486158));
#23069=CARTESIAN_POINT('Ctrl Pts',(-17.1630032804558,-14.4841033890508,
0.483874527712175));
#23070=CARTESIAN_POINT('Ctrl Pts',(-16.8491384993424,-14.0954494858791,
0.505160775836539));
#23071=CARTESIAN_POINT('Ctrl Pts',(-16.66030462317,-13.9358452837369,0.515078993620071));
#23072=CARTESIAN_POINT('Ctrl Pts',(-16.2236425461124,-13.6903827463216,
0.533913007255616));
#23073=CARTESIAN_POINT('Ctrl Pts',(-15.9778499407047,-13.6105539996565,
0.54451448039696));
#23074=CARTESIAN_POINT('Ctrl Pts',(-15.4739117712162,-13.5518158441319,
0.566250231803577));
#23075=CARTESIAN_POINT('Ctrl Pts',(-15.2208352901079,-13.5717427947093,
0.577165871485754));
#23076=CARTESIAN_POINT('Ctrl Pts',(-14.7426848689165,-13.7057278794303,
0.597789351347446));
#23077=CARTESIAN_POINT('Ctrl Pts',(-14.5214408844322,-13.8161488953131,
0.60666457334335));
#23078=CARTESIAN_POINT('Ctrl Pts',(-14.1213400688703,-14.1219606735901,
0.626716158351838));
#23079=CARTESIAN_POINT('Ctrl Pts',(-13.9495491173577,-14.3185686119017,
0.637764922719137));
#23080=CARTESIAN_POINT('Ctrl Pts',(-13.6984440207755,-14.7590310485599,
0.659632917824817));
#23081=CARTESIAN_POINT('Ctrl Pts',(-13.6181551918391,-14.9966959458154,
0.670241966963291));
#23082=CARTESIAN_POINT('Ctrl Pts',(-13.5736457522819,-15.3284077888479,
0.683592357862467));
#23083=CARTESIAN_POINT('Ctrl Pts',(-13.5679367061318,-15.4142441778546,
0.686921743980885));
#23084=CARTESIAN_POINT('Ctrl Pts',(-13.5679367061318,-15.5,0.690124999999813));
#23085=CARTESIAN_POINT('Ctrl Pts',(-13.5679367061318,-15.5000000000002,
0.221374999999905));
#23086=CARTESIAN_POINT('Ctrl Pts',(-13.5679367061318,-15.3093450219841,
0.214253422821946));
#23087=CARTESIAN_POINT('Ctrl Pts',(-13.5961535791236,-15.1194546080678,
0.206551882563236));
#23088=CARTESIAN_POINT('Ctrl Pts',(-13.7256105048354,-14.6948718228171,
0.187900494766885));
#23089=CARTESIAN_POINT('Ctrl Pts',(-13.845972474099,-14.4700098899864,0.176905464582649));
#23090=CARTESIAN_POINT('Ctrl Pts',(-14.1696924220725,-14.0753526087545,
0.155182435506234));
#23091=CARTESIAN_POINT('Ctrl Pts',(-14.3714266003534,-13.9107790534924,
0.145052382155262));
#23092=CARTESIAN_POINT('Ctrl Pts',(-14.8173319842844,-13.6758632411833,
0.125819688220126));
#23093=CARTESIAN_POINT('Ctrl Pts',(-15.0551292056848,-13.6037990123402,
0.115563070240994));
#23094=CARTESIAN_POINT('Ctrl Pts',(-15.5544792855134,-13.5518334963291,
0.0940252113186381));
#23095=CARTESIAN_POINT('Ctrl Pts',(-15.8116932976136,-13.5761558232251,
0.0829311125505648));
#23096=CARTESIAN_POINT('Ctrl Pts',(-16.2949297861469,-13.7215598038885,
0.0620882615396313));
#23097=CARTESIAN_POINT('Ctrl Pts',(-16.5170608749109,-13.8385708543143,
0.0531675695570689));
#23098=CARTESIAN_POINT('Ctrl Pts',(-16.904996700699,-14.1505967904306,0.0331462145940504));
#23099=CARTESIAN_POINT('Ctrl Pts',(-17.0670614606798,-14.3427581395106,
0.0224732986365848));
#23100=CARTESIAN_POINT('Ctrl Pts',(-17.3126898339284,-14.7840616511319,
0.000691997092672782));
#23101=CARTESIAN_POINT('Ctrl Pts',(-17.3915129004033,-15.0303088815555,
-0.0102060193438629));
#23102=CARTESIAN_POINT('Ctrl Pts',(-17.4473055261676,-15.5280187234508,
-0.030000301840267));
#23103=CARTESIAN_POINT('Ctrl Pts',(-17.4281050083167,-15.7742335763025,
-0.0389538708323471));
#23104=CARTESIAN_POINT('Ctrl Pts',(-17.2969077105388,-16.2532901710004,
-0.0596775634460382));
#23105=CARTESIAN_POINT('Ctrl Pts',(-17.1834947936056,-16.4808992970974,
-0.0706253476363654));
#23106=CARTESIAN_POINT('Ctrl Pts',(-16.8732369844076,-16.882970778423,-0.092334997934469));
#23107=CARTESIAN_POINT('Ctrl Pts',(-16.6781753239889,-17.0524923786021,
-0.102808198443676));
#23108=CARTESIAN_POINT('Ctrl Pts',(-16.2425026231762,-17.3005030647046,
-0.121599538518457));
#23109=CARTESIAN_POINT('Ctrl Pts',(-16.0080032116997,-17.3801675178151,
-0.131713916077958));
#23110=CARTESIAN_POINT('Ctrl Pts',(-15.5123656482203,-17.448772467442,-0.153091647553434));
#23111=CARTESIAN_POINT('Ctrl Pts',(-15.2553808902943,-17.4333995515062,
-0.164175858180371));
#23112=CARTESIAN_POINT('Ctrl Pts',(-14.7662503095724,-17.3048200985618,
-0.185272931892274));
#23113=CARTESIAN_POINT('Ctrl Pts',(-14.5384527979055,-17.1944566841175,
-0.194401543736984));
#23114=CARTESIAN_POINT('Ctrl Pts',(-14.1397272750994,-16.8943347846072,
-0.214210934043039));
#23115=CARTESIAN_POINT('Ctrl Pts',(-13.9720032632392,-16.7081889662025,
-0.224781197374756));
#23116=CARTESIAN_POINT('Ctrl Pts',(-13.7111048247492,-16.2741834166746,
-0.246619209105808));
#23117=CARTESIAN_POINT('Ctrl Pts',(-13.6237773095579,-16.0284985545294,
-0.257679625291989));
#23118=CARTESIAN_POINT('Ctrl Pts',(-13.5743830168529,-15.6823226735556,
-0.271675640781532));
#23119=CARTESIAN_POINT('Ctrl Pts',(-13.5679367061318,-15.5911253192395,
-0.275221175979445));
#23120=CARTESIAN_POINT('Ctrl Pts',(-13.5679367061318,-15.5000000000001,
-0.278625000000103));
#23121=CARTESIAN_POINT('Origin',(-15.5,-15.5000000000001,11.20575));
#23122=CARTESIAN_POINT('',(-13.5679367061318,-15.5000000000001,-0.778625000000111));
#23123=CARTESIAN_POINT('',(-13.5679367061318,-15.5000000000214,-0.30987499999861));
#23124=CARTESIAN_POINT('',(-13.5679367061318,-15.5000000000001,11.20575));
#23125=CARTESIAN_POINT('Ctrl Pts',(-13.5679367061318,-15.5000000000426,
-0.309874999998611));
#23126=CARTESIAN_POINT('Ctrl Pts',(-13.5679367061372,-15.7451189900435,
-0.30071901664447));
#23127=CARTESIAN_POINT('Ctrl Pts',(-13.614584910455,-15.9880788836298,-0.290637672395915));
#23128=CARTESIAN_POINT('Ctrl Pts',(-13.7998506160078,-16.4525087353532,
-0.269294302322098));
#23129=CARTESIAN_POINT('Ctrl Pts',(-13.9401358945745,-16.6681650113367,
-0.25821346913606));
#23130=CARTESIAN_POINT('Ctrl Pts',(-14.2937988135869,-17.0300510391149,
-0.237068805018314));
#23131=CARTESIAN_POINT('Ctrl Pts',(-14.5027181075032,-17.1737375672253,
-0.227889545454481));
#23132=CARTESIAN_POINT('Ctrl Pts',(-14.9610456268796,-17.3718881645073,
-0.20812106267792));
#23133=CARTESIAN_POINT('Ctrl Pts',(-15.205635116172,-17.4255568606796,-0.19757148207894));
#23134=CARTESIAN_POINT('Ctrl Pts',(-15.7028273877143,-17.437485526191,-0.176126693273804));
#23135=CARTESIAN_POINT('Ctrl Pts',(-15.950828380533,-17.3951930471992,-0.165429968447499));
#23136=CARTESIAN_POINT('Ctrl Pts',(-16.4162168450069,-17.21903750586,-0.145356934524352));
#23137=CARTESIAN_POINT('Ctrl Pts',(-16.6293413959127,-17.0871779138879,
-0.136472617530252));
#23138=CARTESIAN_POINT('Ctrl Pts',(-16.9997020048591,-16.7447233478946,
-0.115693680499808));
#23139=CARTESIAN_POINT('Ctrl Pts',(-17.1512859841672,-16.5352235199722,
-0.104599143917264));
#23140=CARTESIAN_POINT('Ctrl Pts',(-17.3599329092897,-16.0781299074099,
-0.083025569156745));
#23141=CARTESIAN_POINT('Ctrl Pts',(-17.4184418092007,-15.8364334516317,
-0.07273563190757));
#23142=CARTESIAN_POINT('Ctrl Pts',(-17.4419572678445,-15.3335771418076,
-0.0534451981390733));
#23143=CARTESIAN_POINT('Ctrl Pts',(-17.4026393126746,-15.0770448720175,
-0.0434417100341766));
#23144=CARTESIAN_POINT('Ctrl Pts',(-17.2273302215969,-14.5982616364446,
-0.0217769181316164));
#23145=CARTESIAN_POINT('Ctrl Pts',(-17.0946215718083,-14.3801849192583,
-0.0107690704262966));
#23146=CARTESIAN_POINT('Ctrl Pts',(-16.7583973031523,-14.0137016048738,
0.0101712371104099));
#23147=CARTESIAN_POINT('Ctrl Pts',(-16.5604348396371,-13.8665662971671,
0.0193865553792948));
#23148=CARTESIAN_POINT('Ctrl Pts',(-16.1097762694872,-13.6488960345413,
0.0388242627075219));
#23149=CARTESIAN_POINT('Ctrl Pts',(-15.8594139033153,-13.5844810246989,
0.0496228377751917));
#23150=CARTESIAN_POINT('Ctrl Pts',(-15.3542160204943,-13.557297522928,0.0714129228629977));
#23151=CARTESIAN_POINT('Ctrl Pts',(-15.1043600205154,-13.5924291711368,
0.0821896574542814));
#23152=CARTESIAN_POINT('Ctrl Pts',(-14.6347353821394,-13.7549549306401,
0.102445405107847));
#23153=CARTESIAN_POINT('Ctrl Pts',(-14.4190031858112,-13.8797188217568,
0.111248274994699));
#23154=CARTESIAN_POINT('Ctrl Pts',(-14.0387180251795,-14.2102312356741,
0.131795166002626));
#23155=CARTESIAN_POINT('Ctrl Pts',(-13.8803875205859,-14.4157066951989,
0.1428848743003));
#23156=CARTESIAN_POINT('Ctrl Pts',(-13.6576628179058,-14.8677637645241,
0.164573917775743));
#23157=CARTESIAN_POINT('Ctrl Pts',(-13.5919750720436,-15.1083498919248,
0.174977198895978));
#23158=CARTESIAN_POINT('Ctrl Pts',(-13.5697540327492,-15.4031822744542,
0.186469354010744));
#23159=CARTESIAN_POINT('Ctrl Pts',(-13.5679367061318,-15.4516175612206,
0.188317760160533));
#23160=CARTESIAN_POINT('Ctrl Pts',(-13.5679367061318,-15.5,0.190124999999802));
#23161=CARTESIAN_POINT('Ctrl Pts',(-13.5679367061318,-15.5000000000001,
-0.278625000000104));
#23162=CARTESIAN_POINT('Ctrl Pts',(-13.5679367061318,-15.3467892595674,
-0.284347914365298));
#23163=CARTESIAN_POINT('Ctrl Pts',(-13.5861582264615,-15.1938118278,-0.290455077224571));
#23164=CARTESIAN_POINT('Ctrl Pts',(-13.6816903722921,-14.8002115586198,
-0.307217550198197));
#23165=CARTESIAN_POINT('Ctrl Pts',(-13.7879612606778,-14.570016446838,-0.31810790506839));
#23166=CARTESIAN_POINT('Ctrl Pts',(-14.0854112713272,-14.1593674320811,
-0.339861742263403));
#23167=CARTESIAN_POINT('Ctrl Pts',(-14.2752366149402,-13.9839732653664,
-0.350507031707781));
#23168=CARTESIAN_POINT('Ctrl Pts',(-14.702688554669,-13.7231840671468,-0.369466729782478));
#23169=CARTESIAN_POINT('Ctrl Pts',(-14.9340075270615,-13.6365422674356,
-0.379212735887829));
#23170=CARTESIAN_POINT('Ctrl Pts',(-15.4259040929271,-13.5527035685258,
-0.400429111468748));
#23171=CARTESIAN_POINT('Ctrl Pts',(-15.6824101509155,-13.5598498556791,
-0.4114926748787));
#23172=CARTESIAN_POINT('Ctrl Pts',(-16.1685436048833,-13.6708737218792,
-0.432460477172683));
#23173=CARTESIAN_POINT('Ctrl Pts',(-16.3943923195072,-13.7700581638794,
-0.441627804189991));
#23174=CARTESIAN_POINT('Ctrl Pts',(-16.8066128739237,-14.0539091259065,
-0.461120454984909));
#23175=CARTESIAN_POINT('Ctrl Pts',(-16.986511157224,-14.2395717541843,-0.471935218622489));
#23176=CARTESIAN_POINT('Ctrl Pts',(-17.2601171116814,-14.6649766986924,
-0.493726018975322));
#23177=CARTESIAN_POINT('Ctrl Pts',(-17.3532344935945,-14.899325305048,-0.504487853149966));
#23178=CARTESIAN_POINT('Ctrl Pts',(-17.4445879149158,-15.3879151902704,
-0.524708376151779));
#23179=CARTESIAN_POINT('Ctrl Pts',(-17.4429655287095,-15.6373703519541,
-0.533521108453184));
#23180=CARTESIAN_POINT('Ctrl Pts',(-17.3439130071985,-16.1314699148968,
-0.554113473610937));
#23181=CARTESIAN_POINT('Ctrl Pts',(-17.2437932710759,-16.370599259013,-0.56520489573948));
#23182=CARTESIAN_POINT('Ctrl Pts',(-16.9614315558214,-16.7876645309164,
-0.586873008257939));
#23183=CARTESIAN_POINT('Ctrl Pts',(-16.7850271271049,-16.9637580970129,
-0.597254988531082));
#23184=CARTESIAN_POINT('Ctrl Pts',(-16.368955630774,-17.2443400456584,-0.616708580146808));
#23185=CARTESIAN_POINT('Ctrl Pts',(-16.131560971349,-17.3436265739668,-0.62638464969034));
#23186=CARTESIAN_POINT('Ctrl Pts',(-15.6332086940277,-17.4440644805447,
-0.647879471612186));
#23187=CARTESIAN_POINT('Ctrl Pts',(-15.3772600495196,-17.4447534368068,
-0.658918992820774));
#23188=CARTESIAN_POINT('Ctrl Pts',(-14.8884838631652,-17.3489811387507,
-0.680000780871976));
#23189=CARTESIAN_POINT('Ctrl Pts',(-14.6596166089138,-17.2568181637342,
-0.689459136163638));
#23190=CARTESIAN_POINT('Ctrl Pts',(-14.2388050986946,-16.9858620064432,
-0.708655396108797));
#23191=CARTESIAN_POINT('Ctrl Pts',(-14.0532686227974,-16.8058878838003,
-0.719379268396446));
#23192=CARTESIAN_POINT('Ctrl Pts',(-13.7662002684568,-16.3885881549385,
-0.741157641503204));
#23193=CARTESIAN_POINT('Ctrl Pts',(-13.6656892248834,-16.1564785080748,
-0.75199529423572));
#23194=CARTESIAN_POINT('Ctrl Pts',(-13.5827427724808,-15.7761115114099,
-0.767992040186503));
#23195=CARTESIAN_POINT('Ctrl Pts',(-13.5679367061318,-15.6381065098838,
-0.773466277268877));
#23196=CARTESIAN_POINT('Ctrl Pts',(-13.5679367061318,-15.5000000000001,
-0.778625000000112));
#23197=CARTESIAN_POINT('Origin',(-15.5,-15.5000000000001,11.20575));
#23198=CARTESIAN_POINT('',(-13.5679367061318,-15.5000000000001,-1.27862500000012));
#23199=CARTESIAN_POINT('',(-13.5679367061318,-15.5000000000001,-0.809875000000204));
#23200=CARTESIAN_POINT('',(-13.5679367061318,-15.5000000000001,11.20575));
#23201=CARTESIAN_POINT('Ctrl Pts',(-13.5679367061318,-15.5000000000002,
-0.809875000000203));
#23202=CARTESIAN_POINT('Ctrl Pts',(-13.5679367061318,-15.5387848588903,
-0.808426260665952));
#23203=CARTESIAN_POINT('Ctrl Pts',(-13.5691045537611,-15.5776081217819,
-0.806950901143784));
#23204=CARTESIAN_POINT('Ctrl Pts',(-13.5863172258655,-15.8627498107997,
-0.795928734529179));
#23205=CARTESIAN_POINT('Ctrl Pts',(-13.6482441649587,-16.1039441624044,
-0.785583839426325));
#23206=CARTESIAN_POINT('Ctrl Pts',(-13.8636040208235,-16.5586938389716,
-0.763953047887124));
#23207=CARTESIAN_POINT('Ctrl Pts',(-14.0184106751405,-16.7663048606793,
-0.752859564438659));
#23208=CARTESIAN_POINT('Ctrl Pts',(-14.3935142993233,-17.1030886658291,
-0.732190161230552));
#23209=CARTESIAN_POINT('Ctrl Pts',(-14.6078734364707,-17.2315636886461,
-0.723354008700389));
#23210=CARTESIAN_POINT('Ctrl Pts',(-15.0752831240916,-17.401259102443,-0.703193795820516));
#23211=CARTESIAN_POINT('Ctrl Pts',(-15.3241884796656,-17.4401670421017,
-0.692458064216716));
#23212=CARTESIAN_POINT('Ctrl Pts',(-15.8293918059364,-17.4209116308134,
-0.670667744343207));
#23213=CARTESIAN_POINT('Ctrl Pts',(-16.0807480284637,-17.3604173282468,
-0.659826302479602));
#23214=CARTESIAN_POINT('Ctrl Pts',(-16.5348352725855,-17.1497816929782,
-0.640240710332132));
#23215=CARTESIAN_POINT('Ctrl Pts',(-16.7351193667876,-17.0057085011961,
-0.631148276498325));
#23216=CARTESIAN_POINT('Ctrl Pts',(-17.0767669839639,-16.6447314320374,
-0.610296685602489));
#23217=CARTESIAN_POINT('Ctrl Pts',(-17.2126942752493,-16.4291281586244,
-0.599311816112374));
#23218=CARTESIAN_POINT('Ctrl Pts',(-17.3960714153678,-15.9522914740598,
-0.577545739488913));
#23219=CARTESIAN_POINT('Ctrl Pts',(-17.4394863853225,-15.6949512567246,
-0.567317142600478));
#23220=CARTESIAN_POINT('Ctrl Pts',(-17.4229690903241,-15.1907605692907,
-0.548127787168025));
#23221=CARTESIAN_POINT('Ctrl Pts',(-17.367985737015,-14.9485965706548,-0.537896417242245));
#23222=CARTESIAN_POINT('Ctrl Pts',(-17.1662821041941,-14.4891878782664,
-0.516386105083534));
#23223=CARTESIAN_POINT('Ctrl Pts',(-17.0180420352629,-14.2777915836234,
-0.505292843771123));
#23224=CARTESIAN_POINT('Ctrl Pts',(-16.6526099917287,-13.9295152530064,
-0.484402733995946));
#23225=CARTESIAN_POINT('Ctrl Pts',(-16.4407479085027,-13.7941507738711,
-0.475451133965726));
#23226=CARTESIAN_POINT('Ctrl Pts',(-15.977452801173,-13.6113838875222,-0.45546839026715));
#23227=CARTESIAN_POINT('Ctrl Pts',(-15.7304237057036,-13.5656468617911,
-0.444813585105682));
#23228=CARTESIAN_POINT('Ctrl Pts',(-15.2255315160609,-13.5704710073907,
-0.423036685109488));
#23229=CARTESIAN_POINT('Ctrl Pts',(-14.9725259783181,-13.6237792291611,
-0.412124105341109));
#23230=CARTESIAN_POINT('Ctrl Pts',(-14.5122846645609,-13.8215336428728,
-0.392273077202022));
#23231=CARTESIAN_POINT('Ctrl Pts',(-14.3077326406348,-13.9600852553974,
-0.383350131532138));
#23232=CARTESIAN_POINT('Ctrl Pts',(-13.9563854884099,-14.311092329695,-0.362661772922435));
#23233=CARTESIAN_POINT('Ctrl Pts',(-13.8147703346551,-14.5221235135244,
-0.351725021873736));
#23234=CARTESIAN_POINT('Ctrl Pts',(-13.6188695990396,-14.9904064163149,
-0.330008374038385));
#23235=CARTESIAN_POINT('Ctrl Pts',(-13.5679791180276,-15.2437584839142,
-0.319447360159011));
#23236=CARTESIAN_POINT('Ctrl Pts',(-13.5679367149643,-15.4997866765026,
-0.309882968510016));
#23237=CARTESIAN_POINT('Ctrl Pts',(-13.5679367061318,-15.4998933384699,
-0.30987898415171));
#23238=CARTESIAN_POINT('Ctrl Pts',(-13.5679367061318,-15.5000000000426,
-0.309874999998609));
#23239=CARTESIAN_POINT('Ctrl Pts',(-13.5679367061318,-15.5000000000001,
-0.778625000000111));
#23240=CARTESIAN_POINT('Ctrl Pts',(-13.5679367061318,-15.3931460598282,
-0.78261633864556));
#23241=CARTESIAN_POINT('Ctrl Pts',(-13.5768002208838,-15.2862458062684,
-0.786800556839377));
#23242=CARTESIAN_POINT('Ctrl Pts',(-13.6371564582819,-14.9264097344303,
-0.801543228537963));
#23243=CARTESIAN_POINT('Ctrl Pts',(-13.7301105174323,-14.6835020771365,
-0.812621248617171));
#23244=CARTESIAN_POINT('Ctrl Pts',(-14.0004851886932,-14.2567488542947,
-0.834392726004424));
#23245=CARTESIAN_POINT('Ctrl Pts',(-14.1720617651617,-14.0749328108105,
-0.844884342293561));
#23246=CARTESIAN_POINT('Ctrl Pts',(-14.5783544246733,-13.7832732834677,
-0.864540827803848));
#23247=CARTESIAN_POINT('Ctrl Pts',(-14.8102645191385,-13.6776776438874,
-0.873875479411993));
#23248=CARTESIAN_POINT('Ctrl Pts',(-15.303462333774,-13.5612057991406,-0.895147980171542));
#23249=CARTESIAN_POINT('Ctrl Pts',(-15.5600993610212,-13.5521973966285,
-0.906217192554563));
#23250=CARTESIAN_POINT('Ctrl Pts',(-16.0528776436279,-13.6325934594164,
-0.927471598149985));
#23251=CARTESIAN_POINT('Ctrl Pts',(-16.2849105088377,-13.7176559738657,
-0.937309340891435));
#23252=CARTESIAN_POINT('Ctrl Pts',(-16.7142424070008,-13.9755352342243,
-0.956200886398405));
#23253=CARTESIAN_POINT('Ctrl Pts',(-16.9052695296546,-14.1496041206411,
-0.96682258979334));
#23254=CARTESIAN_POINT('Ctrl Pts',(-17.2056519899816,-14.5583089440343,
-0.988567046072784));
#23255=CARTESIAN_POINT('Ctrl Pts',(-17.3135593943002,-14.7879324233922,
-0.99947134155624));
#23256=CARTESIAN_POINT('Ctrl Pts',(-17.4338950578804,-15.2696786471809,
-1.02006125965414));
#23257=CARTESIAN_POINT('Ctrl Pts',(-17.4474891140443,-15.51669804182,-1.0289160540572));
#23258=CARTESIAN_POINT('Ctrl Pts',(-17.3798092846713,-16.0156874200649,
-1.04901448949424));
#23259=CARTESIAN_POINT('Ctrl Pts',(-17.2940873360173,-16.2621352120533,
-1.0600687780929));
#23260=CARTESIAN_POINT('Ctrl Pts',(-17.0359029312521,-16.6981549445161,
-1.08192349548471));
#23261=CARTESIAN_POINT('Ctrl Pts',(-16.8692878718213,-16.8855107792871,
-1.09251504127557));
#23262=CARTESIAN_POINT('Ctrl Pts',(-16.4727055985413,-17.1880123648935,
-1.11236709943196));
#23263=CARTESIAN_POINT('Ctrl Pts',(-16.2460520786798,-17.2997096592015,
-1.12144644417648));
#23264=CARTESIAN_POINT('Ctrl Pts',(-15.7580841551168,-17.4316717914396,
-1.14249337041296));
#23265=CARTESIAN_POINT('Ctrl Pts',(-15.5010293351169,-17.4488346169957,
-1.15358060294202));
#23266=CARTESIAN_POINT('Ctrl Pts',(-15.0046042921056,-17.3835494183322,
-1.1749922998132));
#23267=CARTESIAN_POINT('Ctrl Pts',(-14.7694246895426,-17.3053971664748,
-1.18513601522654));
#23268=CARTESIAN_POINT('Ctrl Pts',(-14.3319804116802,-17.0601513560859,
-1.20400376657688));
#23269=CARTESIAN_POINT('Ctrl Pts',(-14.1358043637621,-16.8918928497275,
-1.21438674925062));
#23270=CARTESIAN_POINT('Ctrl Pts',(-13.8228284520313,-16.491712693971,-1.23608437075356));
#23271=CARTESIAN_POINT('Ctrl Pts',(-13.7078902727458,-16.2646868044627,
-1.24704326282161));
#23272=CARTESIAN_POINT('Ctrl Pts',(-13.5920235017517,-15.8517814521893,
-1.26496537710754));
#23273=CARTESIAN_POINT('Ctrl Pts',(-13.5679367061318,-15.6761515068699,
-1.27204517415848));
#23274=CARTESIAN_POINT('Ctrl Pts',(-13.5679367061318,-15.5,-1.27862500000012));
#23275=CARTESIAN_POINT('Origin',(-15.5,-15.5000000000001,11.20575));
#23276=CARTESIAN_POINT('',(-13.5679367061318,-15.5000000000001,-1.77862500000012));
#23277=CARTESIAN_POINT('',(-13.5679367061318,-15.5000000000001,-1.30987500000021));
#23278=CARTESIAN_POINT('',(-13.5679367061318,-15.5000000000001,11.20575));
#23279=CARTESIAN_POINT('',(-13.9369173237898,-16.6356236641577,-2.22824839946604));
#23280=CARTESIAN_POINT('Ctrl Pts',(-13.5679367061318,-15.5000000000001,
-1.77862500000012));
#23281=CARTESIAN_POINT('Ctrl Pts',(-13.5679367061318,-15.471311010133,-1.77969662612613));
#23282=CARTESIAN_POINT('Ctrl Pts',(-13.5685756992843,-15.4425999918154,
-1.78078285554243));
#23283=CARTESIAN_POINT('Ctrl Pts',(-13.5812658328334,-15.1581590394341,
-1.79168131481371));
#23284=CARTESIAN_POINT('Ctrl Pts',(-13.6433835358851,-14.907254339342,-1.8023930366865));
#23285=CARTESIAN_POINT('Ctrl Pts',(-13.8594981527771,-14.4490712177349,
-1.82416835554489));
#23286=CARTESIAN_POINT('Ctrl Pts',(-14.0095359247466,-14.2453192498238,
-1.83501484571359));
#23287=CARTESIAN_POINT('Ctrl Pts',(-14.3755767714584,-13.9097095421912,
-1.85544494572747));
#23288=CARTESIAN_POINT('Ctrl Pts',(-14.5868970850357,-13.7796534962008,
-1.86424124387686));
#23289=CARTESIAN_POINT('Ctrl Pts',(-15.0579406868171,-13.6016248094559,
-1.88455819395111));
#23290=CARTESIAN_POINT('Ctrl Pts',(-15.3147261186882,-13.5596639922644,
-1.89563380729006));
#23291=CARTESIAN_POINT('Ctrl Pts',(-15.8197591256804,-13.5785378998648,
-1.91741678098951));
#23292=CARTESIAN_POINT('Ctrl Pts',(-16.0633065482656,-13.6353374705016,
-1.92792141539418));
#23293=CARTESIAN_POINT('Ctrl Pts',(-16.5196132328428,-13.839629489679,-1.94760273596416));
#23294=CARTESIAN_POINT('Ctrl Pts',(-16.7273518612851,-13.9867054192994,
-1.95690084583355));
#23295=CARTESIAN_POINT('Ctrl Pts',(-17.0761951411224,-14.3540458832977,
-1.97814531088906));
#23296=CARTESIAN_POINT('Ctrl Pts',(-17.2132390451091,-14.571339412322,-1.98921739761544));
#23297=CARTESIAN_POINT('Ctrl Pts',(-17.3918917773575,-15.0377637909672,
-2.01049265502812));
#23298=CARTESIAN_POINT('Ctrl Pts',(-17.435193117581,-15.2811490466372,-2.02038271493815));
#23299=CARTESIAN_POINT('Ctrl Pts',(-17.4284331862708,-15.7819930621726,
-2.03923663515864));
#23300=CARTESIAN_POINT('Ctrl Pts',(-17.3741617364932,-16.0346645552799,
-2.04984514099419));
#23301=CARTESIAN_POINT('Ctrl Pts',(-17.1721421782215,-16.5000089832968,
-2.0715839852006));
#23302=CARTESIAN_POINT('Ctrl Pts',(-17.0279622251882,-16.7088902829552,
-2.08249574333672));
#23303=CARTESIAN_POINT('Ctrl Pts',(-16.6721862676384,-17.055293507434,-2.10310764446866));
#23304=CARTESIAN_POINT('Ctrl Pts',(-16.4656337928419,-17.1913024698242,
-2.11197549348959));
#23305=CARTESIAN_POINT('Ctrl Pts',(-16.0003669869149,-17.3839588971727,
-2.13204328006278));
#23306=CARTESIAN_POINT('Ctrl Pts',(-15.7441588924868,-17.4339176131202,
-2.14309399180884));
#23307=CARTESIAN_POINT('Ctrl Pts',(-15.2372592425206,-17.4301770605002,
-2.16495747714662));
#23308=CARTESIAN_POINT('Ctrl Pts',(-14.9914303043227,-17.3804225881419,
-2.17556051738595));
#23309=CARTESIAN_POINT('Ctrl Pts',(-14.6006806199507,-17.2188593062006,
-2.19241424769643));
#23310=CARTESIAN_POINT('Ctrl Pts',(-14.4493679378134,-17.1307744675633,
-2.19870147392335));
#23311=CARTESIAN_POINT('Ctrl Pts',(-14.1693732820954,-16.9124347548105,
-2.21289549932969));
#23312=CARTESIAN_POINT('Ctrl Pts',(-14.0431460179722,-16.7818378043867,
-2.22049591927733));
#23313=CARTESIAN_POINT('Ctrl Pts',(-13.9369173213529,-16.6356236661969,
-2.22824840453255));
#23314=CARTESIAN_POINT('',(-13.936918850212,-16.6356257705295,-1.75949829183043));
#23315=CARTESIAN_POINT('',(-13.9369184637307,-16.6356252385745,-1.75949832116282));
#23316=CARTESIAN_POINT('Ctrl Pts',(-13.9369188502404,-16.6356257705685,
-1.75949829295574));
#23317=CARTESIAN_POINT('Ctrl Pts',(-14.0732165037119,-16.8232265616206,
-1.74955141913573));
#23318=CARTESIAN_POINT('Ctrl Pts',(-14.2421926306504,-16.9847823163706,
-1.73987267086344));
#23319=CARTESIAN_POINT('Ctrl Pts',(-14.6256885475374,-17.2378815903647,
-1.72214816701709));
#23320=CARTESIAN_POINT('Ctrl Pts',(-14.8362794639394,-17.3287014043756,
-1.71350244965326));
#23321=CARTESIAN_POINT('Ctrl Pts',(-15.3036899854226,-17.4385845729922,
-1.69334220080743));
#23322=CARTESIAN_POINT('Ctrl Pts',(-15.5584934383084,-17.4476198869581,
-1.68235207375454));
#23323=CARTESIAN_POINT('Ctrl Pts',(-16.0626255591007,-17.3662648208193,
-1.66060795688251));
#23324=CARTESIAN_POINT('Ctrl Pts',(-16.3065929189332,-17.2745029457009,
-1.65043016901726));
#23325=CARTESIAN_POINT('Ctrl Pts',(-16.733960549226,-17.0069230177967,-1.63121863353652));
#23326=CARTESIAN_POINT('Ctrl Pts',(-16.9157196559872,-16.8376064327553,
-1.62097431691818));
#23327=CARTESIAN_POINT('Ctrl Pts',(-17.2115388605544,-16.4321558772132,
-1.59944982869596));
#23328=CARTESIAN_POINT('Ctrl Pts',(-17.3197729456466,-16.1976492003971,
-1.58835608490565));
#23329=CARTESIAN_POINT('Ctrl Pts',(-17.4370349875307,-15.7067373188983,
-1.56749008537745));
#23330=CARTESIAN_POINT('Ctrl Pts',(-17.44753196976,-15.4557223788834,-1.55855468409502));
#23331=CARTESIAN_POINT('Ctrl Pts',(-17.3726902789254,-14.9634366275316,
-1.53855219877786));
#23332=CARTESIAN_POINT('Ctrl Pts',(-17.2880297167387,-14.7268219856977,
-1.52788809973699));
#23333=CARTESIAN_POINT('Ctrl Pts',(-17.0300046441309,-14.2927306055599,
-1.50610884865219));
#23334=CARTESIAN_POINT('Ctrl Pts',(-16.856734367155,-14.1008202908098,-1.49520365267543));
#23335=CARTESIAN_POINT('Ctrl Pts',(-16.4544579219336,-13.8024087055848,
-1.47538156930747));
#23336=CARTESIAN_POINT('Ctrl Pts',(-16.2319055093256,-13.6952482164327,
-1.46644338907461));
#23337=CARTESIAN_POINT('Ctrl Pts',(-15.751832329794,-13.5679372308724,-1.44573697721882));
#23338=CARTESIAN_POINT('Ctrl Pts',(-15.4981347275309,-13.5515962723609,
-1.43479454747422));
#23339=CARTESIAN_POINT('Ctrl Pts',(-14.994677988732,-13.6177050294596,-1.41307956103129));
#23340=CARTESIAN_POINT('Ctrl Pts',(-14.7500889892405,-13.7011232772003,
-1.40256300391622));
#23341=CARTESIAN_POINT('Ctrl Pts',(-14.316768691791,-13.9530518157519,-1.38380772364027));
#23342=CARTESIAN_POINT('Ctrl Pts',(-14.130076521834,-14.1156697545301,-1.37370723712004));
#23343=CARTESIAN_POINT('Ctrl Pts',(-13.8216873535977,-14.5094994028651,
-1.35234574472347));
#23344=CARTESIAN_POINT('Ctrl Pts',(-13.7058009544627,-14.7392900935936,
-1.34126312922345));
#23345=CARTESIAN_POINT('Ctrl Pts',(-13.5913602763723,-15.1530393767009,
-1.32334024636843));
#23346=CARTESIAN_POINT('Ctrl Pts',(-13.5679367061318,-15.3262907155802,
-1.31636360097145));
#23347=CARTESIAN_POINT('Ctrl Pts',(-13.5679367061318,-15.5000000000002,
-1.30987500000021));
#23348=CARTESIAN_POINT('Origin',(-15.5,-15.5000000000001,11.20575));
#23349=CARTESIAN_POINT('Ctrl Pts',(-13.5679367061318,-15.5000000000002,
-1.30987500000021));
#23350=CARTESIAN_POINT('Ctrl Pts',(-13.5679367061318,-15.5762794463022,
-1.30702571712501));
#23351=CARTESIAN_POINT('Ctrl Pts',(-13.572453778509,-15.6526398620169,-1.30407599509047));
#23352=CARTESIAN_POINT('Ctrl Pts',(-13.6108964642078,-15.9751450143037,
-1.29120033868173));
#23353=CARTESIAN_POINT('Ctrl Pts',(-13.6874920713322,-16.2136336424646,
-1.28064016816177));
#23354=CARTESIAN_POINT('Ctrl Pts',(-13.9314508386655,-16.6572017226074,
-1.258810284233));
#23355=CARTESIAN_POINT('Ctrl Pts',(-14.099870499122,-16.8561400321267,-1.24774717789517));
#23356=CARTESIAN_POINT('Ctrl Pts',(-14.494999203763,-17.1682578349238,-1.22756727057358));
#23357=CARTESIAN_POINT('Ctrl Pts',(-14.7148147242685,-17.2823015923697,
-1.21874144035887));
#23358=CARTESIAN_POINT('Ctrl Pts',(-15.1908203591575,-17.4236222475759,
-1.19821046895298));
#23359=CARTESIAN_POINT('Ctrl Pts',(-15.4431561242079,-17.4474792441872,
-1.18732677767453));
#23360=CARTESIAN_POINT('Ctrl Pts',(-15.9476066067072,-17.3968415255677,
-1.16556892929466));
#23361=CARTESIAN_POINT('Ctrl Pts',(-16.1946658536917,-17.3209404210907,
-1.15491282364461));
#23362=CARTESIAN_POINT('Ctrl Pts',(-16.634975992356,-17.0825888205037,-1.13592146261012));
#23363=CARTESIAN_POINT('Ctrl Pts',(-16.8261410473283,-16.9262354938107,
-1.12621674018239));
#23364=CARTESIAN_POINT('Ctrl Pts',(-17.1458740756934,-16.5433162646628,
-1.10501814661225));
#23365=CARTESIAN_POINT('Ctrl Pts',(-17.2686545572972,-16.3180913830561,
-1.09395740174899));
#23366=CARTESIAN_POINT('Ctrl Pts',(-17.4197688669729,-15.8338668009503,
-1.07261114005866));
#23367=CARTESIAN_POINT('Ctrl Pts',(-17.4469489334785,-15.5797125649259,
-1.06317354299107));
#23368=CARTESIAN_POINT('Ctrl Pts',(-17.4022619456061,-15.0810498002785,
-1.04358316874007));
#23369=CARTESIAN_POINT('Ctrl Pts',(-17.3330146958169,-14.8410934256471,
-1.03312664703887));
#23370=CARTESIAN_POINT('Ctrl Pts',(-17.103339970937,-14.3916950333676,-1.01138703028765));
#23371=CARTESIAN_POINT('Ctrl Pts',(-16.9416955633754,-14.1882964703834,
-1.000303433491));
#23372=CARTESIAN_POINT('Ctrl Pts',(-16.5565376106631,-13.8637511465985,
-0.979874346405003));
#23373=CARTESIAN_POINT('Ctrl Pts',(-16.3394926778595,-13.742491770238,-0.97108381540342));
#23374=CARTESIAN_POINT('Ctrl Pts',(-15.8677779963459,-13.586815206346,-0.950737920464291));
#23375=CARTESIAN_POINT('Ctrl Pts',(-15.617066435513,-13.5553093488706,-0.939924284008528));
#23376=CARTESIAN_POINT('Ctrl Pts',(-15.1119904982334,-13.5900705720839,
-0.918139458649265));
#23377=CARTESIAN_POINT('Ctrl Pts',(-14.8626360597541,-13.6582150358001,
-0.907384357299389));
#23378=CARTESIAN_POINT('Ctrl Pts',(-14.415286943223,-13.8825858943853,-0.888089392604112));
#23379=CARTESIAN_POINT('Ctrl Pts',(-14.2195307589344,-14.0326711922678,
-0.878736660945362));
#23380=CARTESIAN_POINT('Ctrl Pts',(-13.888558418963,-14.404439389832,-0.857712208531265));
#23381=CARTESIAN_POINT('Ctrl Pts',(-13.7589900789029,-14.624853845409,-0.846684762349222));
#23382=CARTESIAN_POINT('Ctrl Pts',(-13.6042442375735,-15.0687257239406,
-0.826767486822917));
#23383=CARTESIAN_POINT('Ctrl Pts',(-13.5679367061318,-15.2837368797497,
-0.817953123727358));
#23384=CARTESIAN_POINT('Ctrl Pts',(-13.5679367061318,-15.5000000000002,
-0.809875000000204));
#23385=CARTESIAN_POINT('Ctrl Pts',(-13.5679367061318,-15.5,-1.27862500000012));
#23386=CARTESIAN_POINT('Ctrl Pts',(-13.5679367061318,-15.4323298280073,
-1.28115269876523));
#23387=CARTESIAN_POINT('Ctrl Pts',(-13.5714917240295,-15.3645884444351,
-1.28375972464103));
#23388=CARTESIAN_POINT('Ctrl Pts',(-13.6055206308558,-15.0424237115268,
-1.29652747821543));
#23389=CARTESIAN_POINT('Ctrl Pts',(-13.682764182422,-14.7956826309076,-1.30740987789996));
#23390=CARTESIAN_POINT('Ctrl Pts',(-13.9256313093853,-14.3526857719949,
-1.32919488267955));
#23391=CARTESIAN_POINT('Ctrl Pts',(-14.0865851623327,-14.1593885173579,
-1.33988627066607));
#23392=CARTESIAN_POINT('Ctrl Pts',(-14.4724436684446,-13.8450923874922,
-1.35994762542375));
#23393=CARTESIAN_POINT('Ctrl Pts',(-14.6935102311441,-13.7268197743643,
-1.36883965888249));
#23394=CARTESIAN_POINT('Ctrl Pts',(-15.1756013089239,-13.5782346236499,
-1.3896331062862));
#23395=CARTESIAN_POINT('Ctrl Pts',(-15.4328247709742,-13.552207619699,-1.40072761264747));
#23396=CARTESIAN_POINT('Ctrl Pts',(-15.9328184705041,-13.6009921106949,
-1.42229323203465));
#23397=CARTESIAN_POINT('Ctrl Pts',(-16.1712147184524,-13.671597546139,-1.43257568709642));
#23398=CARTESIAN_POINT('Ctrl Pts',(-16.618156863512,-13.9035318490541,-1.45185309838682));
#23399=CARTESIAN_POINT('Ctrl Pts',(-16.8204876400156,-14.0663572621764,
-1.46188465464224));
#23400=CARTESIAN_POINT('Ctrl Pts',(-17.1467361911896,-14.4583495489556,
-1.48356266917816));
#23401=CARTESIAN_POINT('Ctrl Pts',(-17.2687582051385,-14.6825207434489,
-1.49456769840488));
#23402=CARTESIAN_POINT('Ctrl Pts',(-17.4170635504822,-15.1571942806963,
-1.51549662000442));
#23403=CARTESIAN_POINT('Ctrl Pts',(-17.4450135091226,-15.4022628476122,
-1.52469491979447));
#23404=CARTESIAN_POINT('Ctrl Pts',(-17.4071872139687,-15.9013115829333,
-1.54415175434035));
#23405=CARTESIAN_POINT('Ctrl Pts',(-17.3372890130251,-16.1502012038136,
-1.55495599988825));
#23406=CARTESIAN_POINT('Ctrl Pts',(-17.1073436483912,-16.6008033545264,
-1.57674641747953));
#23407=CARTESIAN_POINT('Ctrl Pts',(-16.9516283692376,-16.7992722722736,
-1.58751800921948));
#23408=CARTESIAN_POINT('Ctrl Pts',(-16.5754069871356,-17.1240092467816,
-1.60776152996803));
#23409=CARTESIAN_POINT('Ctrl Pts',(-16.3591691893559,-17.2480659982536,
-1.61656750158718));
#23410=CARTESIAN_POINT('Ctrl Pts',(-15.8824275687686,-17.4111698385855,
-1.63713021736795));
#23411=CARTESIAN_POINT('Ctrl Pts',(-15.6253005633504,-17.4450216013441,
-1.64822056338276));
#23412=CARTESIAN_POINT('Ctrl Pts',(-15.1226120634958,-17.4108856794204,
-1.6699024143108));
#23413=CARTESIAN_POINT('Ctrl Pts',(-14.8815852150972,-17.3470216561184,
-1.68029833185843));
#23414=CARTESIAN_POINT('Ctrl Pts',(-14.4299734275499,-17.1287077735559,
-1.69977715315189));
#23415=CARTESIAN_POINT('Ctrl Pts',(-14.2249541814665,-16.9737451489754,
-1.70940670711442));
#23416=CARTESIAN_POINT('Ctrl Pts',(-13.8873840854283,-16.5939162203865,
-1.73087454027017));
#23417=CARTESIAN_POINT('Ctrl Pts',(-13.7578745391481,-16.3730298263104,
-1.74191834693414));
#23418=CARTESIAN_POINT('Ctrl Pts',(-13.6039590632987,-15.9295232152934,
-1.76180407097136));
#23419=CARTESIAN_POINT('Ctrl Pts',(-13.5679367061318,-15.7154111956131,
-1.77057869840067));
#23420=CARTESIAN_POINT('Ctrl Pts',(-13.5679367061318,-15.5000000000001,
-1.77862500000012));
#23421=CARTESIAN_POINT('Origin',(15.5,-15.5,11.20575));
#23422=CARTESIAN_POINT('Ctrl Pts',(15.5000000000001,-13.5679367061317,-1.30987500000019));
#23423=CARTESIAN_POINT('Ctrl Pts',(15.5762794463024,-13.5679367061317,-1.30702571712498));
#23424=CARTESIAN_POINT('Ctrl Pts',(15.6526398620174,-13.5724537785089,-1.30407599509039));
#23425=CARTESIAN_POINT('Ctrl Pts',(15.9751450143044,-13.6108964642079,-1.29120033868165));
#23426=CARTESIAN_POINT('Ctrl Pts',(16.2136336424653,-13.6874920713324,-1.28064016816167));
#23427=CARTESIAN_POINT('Ctrl Pts',(16.657201722608,-13.9314508386658,-1.2588102842329));
#23428=CARTESIAN_POINT('Ctrl Pts',(16.8561400321273,-14.0998704991224,-1.24774717789506));
#23429=CARTESIAN_POINT('Ctrl Pts',(17.1682578349242,-14.4949992037636,-1.2275672705735));
#23430=CARTESIAN_POINT('Ctrl Pts',(17.28230159237,-14.7148147242691,-1.2187414403588));
#23431=CARTESIAN_POINT('Ctrl Pts',(17.423622247576,-15.1908203591582,-1.19821046895292));
#23432=CARTESIAN_POINT('Ctrl Pts',(17.4474792441873,-15.4431561242087,-1.18732677767448));
#23433=CARTESIAN_POINT('Ctrl Pts',(17.3968415255676,-15.9476066067079,-1.16556892929462));
#23434=CARTESIAN_POINT('Ctrl Pts',(17.3209404210904,-16.1946658536924,-1.15491282364457));
#23435=CARTESIAN_POINT('Ctrl Pts',(17.0825888205032,-16.6349759923567,-1.13592146261006));
#23436=CARTESIAN_POINT('Ctrl Pts',(16.9262354938101,-16.826141047329,-1.12621674018233));
#23437=CARTESIAN_POINT('Ctrl Pts',(16.5433162646621,-17.145874075694,-1.10501814661218));
#23438=CARTESIAN_POINT('Ctrl Pts',(16.3180913830553,-17.2686545572977,-1.09395740174894));
#23439=CARTESIAN_POINT('Ctrl Pts',(15.8338668009495,-17.4197688669732,-1.07261114005862));
#23440=CARTESIAN_POINT('Ctrl Pts',(15.579712564925,-17.4469489334786,-1.06317354299105));
#23441=CARTESIAN_POINT('Ctrl Pts',(15.0810498002778,-17.402261945606,-1.04358316874003));
#23442=CARTESIAN_POINT('Ctrl Pts',(14.8410934256464,-17.3330146958168,-1.03312664703881));
#23443=CARTESIAN_POINT('Ctrl Pts',(14.391695033367,-17.1033399709368,-1.01138703028757));
#23444=CARTESIAN_POINT('Ctrl Pts',(14.1882964703829,-16.9416955633752,-1.0003034334909));
#23445=CARTESIAN_POINT('Ctrl Pts',(13.863751146598,-16.5565376106627,-0.979874346404903));
#23446=CARTESIAN_POINT('Ctrl Pts',(13.7424917702376,-16.3394926778591,-0.971083815403324));
#23447=CARTESIAN_POINT('Ctrl Pts',(13.5868152063457,-15.8677779963454,-0.950737920464194));
#23448=CARTESIAN_POINT('Ctrl Pts',(13.5553093488703,-15.6170664355125,-0.939924284008434));
#23449=CARTESIAN_POINT('Ctrl Pts',(13.5900705720838,-15.1119904982328,-0.918139458649165));
#23450=CARTESIAN_POINT('Ctrl Pts',(13.6582150358001,-14.8626360597536,-0.907384357299283));
#23451=CARTESIAN_POINT('Ctrl Pts',(13.8825858943854,-14.4152869432226,-0.888089392603988));
#23452=CARTESIAN_POINT('Ctrl Pts',(14.0326711922679,-14.219530758934,-0.878736660945231));
#23453=CARTESIAN_POINT('Ctrl Pts',(14.4044393898322,-13.8885584189627,-0.857712208531138));
#23454=CARTESIAN_POINT('Ctrl Pts',(14.6248538454093,-13.7589900789026,-0.846684762349108));
#23455=CARTESIAN_POINT('Ctrl Pts',(15.0687257239408,-13.6042442375733,-0.826767486822827));
#23456=CARTESIAN_POINT('Ctrl Pts',(15.2837368797498,-13.5679367061317,-0.817953123727326));
#23457=CARTESIAN_POINT('Ctrl Pts',(15.5000000000001,-13.5679367061317,-0.809875000000185));
#23458=CARTESIAN_POINT('Ctrl Pts',(15.4999999999999,-13.5679367061317,-1.27862500000015));
#23459=CARTESIAN_POINT('Ctrl Pts',(15.4323298281631,-13.5679367061317,-1.28115269875943));
#23460=CARTESIAN_POINT('Ctrl Pts',(15.364588444747,-13.5714917240132,-1.28375972462899));
#23461=CARTESIAN_POINT('Ctrl Pts',(15.0424237119866,-13.6055206307448,-1.29652747819584));
#23462=CARTESIAN_POINT('Ctrl Pts',(14.795682631349,-13.6827641822509,-1.30740987787979));
#23463=CARTESIAN_POINT('Ctrl Pts',(14.3526857723723,-13.9256313091094,-1.32919488265952));
#23464=CARTESIAN_POINT('Ctrl Pts',(14.1593885176923,-14.0865851620145,-1.33988627064674));
#23465=CARTESIAN_POINT('Ctrl Pts',(13.8450923877406,-14.4724436680476,-1.35994762540591));
#23466=CARTESIAN_POINT('Ctrl Pts',(13.7268197745649,-14.6935102307068,-1.36883965886362));
#23467=CARTESIAN_POINT('Ctrl Pts',(13.5782346237301,-15.175601308443,-1.38963310626542));
#23468=CARTESIAN_POINT('Ctrl Pts',(13.5522076197147,-15.4328247704935,-1.4007276126267));
#23469=CARTESIAN_POINT('Ctrl Pts',(13.6009921105901,-15.9328184700475,-1.42229323201492));
#23470=CARTESIAN_POINT('Ctrl Pts',(13.6715975459788,-16.1712147180183,-1.43257568707766));
#23471=CARTESIAN_POINT('Ctrl Pts',(13.9035318487812,-16.618156863117,-1.45185309836975));
#23472=CARTESIAN_POINT('Ctrl Pts',(14.0663572618374,-16.8204876396432,-1.46188465462152));
#23473=CARTESIAN_POINT('Ctrl Pts',(14.4583495485159,-17.1467361909125,-1.48356266915572));
#23474=CARTESIAN_POINT('Ctrl Pts',(14.6825207429828,-17.268758204924,-1.49456769838278));
#23475=CARTESIAN_POINT('Ctrl Pts',(15.1571942801975,-17.4170635503929,-1.51549661998378));
#23476=CARTESIAN_POINT('Ctrl Pts',(15.4022628471055,-17.445013509097,-1.524694919776));
#23477=CARTESIAN_POINT('Ctrl Pts',(15.9013115824355,-17.4071872140733,-1.5441517543194));
#23478=CARTESIAN_POINT('Ctrl Pts',(16.1502012033337,-17.3372890131948,-1.55495599986658));
#23479=CARTESIAN_POINT('Ctrl Pts',(16.6008033541118,-17.1073436486759,-1.57674641745783));
#23480=CARTESIAN_POINT('Ctrl Pts',(16.7992722719041,-16.9516283695692,-1.58751800919846));
#23481=CARTESIAN_POINT('Ctrl Pts',(17.1240092465038,-16.5754069875524,-1.60776152994859));
#23482=CARTESIAN_POINT('Ctrl Pts',(17.2480659980264,-16.3591691898146,-1.6165675015673));
#23483=CARTESIAN_POINT('Ctrl Pts',(17.411169838485,-15.8824275692749,-1.63713021734601));
#23484=CARTESIAN_POINT('Ctrl Pts',(17.4450216013122,-15.6253005638585,-1.64822056336075));
#23485=CARTESIAN_POINT('Ctrl Pts',(17.4108856795171,-15.1226120639822,-1.66990241428974));
#23486=CARTESIAN_POINT('Ctrl Pts',(17.3470216562745,-14.8815852155614,-1.68029833183834));
#23487=CARTESIAN_POINT('Ctrl Pts',(17.1287077738309,-14.4299734279737,-1.69977715313357));
#23488=CARTESIAN_POINT('Ctrl Pts',(16.9737451493181,-14.2249541818671,-1.70940670709295));
#23489=CARTESIAN_POINT('Ctrl Pts',(16.5939162208352,-13.8873840857317,-1.73087454024684));
#23490=CARTESIAN_POINT('Ctrl Pts',(16.3730298267886,-13.7578745393868,-1.74191834691109));
#23491=CARTESIAN_POINT('Ctrl Pts',(15.9295232156415,-13.6039590633578,-1.76180407095704));
#23492=CARTESIAN_POINT('Ctrl Pts',(15.7154111957893,-13.5679367061317,-1.77057869839411));
#23493=CARTESIAN_POINT('Ctrl Pts',(15.5,-13.5679367061317,-1.77862500000015));
#23494=CARTESIAN_POINT('Origin',(15.4999999999998,15.5000000000002,11.20575));
#23495=CARTESIAN_POINT('Ctrl Pts',(13.5679367061316,15.5000000000003,-1.30987500000013));
#23496=CARTESIAN_POINT('Ctrl Pts',(13.5679367061316,15.5762794463024,-1.30702571712493));
#23497=CARTESIAN_POINT('Ctrl Pts',(13.5724537785087,15.6526398620172,-1.30407599509038));
#23498=CARTESIAN_POINT('Ctrl Pts',(13.6108964642076,15.975145014304,-1.29120033868164));
#23499=CARTESIAN_POINT('Ctrl Pts',(13.6874920713321,16.213633642465,-1.28064016816168));
#23500=CARTESIAN_POINT('Ctrl Pts',(13.9314508386654,16.6572017226077,-1.25881028423292));
#23501=CARTESIAN_POINT('Ctrl Pts',(14.0998704991219,16.856140032127,-1.24774717789509));
#23502=CARTESIAN_POINT('Ctrl Pts',(14.494999203763,17.168257834924,-1.22756727057352));
#23503=CARTESIAN_POINT('Ctrl Pts',(14.7148147242685,17.2823015923699,-1.21874144035882));
#23504=CARTESIAN_POINT('Ctrl Pts',(15.1908203591575,17.4236222475761,-1.19821046895294));
#23505=CARTESIAN_POINT('Ctrl Pts',(15.4431561242079,17.4474792441874,-1.18732677767449));
#23506=CARTESIAN_POINT('Ctrl Pts',(15.9476066067072,17.3968415255678,-1.16556892929464));
#23507=CARTESIAN_POINT('Ctrl Pts',(16.1946658536917,17.3209404210907,-1.1549128236446));
#23508=CARTESIAN_POINT('Ctrl Pts',(16.634975992356,17.0825888205037,-1.13592146261013));
#23509=CARTESIAN_POINT('Ctrl Pts',(16.8261410473284,16.9262354938106,-1.1262167401824));
#23510=CARTESIAN_POINT('Ctrl Pts',(17.1458740756934,16.5433162646627,-1.10501814661226));
#23511=CARTESIAN_POINT('Ctrl Pts',(17.2686545572972,16.318091383056,-1.09395740174901));
#23512=CARTESIAN_POINT('Ctrl Pts',(17.4197688669728,15.8338668009502,-1.07261114005869));
#23513=CARTESIAN_POINT('Ctrl Pts',(17.4469489334783,15.5797125649257,-1.0631735429911));
#23514=CARTESIAN_POINT('Ctrl Pts',(17.4022619456059,15.0810498002784,-1.04358316874009));
#23515=CARTESIAN_POINT('Ctrl Pts',(17.3330146958167,14.8410934256471,-1.03312664703889));
#23516=CARTESIAN_POINT('Ctrl Pts',(17.1033399709367,14.3916950333675,-1.01138703028766));
#23517=CARTESIAN_POINT('Ctrl Pts',(16.9416955633752,14.1882964703834,-1.00030343349101));
#23518=CARTESIAN_POINT('Ctrl Pts',(16.5565376106628,13.8637511465985,-0.979874346405002));
#23519=CARTESIAN_POINT('Ctrl Pts',(16.3394926778592,13.742491770238,-0.971083815403412));
#23520=CARTESIAN_POINT('Ctrl Pts',(15.8677779963456,13.5868152063461,-0.950737920464266));
#23521=CARTESIAN_POINT('Ctrl Pts',(15.6170664355127,13.5553093488706,-0.939924284008494));
#23522=CARTESIAN_POINT('Ctrl Pts',(15.111990498233,13.590070572084,-0.918139458649215));
#23523=CARTESIAN_POINT('Ctrl Pts',(14.8626360597538,13.6582150358002,-0.907384357299333));
#23524=CARTESIAN_POINT('Ctrl Pts',(14.4152869432227,13.8825858943855,-0.888089392604046));
#23525=CARTESIAN_POINT('Ctrl Pts',(14.2195307589341,14.0326711922679,-0.878736660945288));
#23526=CARTESIAN_POINT('Ctrl Pts',(13.8885584189627,14.4044393898322,-0.857712208531179));
#23527=CARTESIAN_POINT('Ctrl Pts',(13.7589900789026,14.6248538454092,-0.846684762349132));
#23528=CARTESIAN_POINT('Ctrl Pts',(13.6042442375732,15.0687257239408,-0.826767486822827));
#23529=CARTESIAN_POINT('Ctrl Pts',(13.5679367061315,15.2837368797499,-0.817953123727281));
#23530=CARTESIAN_POINT('Ctrl Pts',(13.5679367061315,15.5000000000003,-0.809875000000128));
#23531=CARTESIAN_POINT('Ctrl Pts',(13.5679367061315,15.5000000000001,-1.2786250000002));
#23532=CARTESIAN_POINT('Ctrl Pts',(13.5679367061315,15.4323298280958,-1.281152698762));
#23533=CARTESIAN_POINT('Ctrl Pts',(13.57149172402,15.364588444612,-1.28375972463429));
#23534=CARTESIAN_POINT('Ctrl Pts',(13.6055206307927,15.0424237117876,-1.2965274782044));
#23535=CARTESIAN_POINT('Ctrl Pts',(13.6827641823248,14.7956826311579,-1.30740987788859));
#23536=CARTESIAN_POINT('Ctrl Pts',(13.9256313092287,14.3526857722089,-1.32919488266825));
#23537=CARTESIAN_POINT('Ctrl Pts',(14.0865851621521,14.1593885175476,-1.33988627065515));
#23538=CARTESIAN_POINT('Ctrl Pts',(14.4724436682193,13.8450923876331,-1.35994762541367));
#23539=CARTESIAN_POINT('Ctrl Pts',(14.6935102308959,13.7268197744781,-1.36883965887183));
#23540=CARTESIAN_POINT('Ctrl Pts',(15.1756013086511,13.5782346236955,-1.38963310627446));
#23541=CARTESIAN_POINT('Ctrl Pts',(15.4328247707015,13.552207619708,-1.40072761263572));
#23542=CARTESIAN_POINT('Ctrl Pts',(15.932818470245,13.6009921106356,-1.42229323202347));
#23543=CARTESIAN_POINT('Ctrl Pts',(16.1712147182061,13.6715975460483,-1.43257568708578));
#23544=CARTESIAN_POINT('Ctrl Pts',(16.6181568632879,13.9035318488995,-1.45185309837713));
#23545=CARTESIAN_POINT('Ctrl Pts',(16.8204876398043,14.0663572619843,-1.46188465463047));
#23546=CARTESIAN_POINT('Ctrl Pts',(17.1467361910322,14.4583495487063,-1.48356266916542));
#23547=CARTESIAN_POINT('Ctrl Pts',(17.2687582050167,14.6825207431847,-1.49456769839234));
#23548=CARTESIAN_POINT('Ctrl Pts',(17.4170635504314,15.1571942804135,-1.51549661999271));
#23549=CARTESIAN_POINT('Ctrl Pts',(17.4450135091079,15.402262847325,-1.524694919784));
#23550=CARTESIAN_POINT('Ctrl Pts',(17.4071872140279,15.9013115826512,-1.54415175432848));
#23551=CARTESIAN_POINT('Ctrl Pts',(17.3372890131212,16.1502012035416,-1.55495599987596));
#23552=CARTESIAN_POINT('Ctrl Pts',(17.1073436485524,16.6008033542915,-1.57674641746723));
#23553=CARTESIAN_POINT('Ctrl Pts',(16.9516283694255,16.7992722720642,-1.58751800920757));
#23554=CARTESIAN_POINT('Ctrl Pts',(16.5754069873718,17.1240092466243,-1.60776152995703));
#23555=CARTESIAN_POINT('Ctrl Pts',(16.3591691896159,17.248065998125,-1.61656750157594));
#23556=CARTESIAN_POINT('Ctrl Pts',(15.8824275690554,17.4111698385287,-1.63713021735557));
#23557=CARTESIAN_POINT('Ctrl Pts',(15.6253005636383,17.4450216013262,-1.64822056337034));
#23558=CARTESIAN_POINT('Ctrl Pts',(15.1226120637714,17.4108856794754,-1.66990241429892));
#23559=CARTESIAN_POINT('Ctrl Pts',(14.8815852153602,17.3470216562071,-1.68029833184711));
#23560=CARTESIAN_POINT('Ctrl Pts',(14.42997342779,17.1287077737121,-1.69977715314157));
#23561=CARTESIAN_POINT('Ctrl Pts',(14.2249541816935,16.97374514917,-1.70940670710231));
#23562=CARTESIAN_POINT('Ctrl Pts',(13.8873840856002,16.5939162206412,-1.73087454025701));
#23563=CARTESIAN_POINT('Ctrl Pts',(13.7578745392833,16.3730298265818,-1.74191834692115));
#23564=CARTESIAN_POINT('Ctrl Pts',(13.603959063332,15.9295232154911,-1.76180407096332));
#23565=CARTESIAN_POINT('Ctrl Pts',(13.5679367061315,15.7154111957132,-1.77057869839701));
#23566=CARTESIAN_POINT('Ctrl Pts',(13.5679367061315,15.5000000000002,-1.7786250000002));
#23567=CARTESIAN_POINT('Origin',(-15.5,15.5,11.20575));
#23568=CARTESIAN_POINT('Ctrl Pts',(-15.5000000000001,13.5679367061317,-1.30987500000019));
#23569=CARTESIAN_POINT('Ctrl Pts',(-15.5762794463024,13.5679367061317,-1.30702571712498));
#23570=CARTESIAN_POINT('Ctrl Pts',(-15.6526398620174,13.5724537785089,-1.30407599509039));
#23571=CARTESIAN_POINT('Ctrl Pts',(-15.9751450143044,13.6108964642079,-1.29120033868165));
#23572=CARTESIAN_POINT('Ctrl Pts',(-16.2136336424653,13.6874920713324,-1.28064016816167));
#23573=CARTESIAN_POINT('Ctrl Pts',(-16.657201722608,13.9314508386658,-1.2588102842329));
#23574=CARTESIAN_POINT('Ctrl Pts',(-16.8561400321273,14.0998704991224,-1.24774717789506));
#23575=CARTESIAN_POINT('Ctrl Pts',(-17.1682578349242,14.4949992037636,-1.2275672705735));
#23576=CARTESIAN_POINT('Ctrl Pts',(-17.28230159237,14.7148147242692,-1.2187414403588));
#23577=CARTESIAN_POINT('Ctrl Pts',(-17.423622247576,15.1908203591582,-1.19821046895292));
#23578=CARTESIAN_POINT('Ctrl Pts',(-17.4474792441873,15.4431561242087,-1.18732677767448));
#23579=CARTESIAN_POINT('Ctrl Pts',(-17.3968415255676,15.9476066067079,-1.16556892929462));
#23580=CARTESIAN_POINT('Ctrl Pts',(-17.3209404210904,16.1946658536924,-1.15491282364457));
#23581=CARTESIAN_POINT('Ctrl Pts',(-17.0825888205032,16.6349759923567,-1.13592146261006));
#23582=CARTESIAN_POINT('Ctrl Pts',(-16.9262354938101,16.826141047329,-1.12621674018233));
#23583=CARTESIAN_POINT('Ctrl Pts',(-16.5433162646621,17.145874075694,-1.10501814661218));
#23584=CARTESIAN_POINT('Ctrl Pts',(-16.3180913830553,17.2686545572977,-1.09395740174894));
#23585=CARTESIAN_POINT('Ctrl Pts',(-15.8338668009495,17.4197688669732,-1.07261114005862));
#23586=CARTESIAN_POINT('Ctrl Pts',(-15.579712564925,17.4469489334786,-1.06317354299105));
#23587=CARTESIAN_POINT('Ctrl Pts',(-15.0810498002778,17.402261945606,-1.04358316874003));
#23588=CARTESIAN_POINT('Ctrl Pts',(-14.8410934256464,17.3330146958168,-1.03312664703881));
#23589=CARTESIAN_POINT('Ctrl Pts',(-14.391695033367,17.1033399709368,-1.01138703028757));
#23590=CARTESIAN_POINT('Ctrl Pts',(-14.1882964703828,16.9416955633752,-1.0003034334909));
#23591=CARTESIAN_POINT('Ctrl Pts',(-13.863751146598,16.5565376106627,-0.979874346404903));
#23592=CARTESIAN_POINT('Ctrl Pts',(-13.7424917702376,16.3394926778591,-0.971083815403324));
#23593=CARTESIAN_POINT('Ctrl Pts',(-13.5868152063457,15.8677779963454,-0.950737920464194));
#23594=CARTESIAN_POINT('Ctrl Pts',(-13.5553093488703,15.6170664355125,-0.939924284008433));
#23595=CARTESIAN_POINT('Ctrl Pts',(-13.5900705720838,15.1119904982328,-0.918139458649165));
#23596=CARTESIAN_POINT('Ctrl Pts',(-13.6582150358001,14.8626360597536,-0.907384357299283));
#23597=CARTESIAN_POINT('Ctrl Pts',(-13.8825858943854,14.4152869432226,-0.888089392603988));
#23598=CARTESIAN_POINT('Ctrl Pts',(-14.0326711922679,14.219530758934,-0.878736660945231));
#23599=CARTESIAN_POINT('Ctrl Pts',(-14.4044393898322,13.8885584189627,-0.857712208531138));
#23600=CARTESIAN_POINT('Ctrl Pts',(-14.6248538454093,13.7589900789026,-0.846684762349108));
#23601=CARTESIAN_POINT('Ctrl Pts',(-15.0687257239408,13.6042442375733,-0.826767486822827));
#23602=CARTESIAN_POINT('Ctrl Pts',(-15.2837368797498,13.5679367061317,-0.817953123727327));
#23603=CARTESIAN_POINT('Ctrl Pts',(-15.5000000000001,13.5679367061317,-0.809875000000185));
#23604=CARTESIAN_POINT('Ctrl Pts',(-15.4999999999999,13.5679367061317,-1.27862500000015));
#23605=CARTESIAN_POINT('Ctrl Pts',(-15.4323298281631,13.5679367061317,-1.28115269875943));
#23606=CARTESIAN_POINT('Ctrl Pts',(-15.364588444747,13.5714917240132,-1.28375972462899));
#23607=CARTESIAN_POINT('Ctrl Pts',(-15.0424237119866,13.6055206307448,-1.29652747819584));
#23608=CARTESIAN_POINT('Ctrl Pts',(-14.795682631349,13.6827641822509,-1.30740987787979));
#23609=CARTESIAN_POINT('Ctrl Pts',(-14.3526857723723,13.9256313091094,-1.32919488265952));
#23610=CARTESIAN_POINT('Ctrl Pts',(-14.1593885176923,14.0865851620145,-1.33988627064674));
#23611=CARTESIAN_POINT('Ctrl Pts',(-13.8450923877406,14.4724436680476,-1.35994762540591));
#23612=CARTESIAN_POINT('Ctrl Pts',(-13.7268197745649,14.6935102307068,-1.36883965886362));
#23613=CARTESIAN_POINT('Ctrl Pts',(-13.5782346237301,15.175601308443,-1.38963310626542));
#23614=CARTESIAN_POINT('Ctrl Pts',(-13.5522076197147,15.4328247704935,-1.4007276126267));
#23615=CARTESIAN_POINT('Ctrl Pts',(-13.6009921105901,15.9328184700475,-1.42229323201492));
#23616=CARTESIAN_POINT('Ctrl Pts',(-13.6715975459788,16.1712147180183,-1.43257568707766));
#23617=CARTESIAN_POINT('Ctrl Pts',(-13.9035318487812,16.618156863117,-1.45185309836975));
#23618=CARTESIAN_POINT('Ctrl Pts',(-14.0663572618374,16.8204876396432,-1.46188465462152));
#23619=CARTESIAN_POINT('Ctrl Pts',(-14.4583495485159,17.1467361909125,-1.48356266915572));
#23620=CARTESIAN_POINT('Ctrl Pts',(-14.6825207429828,17.268758204924,-1.49456769838278));
#23621=CARTESIAN_POINT('Ctrl Pts',(-15.1571942801975,17.4170635503929,-1.51549661998378));
#23622=CARTESIAN_POINT('Ctrl Pts',(-15.4022628471055,17.445013509097,-1.524694919776));
#23623=CARTESIAN_POINT('Ctrl Pts',(-15.9013115824355,17.4071872140733,-1.5441517543194));
#23624=CARTESIAN_POINT('Ctrl Pts',(-16.1502012033337,17.3372890131948,-1.55495599986658));
#23625=CARTESIAN_POINT('Ctrl Pts',(-16.6008033541118,17.1073436486759,-1.57674641745783));
#23626=CARTESIAN_POINT('Ctrl Pts',(-16.7992722719041,16.9516283695692,-1.58751800919846));
#23627=CARTESIAN_POINT('Ctrl Pts',(-17.1240092465038,16.5754069875524,-1.60776152994859));
#23628=CARTESIAN_POINT('Ctrl Pts',(-17.2480659980264,16.3591691898146,-1.6165675015673));
#23629=CARTESIAN_POINT('Ctrl Pts',(-17.411169838485,15.8824275692749,-1.63713021734601));
#23630=CARTESIAN_POINT('Ctrl Pts',(-17.4450216013122,15.6253005638585,-1.64822056336075));
#23631=CARTESIAN_POINT('Ctrl Pts',(-17.4108856795171,15.1226120639822,-1.66990241428974));
#23632=CARTESIAN_POINT('Ctrl Pts',(-17.3470216562745,14.8815852155614,-1.68029833183834));
#23633=CARTESIAN_POINT('Ctrl Pts',(-17.1287077738309,14.4299734279737,-1.69977715313357));
#23634=CARTESIAN_POINT('Ctrl Pts',(-16.9737451493181,14.2249541818671,-1.70940670709295));
#23635=CARTESIAN_POINT('Ctrl Pts',(-16.5939162208352,13.8873840857317,-1.73087454024684));
#23636=CARTESIAN_POINT('Ctrl Pts',(-16.3730298267886,13.7578745393868,-1.74191834691109));
#23637=CARTESIAN_POINT('Ctrl Pts',(-15.9295232156415,13.6039590633578,-1.76180407095704));
#23638=CARTESIAN_POINT('Ctrl Pts',(-15.7154111957893,13.5679367061317,-1.77057869839411));
#23639=CARTESIAN_POINT('Ctrl Pts',(-15.5,13.5679367061317,-1.77862500000015));
#23640=CARTESIAN_POINT('Origin',(-15.5,15.5,-1.713));
#23641=CARTESIAN_POINT('',(-17.32565468021,16.0440680000031,1.3858));
#23642=CARTESIAN_POINT('Ctrl Pts',(-17.405,15.5,1.86199999999989));
#23643=CARTESIAN_POINT('Ctrl Pts',(-17.405,15.4320300859014,1.85902668792209));
#23644=CARTESIAN_POINT('Ctrl Pts',(-17.4013623773891,15.3639795867244,1.85604985068775));
#23645=CARTESIAN_POINT('Ctrl Pts',(-17.3680903519982,15.0548487108932,1.84252706521832));
#23646=CARTESIAN_POINT('Ctrl Pts',(-17.2962463427199,14.8207041548242,1.8322845212083));
#23647=CARTESIAN_POINT('Ctrl Pts',(-17.0629990902563,14.3816006382695,1.81307614340625));
#23648=CARTESIAN_POINT('Ctrl Pts',(-16.8997756224006,14.1830144823051,1.80289013515953));
#23649=CARTESIAN_POINT('Ctrl Pts',(-16.5091900816921,13.8652038277476,1.7811420018313));
#23650=CARTESIAN_POINT('Ctrl Pts',(-16.2871007630363,13.7474308444605,1.77015243562359));
#23651=CARTESIAN_POINT('Ctrl Pts',(-15.8177448508294,13.6062726464789,1.74928396482839));
#23652=CARTESIAN_POINT('Ctrl Pts',(-15.5757787768183,13.5813005437059,1.74017043193075));
#23653=CARTESIAN_POINT('Ctrl Pts',(-15.0840796797206,13.6238960707691,1.72061130364396));
#23654=CARTESIAN_POINT('Ctrl Pts',(-14.8394161266748,13.6954601884097,1.70977723054079));
#23655=CARTESIAN_POINT('Ctrl Pts',(-14.3978031730946,13.9268566861076,1.68798605445638));
#23656=CARTESIAN_POINT('Ctrl Pts',(-14.2039509059274,14.082295157107,1.67724238763888));
#23657=CARTESIAN_POINT('Ctrl Pts',(-13.8874957229304,14.4567250042913,1.65706420954498));
#23658=CARTESIAN_POINT('Ctrl Pts',(-13.7672449283597,14.67165607392,1.64823551732623));
#23659=CARTESIAN_POINT('Ctrl Pts',(-13.6116074571869,15.1436631098165,1.62758779047162));
#23660=CARTESIAN_POINT('Ctrl Pts',(-13.5810328132329,15.3972548412816,1.61649453887646));
#23661=CARTESIAN_POINT('Ctrl Pts',(-13.6199507818047,15.8919955927732,1.59485233627403));
#23662=CARTESIAN_POINT('Ctrl Pts',(-13.6853476751625,16.1287315281175,1.58449643359055));
#23663=CARTESIAN_POINT('Ctrl Pts',(-13.9054834861942,16.572367937139,1.56508976652923));
#23664=CARTESIAN_POINT('Ctrl Pts',(-14.0610698096642,16.7735622211342,1.55532322784484));
#23665=CARTESIAN_POINT('Ctrl Pts',(-14.4399397318407,17.1023987051858,1.53377776768035));
#23666=CARTESIAN_POINT('Ctrl Pts',(-14.6589383366756,17.2274330903607,1.52274646637818));
#23667=CARTESIAN_POINT('Ctrl Pts',(-15.124472454443,17.3831189075426,1.50170502801835));
#23668=CARTESIAN_POINT('Ctrl Pts',(-15.3655432554421,17.4154773378446,1.49232290574879));
#23669=CARTESIAN_POINT('Ctrl Pts',(-15.8582468171056,17.3879615174967,1.47305555180698));
#23670=CARTESIAN_POINT('Ctrl Pts',(-16.1049540011558,17.3239372389492,1.46230897140638));
#23671=CARTESIAN_POINT('Ctrl Pts',(-16.5540792357571,17.10589348966,1.44052525586438));
#23672=CARTESIAN_POINT('Ctrl Pts',(-16.7531192799618,16.9559118142615,1.42970440842995));
#23673=CARTESIAN_POINT('Ctrl Pts',(-17.0114997971817,16.6679033966798,1.41361655626258));
#23674=CARTESIAN_POINT('Ctrl Pts',(-17.0932012813456,16.5537180410099,1.40809440249374));
#23675=CARTESIAN_POINT('Ctrl Pts',(-17.2304684005269,16.3088931485296,1.39738465216653));
#23676=CARTESIAN_POINT('Ctrl Pts',(-17.2854690953382,16.1789132787142,1.39169874360068));
#23677=CARTESIAN_POINT('Ctrl Pts',(-17.32565468021,16.0440680000031,1.38580000000002));
#23678=CARTESIAN_POINT('',(-16.3931641176038,17.1826416311934,1.3858));
#23679=CARTESIAN_POINT('Origin',(-15.5,15.5,1.3858));
#23680=CARTESIAN_POINT('Ctrl Pts',(-16.3931641176044,17.182641631193,1.38579999999996));
#23681=CARTESIAN_POINT('Ctrl Pts',(-16.2723883324171,17.2467507056418,1.3917776655887));
#23682=CARTESIAN_POINT('Ctrl Pts',(-16.1450664179259,17.2976688253463,1.3977148078573));
#23683=CARTESIAN_POINT('Ctrl Pts',(-15.8851785600351,17.3703971986234,1.40915110154527));
#23684=CARTESIAN_POINT('Ctrl Pts',(-15.7535588097723,17.3927389340048,1.41462603221265));
#23685=CARTESIAN_POINT('Ctrl Pts',(-15.3801305916486,17.4164430131056,1.4292914024198));
#23686=CARTESIAN_POINT('Ctrl Pts',(-15.1388459584443,17.3859249483997,1.43859912950402));
#23687=CARTESIAN_POINT('Ctrl Pts',(-14.6723439861098,17.23386825394,1.45959785680879));
#23688=CARTESIAN_POINT('Ctrl Pts',(-14.4525515511058,17.110640943444,1.47061970665662));
#23689=CARTESIAN_POINT('Ctrl Pts',(-14.0707452475483,16.7845360897548,1.49221666138324));
#23690=CARTESIAN_POINT('Ctrl Pts',(-13.9132616040367,16.5839904470103,1.50208134527492));
#23691=CARTESIAN_POINT('Ctrl Pts',(-13.6898378009267,16.1414810943751,1.52143870978214));
#23692=CARTESIAN_POINT('Ctrl Pts',(-13.6228129384099,15.9053796762351,1.53176685580751));
#23693=CARTESIAN_POINT('Ctrl Pts',(-13.580357781213,15.4112880829908,1.55338066128627));
#23694=CARTESIAN_POINT('Ctrl Pts',(-13.6090431492827,15.1576722103972,1.56447496892379));
#23695=CARTESIAN_POINT('Ctrl Pts',(-13.7611758077611,14.6843730255031,1.58517922023149));
#23696=CARTESIAN_POINT('Ctrl Pts',(-13.8800302566413,14.4682765188114,1.59402873094833));
#23697=CARTESIAN_POINT('Ctrl Pts',(-14.1939644866156,14.0915194243571,1.61416230774197));
#23698=CARTESIAN_POINT('Ctrl Pts',(-14.3865682657467,13.9348153522307,1.62488635855805));
#23699=CARTESIAN_POINT('Ctrl Pts',(-14.8263458369783,13.7002975223377,1.64667627385321));
#23700=CARTESIAN_POINT('Ctrl Pts',(-15.0704913068452,13.6269593374867,1.65752952282736));
#23701=CARTESIAN_POINT('Ctrl Pts',(-15.5619293145468,13.5807968238314,1.67715677811531));
#23702=CARTESIAN_POINT('Ctrl Pts',(-15.804120411355,13.6040306004054,1.68621877962558));
#23703=CARTESIAN_POINT('Ctrl Pts',(-16.2743516095945,13.7417859609585,1.70704598188298));
#23704=CARTESIAN_POINT('Ctrl Pts',(-16.4971311158611,13.8578481105359,1.7180242752626));
#23705=CARTESIAN_POINT('Ctrl Pts',(-16.8882752695545,14.1713019326203,1.73969827721722));
#23706=CARTESIAN_POINT('Ctrl Pts',(-17.0518930224525,14.3667173602226,1.74992508137436));
#23707=CARTESIAN_POINT('Ctrl Pts',(-17.288707924895,14.8011847488145,1.76893065392868));
#23708=CARTESIAN_POINT('Ctrl Pts',(-17.3630339890476,15.0342747992455,1.77912706908314));
#23709=CARTESIAN_POINT('Ctrl Pts',(-17.4005657968241,15.3498262737769,1.79293072063744));
#23710=CARTESIAN_POINT('Ctrl Pts',(-17.405,15.4249560243541,1.79621723641079));
#23711=CARTESIAN_POINT('Ctrl Pts',(-17.405,15.5,1.79949999999985));
#23712=CARTESIAN_POINT('Origin',(15.5,15.5,-1.713));
#23713=CARTESIAN_POINT('',(16.0440680000052,17.3256546802097,1.3858));
#23714=CARTESIAN_POINT('Ctrl Pts',(13.595,15.5,1.73699999999994));
#23715=CARTESIAN_POINT('Ctrl Pts',(13.595,15.4699273628645,1.73586073194578));
#23716=CARTESIAN_POINT('Ctrl Pts',(13.5957120893792,15.4398306754848,1.73470497776689));
#23717=CARTESIAN_POINT('Ctrl Pts',(13.6090996130625,15.1576110183613,1.72372058781246));
#23718=CARTESIAN_POINT('Ctrl Pts',(13.6710479482893,14.9103855829078,1.71299977962444));
#23719=CARTESIAN_POINT('Ctrl Pts',(13.8853907466994,14.4592729280394,1.69122172108156));
#23720=CARTESIAN_POINT('Ctrl Pts',(14.0338479961768,14.258837749694,1.68038136320761));
#23721=CARTESIAN_POINT('Ctrl Pts',(14.3956899669362,13.9288953046006,1.65996756073088));
#23722=CARTESIAN_POINT('Ctrl Pts',(14.6044910974772,13.8011967843423,1.651173617783));
#23723=CARTESIAN_POINT('Ctrl Pts',(15.0694642475063,13.6269920348691,1.63083358497329));
#23724=CARTESIAN_POINT('Ctrl Pts',(15.3226988387298,13.5863464627192,1.61975595631083));
#23725=CARTESIAN_POINT('Ctrl Pts',(15.8204761748578,13.6063323454247,1.59798091973478));
#23726=CARTESIAN_POINT('Ctrl Pts',(16.0604000490661,13.6629773403858,1.58748556215787));
#23727=CARTESIAN_POINT('Ctrl Pts',(16.5099074456352,13.8656749614721,1.56782207149429));
#23728=CARTESIAN_POINT('Ctrl Pts',(16.7144958138179,14.0113953950104,1.55849700337696));
#23729=CARTESIAN_POINT('Ctrl Pts',(17.0574581079868,14.3747233338918,1.53723137030345));
#23730=CARTESIAN_POINT('Ctrl Pts',(17.1919121858965,14.589311632061,1.52616111848699));
#23731=CARTESIAN_POINT('Ctrl Pts',(17.3666878890906,15.049604046309,1.50490071710883));
#23732=CARTESIAN_POINT('Ctrl Pts',(17.4086874588649,15.2896536370031,1.49504938859915));
#23733=CARTESIAN_POINT('Ctrl Pts',(17.4006271908752,15.7834258159291,1.4761670883093));
#23734=CARTESIAN_POINT('Ctrl Pts',(17.3464078918416,16.0324150395295,1.46554851252527));
#23735=CARTESIAN_POINT('Ctrl Pts',(17.1459365086778,16.4906249151765,1.44380498303461));
#23736=CARTESIAN_POINT('Ctrl Pts',(17.0032377368195,16.6961304680377,1.43289849067567));
#23737=CARTESIAN_POINT('Ctrl Pts',(16.7155289154758,16.9747253572526,1.41605139259624));
#23738=CARTESIAN_POINT('Ctrl Pts',(16.5934948001371,17.0673550935378,1.40987305653158));
#23739=CARTESIAN_POINT('Ctrl Pts',(16.3302699480926,17.2212965079858,1.39828383511302));
#23740=CARTESIAN_POINT('Ctrl Pts',(16.1900656890046,17.2821455371494,1.3921866005688));
#23741=CARTESIAN_POINT('Ctrl Pts',(16.0440680000051,17.3256546802094,1.38580000000015));
#23742=CARTESIAN_POINT('',(17.1826416311923,16.393164117606,1.3858));
#23743=CARTESIAN_POINT('Origin',(15.5,15.5,1.3858));
#23744=CARTESIAN_POINT('Ctrl Pts',(17.1826416311919,16.3931641176066,1.38579999999991));
#23745=CARTESIAN_POINT('Ctrl Pts',(17.24665362517,16.2725712233782,1.39176861360038));
#23746=CARTESIAN_POINT('Ctrl Pts',(17.2975148512645,16.1454515121981,1.39769685123167));
#23747=CARTESIAN_POINT('Ctrl Pts',(17.3702201242742,15.8859713444243,1.40911719478266));
#23748=CARTESIAN_POINT('Ctrl Pts',(17.3925920222397,15.7545528306264,1.41458516155685));
#23749=CARTESIAN_POINT('Ctrl Pts',(17.4165176652001,15.3813317017817,1.42924753252314));
#23750=CARTESIAN_POINT('Ctrl Pts',(17.3861509933302,15.1400292056562,1.43854935939874));
#23751=CARTESIAN_POINT('Ctrl Pts',(17.234392581011,14.6734480786425,1.45954456128325));
#23752=CARTESIAN_POINT('Ctrl Pts',(17.1113140091714,14.4535910385712,1.47056560536997));
#23753=CARTESIAN_POINT('Ctrl Pts',(16.7854343398408,14.0715436685454,1.49216676733657));
#23754=CARTESIAN_POINT('Ctrl Pts',(16.5849420836776,13.9139037708014,1.50203971637447));
#23755=CARTESIAN_POINT('Ctrl Pts',(16.1425255215973,13.6902101009022,1.52139302180229));
#23756=CARTESIAN_POINT('Ctrl Pts',(15.906476643006,13.6230519475303,1.5317188695097));
#23757=CARTESIAN_POINT('Ctrl Pts',(15.4124393942654,13.5803069603505,1.55333029771356));
#23758=CARTESIAN_POINT('Ctrl Pts',(15.1588221439251,13.6088374167553,1.56442466561995));
#23759=CARTESIAN_POINT('Ctrl Pts',(14.6854174034196,13.7606823527963,1.58513353440842));
#23760=CARTESIAN_POINT('Ctrl Pts',(14.4692250920796,13.8794222936253,1.59398495150606));
#23761=CARTESIAN_POINT('Ctrl Pts',(14.0922776263441,14.1931499146905,1.61411486500468));
#23762=CARTESIAN_POINT('Ctrl Pts',(13.935470385775,14.3856511393828,1.62483728718873));
#23763=CARTESIAN_POINT('Ctrl Pts',(13.7006976935149,14.8252774899478,1.64662704807638));
#23764=CARTESIAN_POINT('Ctrl Pts',(13.6272144555416,15.0693799656232,1.65748184090438));
#23765=CARTESIAN_POINT('Ctrl Pts',(13.5978121805544,15.3804101463148,1.66990796405906));
#23766=CARTESIAN_POINT('Ctrl Pts',(13.595,15.440236933533,1.67223594340449));
#23767=CARTESIAN_POINT('Ctrl Pts',(13.595,15.4999999999999,1.67449999999978));
#23768=CARTESIAN_POINT('Origin',(15.5,-15.5,-1.713));
#23769=CARTESIAN_POINT('',(17.32565468021,-16.0440680000029,1.3858));
#23770=CARTESIAN_POINT('Ctrl Pts',(13.595,-15.5,1.61199999999989));
#23771=CARTESIAN_POINT('Ctrl Pts',(13.595,-15.536390811308,1.61040810099254));
#23772=CARTESIAN_POINT('Ctrl Pts',(13.5960427336748,-15.5728179794516,1.60881461157244));
#23773=CARTESIAN_POINT('Ctrl Pts',(13.6121171890736,-15.8526811699943,1.59657212729673));
#23774=CARTESIAN_POINT('Ctrl Pts',(13.6727140897741,-16.091211600863,1.58613772524647));
#23775=CARTESIAN_POINT('Ctrl Pts',(13.8832384335276,-16.538105979127,1.56658853984559));
#23776=CARTESIAN_POINT('Ctrl Pts',(14.033346321881,-16.7411793436505,1.55708178792549));
#23777=CARTESIAN_POINT('Ctrl Pts',(14.4036422324888,-17.0778758818557,1.53568922735653));
#23778=CARTESIAN_POINT('Ctrl Pts',(14.6202507282492,-17.208137086823,1.52463415025734));
#23779=CARTESIAN_POINT('Ctrl Pts',(15.0829186266929,-17.3743776635122,1.50347043888761));
#23780=CARTESIAN_POINT('Ctrl Pts',(15.3234036970219,-17.412073738625,1.49384487112439));
#23781=CARTESIAN_POINT('Ctrl Pts',(15.8167315474728,-17.3953646239746,1.47479023384486));
#23782=CARTESIAN_POINT('Ctrl Pts',(16.0647559828302,-17.3367775777424,1.46411267545049));
#23783=CARTESIAN_POINT('Ctrl Pts',(16.5190134240267,-17.1284495137126,1.44234703608263));
#23784=CARTESIAN_POINT('Ctrl Pts',(16.721677544645,-16.9824805684246,1.43147666208721));
#23785=CARTESIAN_POINT('Ctrl Pts',(16.9912576203034,-16.6944874199144,1.41496486120666));
#23786=CARTESIAN_POINT('Ctrl Pts',(17.0789552713108,-16.575884089482,1.40906404590897));
#23787=CARTESIAN_POINT('Ctrl Pts',(17.2254012201848,-16.3207782997712,1.39790456254455));
#23788=CARTESIAN_POINT('Ctrl Pts',(17.28362719674,-16.1850938862784,1.39196911138564));
#23789=CARTESIAN_POINT('Ctrl Pts',(17.3256546802103,-16.0440680000022,1.38579999999998));
#23790=CARTESIAN_POINT('',(16.3931641176036,-17.1826416311934,1.3858));
#23791=CARTESIAN_POINT('Origin',(15.5,-15.5,1.3858));
#23792=CARTESIAN_POINT('Ctrl Pts',(16.3931641176036,-17.1826416311935,1.3858));
#23793=CARTESIAN_POINT('Ctrl Pts',(16.2759070945517,-17.2448829091848,1.39160350829969));
#23794=CARTESIAN_POINT('Ctrl Pts',(16.1524707830423,-17.2946955088363,1.39736926863837));
#23795=CARTESIAN_POINT('Ctrl Pts',(15.9004262675809,-17.3669323901444,1.40849767607179));
#23796=CARTESIAN_POINT('Ctrl Pts',(15.7726845826618,-17.3898214067908,1.41383766087422));
#23797=CARTESIAN_POINT('Ctrl Pts',(15.4032482695823,-17.4177501133806,1.428444204422));
#23798=CARTESIAN_POINT('Ctrl Pts',(15.1616129530288,-17.3901425823975,1.43764437829329));
#23799=CARTESIAN_POINT('Ctrl Pts',(14.6936015261495,-17.2438130087807,1.45857502447647));
#23800=CARTESIAN_POINT('Ctrl Pts',(14.4725857350829,-17.1234469739703,1.46958063721079));
#23801=CARTESIAN_POINT('Ctrl Pts',(14.0861584798649,-16.8016835834113,1.49125769386053));
#23802=CARTESIAN_POINT('Ctrl Pts',(13.9256664401826,-16.6021652185474,1.50128629840102));
#23803=CARTESIAN_POINT('Ctrl Pts',(13.6970710454032,-16.1614416400184,1.52056554505583));
#23804=CARTESIAN_POINT('Ctrl Pts',(13.6275006434827,-15.9263591104517,1.53084912027747));
#23805=CARTESIAN_POINT('Ctrl Pts',(13.5979805133499,-15.6231241110188,1.54411399339352));
#23806=CARTESIAN_POINT('Ctrl Pts',(13.595,-15.561525211074,1.5468086084393));
#23807=CARTESIAN_POINT('Ctrl Pts',(13.595,-15.5,1.54949999999984));
#23808=CARTESIAN_POINT('Origin',(-15.5,-15.5,-1.713));
#23809=CARTESIAN_POINT('',(-16.0440680000367,-17.3256546802026,1.3858));
#23810=CARTESIAN_POINT('Ctrl Pts',(-17.405,-15.5,1.48699999999984));
#23811=CARTESIAN_POINT('Ctrl Pts',(-17.405,-15.5186265321859,1.48629435476548));
#23812=CARTESIAN_POINT('Ctrl Pts',(-17.4047268139491,-15.5372634348496,
1.48558234145932));
#23813=CARTESIAN_POINT('Ctrl Pts',(-17.3967729604905,-15.8081805965321,
1.47514498052024));
#23814=CARTESIAN_POINT('Ctrl Pts',(-17.3393068162074,-16.0564605136505,
1.46448226015211));
#23815=CARTESIAN_POINT('Ctrl Pts',(-17.1329906165269,-16.5117466633973,
1.44272165334931));
#23816=CARTESIAN_POINT('Ctrl Pts',(-16.9878569403636,-16.7151458811511,
1.43184170025367));
#23817=CARTESIAN_POINT('Ctrl Pts',(-16.699905912139,-16.9870454132385,1.41524295063963));
#23818=CARTESIAN_POINT('Ctrl Pts',(-16.5804094676046,-17.0759978712803,
1.40926200645678));
#23819=CARTESIAN_POINT('Ctrl Pts',(-16.3232094764869,-17.2243558857854,
1.39801091323203));
#23820=CARTESIAN_POINT('Ctrl Pts',(-16.1863597090227,-17.2832499656779,
1.3920244842091));
#23821=CARTESIAN_POINT('Ctrl Pts',(-16.0440680000359,-17.3256546802002,
1.38580000000145));
#23822=CARTESIAN_POINT('',(-17.1826416312037,-16.3931641175801,1.3858));
#23823=CARTESIAN_POINT('Origin',(-15.5,-15.5,1.3858));
#23824=CARTESIAN_POINT('Ctrl Pts',(-17.1826416312051,-16.3931641175817,
1.38580000000111));
#23825=CARTESIAN_POINT('Ctrl Pts',(-17.243819155217,-16.2779111122602,1.39150432163177));
#23826=CARTESIAN_POINT('Ctrl Pts',(-17.2929918586721,-16.1566832784271,
1.39717242029638));
#23827=CARTESIAN_POINT('Ctrl Pts',(-17.3649044547202,-15.9091049784493,
1.40812453732309));
#23828=CARTESIAN_POINT('Ctrl Pts',(-17.3880739083904,-15.783577621763,1.41338676858269));
#23829=CARTESIAN_POINT('Ctrl Pts',(-17.4028534332033,-15.6044814179587,
1.42049488864491));
#23830=CARTESIAN_POINT('Ctrl Pts',(-17.405,-15.5522133244187,1.42252195689568));
#23831=CARTESIAN_POINT('Ctrl Pts',(-17.405,-15.5000000000001,1.42449999999991));
#23832=CARTESIAN_POINT('Origin',(0.,0.,-37.019));
#23833=CARTESIAN_POINT('',(-2.62699999999999,-3.21714714136009E-16,1.3858));
#23834=CARTESIAN_POINT('Origin',(0.,0.,1.3858));
#23835=CARTESIAN_POINT('',(-2.62699999999999,-3.21714714136009E-16,6.669));
#23836=CARTESIAN_POINT('',(-2.62699999999999,-3.21714714136008E-16,-37.019));
#23837=CARTESIAN_POINT('Origin',(0.,0.,6.669));
#23838=CARTESIAN_POINT('Origin',(0.,0.,6.669));
#23839=CARTESIAN_POINT('',(-3.76999999999999,-4.61691843278552E-16,6.669));
#23840=CARTESIAN_POINT('Origin',(0.,0.,6.669));
#23841=CARTESIAN_POINT('',(-3.76999999999999,-4.61691843278552E-16,13.019));
#23842=CARTESIAN_POINT('',(-3.76999999999999,-4.61691843278551E-16,6.669));
#23843=CARTESIAN_POINT('Origin',(0.,0.,13.019));
#23844=CARTESIAN_POINT('Origin',(0.,0.,11.495));
#23845=CARTESIAN_POINT('',(11.493,-1.40748656626005E-15,10.987));
#23846=CARTESIAN_POINT('Origin',(0.,0.,10.987));
#23847=CARTESIAN_POINT('',(10.985,-1.34527450886337E-15,11.495));
#23848=CARTESIAN_POINT('',(10.985,-1.34527450886337E-15,11.495));
#23849=CARTESIAN_POINT('Origin',(0.,0.,11.495));
#23850=CARTESIAN_POINT('Origin',(0.,0.,13.019));
#23851=CARTESIAN_POINT('',(10.985,-1.34527450886337E-15,13.019));
#23852=CARTESIAN_POINT('',(10.985,-1.34527450886337E-15,13.019));
#23853=CARTESIAN_POINT('Origin',(0.,0.,13.019));
#23854=CARTESIAN_POINT('Origin',(-15.4999999999999,-15.5000000000001,10.987));
#23855=CARTESIAN_POINT('',(-15.499999994708,-17.1672595260839,10.4992595260838));
#23856=CARTESIAN_POINT('Ctrl Pts',(-13.5949999999992,-15.5000000000296,
10.7370000000007));
#23857=CARTESIAN_POINT('Ctrl Pts',(-13.6008497881007,-15.2564355648758,
10.7311502118955));
#23858=CARTESIAN_POINT('Ctrl Pts',(-13.650944651317,-15.0667953438396,10.7259167101349));
#23859=CARTESIAN_POINT('Ctrl Pts',(-13.7548661865755,-14.7648541062214,
10.7172082071437));
#23860=CARTESIAN_POINT('Ctrl Pts',(-13.8368618391017,-14.6050214267038,
10.7121852577521));
#23861=CARTESIAN_POINT('Ctrl Pts',(-14.073970488167,-14.2704423655218,10.7006604618175));
#23862=CARTESIAN_POINT('Ctrl Pts',(-14.2414766707786,-14.1080191324474,
10.6942562020715));
#23863=CARTESIAN_POINT('Ctrl Pts',(-14.6374778586095,-13.8453173047647,
10.681998762105));
#23864=CARTESIAN_POINT('Ctrl Pts',(-14.8639328565342,-13.7520840601426,
10.6760021091648));
#23865=CARTESIAN_POINT('Ctrl Pts',(-15.3364039021795,-13.6614771916233,
10.6624990364387));
#23866=CARTESIAN_POINT('Ctrl Pts',(-15.5758065143609,-13.6626363666899,
10.655582285966));
#23867=CARTESIAN_POINT('Ctrl Pts',(-16.062912999776,-13.7609513162477,10.6413472559504));
#23868=CARTESIAN_POINT('Ctrl Pts',(-16.2635040620812,-13.8578641877347,
10.6354098660481));
#23869=CARTESIAN_POINT('Ctrl Pts',(-16.6035611311394,-14.0672823720547,
10.6252403230972));
#23870=CARTESIAN_POINT('Ctrl Pts',(-16.7766690301586,-14.2283948798923,
10.6186368111943));
#23871=CARTESIAN_POINT('Ctrl Pts',(-17.0457728351311,-14.6023972130674,
10.6050799280797));
#23872=CARTESIAN_POINT('Ctrl Pts',(-17.1416118806701,-14.8099919664234,
10.5982690748888));
#23873=CARTESIAN_POINT('Ctrl Pts',(-17.2495576082356,-15.2485979049578,
10.5851458477462));
#23874=CARTESIAN_POINT('Ctrl Pts',(-17.2617643752449,-15.4776646621072,
10.5793320921415));
#23875=CARTESIAN_POINT('Ctrl Pts',(-17.1990672566599,-15.9104000162702,
10.567155287325));
#23876=CARTESIAN_POINT('Ctrl Pts',(-17.1306302329843,-16.1118828633918,
10.5608366679581));
#23877=CARTESIAN_POINT('Ctrl Pts',(-16.9166251729184,-16.4935678846234,
10.5474332016197));
#23878=CARTESIAN_POINT('Ctrl Pts',(-16.7678269425302,-16.6673647634593,
10.5404564545235));
#23879=CARTESIAN_POINT('Ctrl Pts',(-16.4380554775456,-16.9263243699996,
10.5282450923036));
#23880=CARTESIAN_POINT('Ctrl Pts',(-16.2402954425981,-17.0406955315939,
10.5224302623227));
#23881=CARTESIAN_POINT('Ctrl Pts',(-15.8342695060709,-17.1526817172524,
10.5098001955615));
#23882=CARTESIAN_POINT('Ctrl Pts',(-15.6670883208016,-17.1725541316431,
10.5045541305823));
#23883=CARTESIAN_POINT('Ctrl Pts',(-15.4999999894162,-17.1672595260839,
10.4992595260838));
#23884=CARTESIAN_POINT('',(-14.5577749122402,-14.2313898004749,10.4122404735808));
#23885=CARTESIAN_POINT('Ctrl Pts',(-14.5577749122402,-14.2313898004749,
10.4122404735809));
#23886=CARTESIAN_POINT('Ctrl Pts',(-14.3868051820039,-14.3303760686904,
10.4347161538326));
#23887=CARTESIAN_POINT('Ctrl Pts',(-14.235113371322,-14.4592007076174,10.4582727675319));
#23888=CARTESIAN_POINT('Ctrl Pts',(-13.98017849664,-14.7697452365794,10.5059067908485));
#23889=CARTESIAN_POINT('Ctrl Pts',(-13.8810021159392,-14.9504857681989,
10.5295757840843));
#23890=CARTESIAN_POINT('Ctrl Pts',(-13.7335179124492,-15.400735819956,10.5809089218014));
#23891=CARTESIAN_POINT('Ctrl Pts',(-13.7252310950464,-15.6393119361012,
10.6025326156877));
#23892=CARTESIAN_POINT('Ctrl Pts',(-13.7544578969404,-16.0071202507761,
10.6406359197722));
#23893=CARTESIAN_POINT('Ctrl Pts',(-13.7957662195545,-16.1857710732841,
10.6600613989279));
#23894=CARTESIAN_POINT('Ctrl Pts',(-13.9306559184097,-16.5282411322908,
10.6990893282686));
#23895=CARTESIAN_POINT('Ctrl Pts',(-14.0244109493983,-16.6897880532903,
10.7184707369832));
#23896=CARTESIAN_POINT('Ctrl Pts',(-14.1407339385554,-16.8346987578457,
10.7369999999972));
#23897=CARTESIAN_POINT('',(-13.9406917842496,-15.2436450846258,10.4122404735808));
#23898=CARTESIAN_POINT('Origin',(-15.5,-15.5000000000001,10.4122404735808));
#23899=CARTESIAN_POINT('Ctrl Pts',(-15.4999999894162,-17.1672595260839,
10.4992595260838));
#23900=CARTESIAN_POINT('Ctrl Pts',(-15.4589933982957,-17.1659601311859,
10.4979601314461));
#23901=CARTESIAN_POINT('Ctrl Pts',(-15.4179923936843,-17.1631450533092,
10.4966578716341));
#23902=CARTESIAN_POINT('Ctrl Pts',(-15.1578207074785,-17.1355603869698,
10.4883749005524));
#23903=CARTESIAN_POINT('Ctrl Pts',(-14.9453351143306,-17.0690262279152,
10.4815187112078));
#23904=CARTESIAN_POINT('Ctrl Pts',(-14.5384028688187,-16.8460543494088,
10.468240993816));
#23905=CARTESIAN_POINT('Ctrl Pts',(-14.384838579944,-16.7012184908713,10.4620910771073));
#23906=CARTESIAN_POINT('Ctrl Pts',(-14.1456891975424,-16.4090783981286,
10.4500509032653));
#23907=CARTESIAN_POINT('Ctrl Pts',(-14.046850578254,-16.2259194616222,10.4432455275598));
#23908=CARTESIAN_POINT('Ctrl Pts',(-13.9464878894178,-15.9056854194768,
10.4323954781049));
#23909=CARTESIAN_POINT('Ctrl Pts',(-13.9227846102421,-15.7780439261845,
10.4283074238932));
#23910=CARTESIAN_POINT('Ctrl Pts',(-13.9059874790046,-15.513966292252,10.4203309872474));
#23911=CARTESIAN_POINT('Ctrl Pts',(-13.914345653721,-15.3775884074119,10.4165086268911));
#23912=CARTESIAN_POINT('Ctrl Pts',(-13.94069178425,-15.2436450846239,10.4122404735808));
#23913=CARTESIAN_POINT('',(-15.4999999999999,-17.6550000000001,10.987));
#23914=CARTESIAN_POINT('',(-15.4999999999999,-17.6550000000001,10.987));
#23915=CARTESIAN_POINT('Origin',(-15.5,-15.5,10.987));
#23916=CARTESIAN_POINT('Origin',(15.5,-15.5,10.987));
#23917=CARTESIAN_POINT('',(17.1672595260838,-15.4999999947082,10.4992595260838));
#23918=CARTESIAN_POINT('Ctrl Pts',(15.5000000000296,-13.5949999999993,10.7370000000007));
#23919=CARTESIAN_POINT('Ctrl Pts',(15.2564355648662,-13.600849788101,10.7311502118952));
#23920=CARTESIAN_POINT('Ctrl Pts',(15.0667953438228,-13.6509446513211,10.7259167101345));
#23921=CARTESIAN_POINT('Ctrl Pts',(14.7648541061942,-13.7548661865872,10.7172082071429));
#23922=CARTESIAN_POINT('Ctrl Pts',(14.6050214266715,-13.8368618391195,10.712185257751));
#23923=CARTESIAN_POINT('Ctrl Pts',(14.27044236549,-14.0739704881962,10.7006604618163));
#23924=CARTESIAN_POINT('Ctrl Pts',(14.1080191324201,-14.2414766708108,10.6942562020704));
#23925=CARTESIAN_POINT('Ctrl Pts',(13.8453173047464,-14.6374778586467,10.681998762104));
#23926=CARTESIAN_POINT('Ctrl Pts',(13.7520840601298,-14.8639328565725,10.6760021091637));
#23927=CARTESIAN_POINT('Ctrl Pts',(13.661477191621,-15.336403902218,10.6624990364376));
#23928=CARTESIAN_POINT('Ctrl Pts',(13.6626363666926,-15.5758065143984,10.6555822859649));
#23929=CARTESIAN_POINT('Ctrl Pts',(13.7609513162606,-16.0629129998141,10.6413472559492));
#23930=CARTESIAN_POINT('Ctrl Pts',(13.8578641877541,-16.2635040621222,10.635409866047));
#23931=CARTESIAN_POINT('Ctrl Pts',(14.0672823720874,-16.6035611311796,10.6252403230958));
#23932=CARTESIAN_POINT('Ctrl Pts',(14.2283948799295,-16.7766690301937,10.6186368111928));
#23933=CARTESIAN_POINT('Ctrl Pts',(14.6023972131106,-17.0457728351544,10.6050799280782));
#23934=CARTESIAN_POINT('Ctrl Pts',(14.8099919664681,-17.1416118806874,10.5982690748874));
#23935=CARTESIAN_POINT('Ctrl Pts',(15.2485979050077,-17.2495576082419,10.5851458477448));
#23936=CARTESIAN_POINT('Ctrl Pts',(15.4776646621617,-17.2617643752449,10.57933209214));
#23937=CARTESIAN_POINT('Ctrl Pts',(15.9104000163284,-17.1990672566442,10.5671552873232));
#23938=CARTESIAN_POINT('Ctrl Pts',(16.1118828634489,-17.1306302329612,10.5608366679562));
#23939=CARTESIAN_POINT('Ctrl Pts',(16.4935678846754,-16.9166251728798,10.5474332016177));
#23940=CARTESIAN_POINT('Ctrl Pts',(16.667364763507,-16.767826942484,10.5404564545215));
#23941=CARTESIAN_POINT('Ctrl Pts',(16.9263243700374,-16.4380554774851,10.5282450923016));
#23942=CARTESIAN_POINT('Ctrl Pts',(17.0406955316219,-16.2402954425337,10.5224302623207));
#23943=CARTESIAN_POINT('Ctrl Pts',(17.1526817172575,-15.8342695060273,10.5098001955601));
#23944=CARTESIAN_POINT('Ctrl Pts',(17.1725541316423,-15.6670883207797,10.5045541305816));
#23945=CARTESIAN_POINT('Ctrl Pts',(17.1672595260838,-15.4999999894163,10.4992595260838));
#23946=CARTESIAN_POINT('',(14.2313898004749,-14.5577749122403,10.4122404735808));
#23947=CARTESIAN_POINT('Ctrl Pts',(14.2313898004748,-14.5577749122403,10.4122404735809));
#23948=CARTESIAN_POINT('Ctrl Pts',(14.330374396146,-14.3868080708335,10.4347157740671));
#23949=CARTESIAN_POINT('Ctrl Pts',(14.4592032863654,-14.2351112543341,10.4582731630844));
#23950=CARTESIAN_POINT('Ctrl Pts',(14.7697452366637,-13.9801784965913,10.5059067908598));
#23951=CARTESIAN_POINT('Ctrl Pts',(14.9504857682593,-13.8810021159152,10.5295757840915));
#23952=CARTESIAN_POINT('Ctrl Pts',(15.400735820047,-13.7335179124251,10.5809089218113));
#23953=CARTESIAN_POINT('Ctrl Pts',(15.6393119362485,-13.72523109504,10.6025326157022));
#23954=CARTESIAN_POINT('Ctrl Pts',(16.0071202509296,-13.7544578969706,10.6406359197886));
#23955=CARTESIAN_POINT('Ctrl Pts',(16.1857710734102,-13.7957662195931,10.6600613989418));
#23956=CARTESIAN_POINT('Ctrl Pts',(16.5282411323567,-13.9306559184475,10.6990893282765));
#23957=CARTESIAN_POINT('Ctrl Pts',(16.689788053325,-14.0244109494249,10.7184707369876));
#23958=CARTESIAN_POINT('Ctrl Pts',(16.8346987578547,-14.140733938563,10.7369999999983));
#23959=CARTESIAN_POINT('',(15.2436450846258,-13.9406917842497,10.4122404735808));
#23960=CARTESIAN_POINT('Origin',(15.5,-15.5,10.4122404735808));
#23961=CARTESIAN_POINT('Ctrl Pts',(17.1672595260838,-15.4999999894163,10.4992595260838));
#23962=CARTESIAN_POINT('Ctrl Pts',(17.1659601311851,-15.4589933982724,10.4979601314454));
#23963=CARTESIAN_POINT('Ctrl Pts',(17.1631450533059,-15.4179923936375,10.4966578716326));
#23964=CARTESIAN_POINT('Ctrl Pts',(17.135560386953,-15.1578207074097,10.4883749005502));
#23965=CARTESIAN_POINT('Ctrl Pts',(17.0690262278895,-14.9453351142648,10.4815187112057));
#23966=CARTESIAN_POINT('Ctrl Pts',(16.8460543493517,-14.5384028687359,10.4682409938133));
#23967=CARTESIAN_POINT('Ctrl Pts',(16.7012184908016,-14.3848385798802,10.4620910771043));
#23968=CARTESIAN_POINT('Ctrl Pts',(16.4090783980845,-14.1456891975148,10.4500509032636));
#23969=CARTESIAN_POINT('Ctrl Pts',(16.2259194615737,-14.0468505782317,10.4432455275581));
#23970=CARTESIAN_POINT('Ctrl Pts',(15.9056854194317,-13.9464878894083,10.4323954781035));
#23971=CARTESIAN_POINT('Ctrl Pts',(15.7780439261473,-13.9227846102375,10.428307423892));
#23972=CARTESIAN_POINT('Ctrl Pts',(15.5139662922323,-13.9059874790058,10.4203309872468));
#23973=CARTESIAN_POINT('Ctrl Pts',(15.3775884074022,-13.914345653723,10.4165086268908));
#23974=CARTESIAN_POINT('Ctrl Pts',(15.2436450846239,-13.9406917842501,10.4122404735808));
#23975=CARTESIAN_POINT('',(17.655,-15.5,10.987));
#23976=CARTESIAN_POINT('',(17.655,-15.5,10.987));
#23977=CARTESIAN_POINT('Origin',(15.5,-15.5,10.987));
#23978=CARTESIAN_POINT('Origin',(15.4999999999998,15.5000000000002,10.987));
#23979=CARTESIAN_POINT('',(15.4999999947079,17.167259526084,10.4992595260838));
#23980=CARTESIAN_POINT('Ctrl Pts',(13.5949999999991,15.5000000000298,10.7370000000007));
#23981=CARTESIAN_POINT('Ctrl Pts',(13.600849788101,15.2564355648587,10.731150211895));
#23982=CARTESIAN_POINT('Ctrl Pts',(13.6509446513241,15.0667953438098,10.7259167101341));
#23983=CARTESIAN_POINT('Ctrl Pts',(13.7548661865961,14.7648541061731,10.7172082071422));
#23984=CARTESIAN_POINT('Ctrl Pts',(13.8368618391331,14.6050214266467,10.7121852577502));
#23985=CARTESIAN_POINT('Ctrl Pts',(14.0739704882185,14.2704423654658,10.7006604618154));
#23986=CARTESIAN_POINT('Ctrl Pts',(14.2414766708351,14.1080191323993,10.6942562020695));
#23987=CARTESIAN_POINT('Ctrl Pts',(14.6374778586748,13.8453173047327,10.6819987621032));
#23988=CARTESIAN_POINT('Ctrl Pts',(14.8639328566015,13.7520840601203,10.6760021091628));
#23989=CARTESIAN_POINT('Ctrl Pts',(15.3364039022473,13.6614771916195,10.6624990364368));
#23990=CARTESIAN_POINT('Ctrl Pts',(15.5758065144269,13.6626363666949,10.655582285964));
#23991=CARTESIAN_POINT('Ctrl Pts',(16.0629129998439,13.7609513162709,10.6413472559484));
#23992=CARTESIAN_POINT('Ctrl Pts',(16.2635040621546,13.8578641877698,10.6354098660461));
#23993=CARTESIAN_POINT('Ctrl Pts',(16.6035611312114,14.0672823721137,10.6252403230947));
#23994=CARTESIAN_POINT('Ctrl Pts',(16.7766690302213,14.2283948799594,10.6186368111917));
#23995=CARTESIAN_POINT('Ctrl Pts',(17.0457728351728,14.6023972131454,10.605079928077));
#23996=CARTESIAN_POINT('Ctrl Pts',(17.1416118807008,14.8099919665041,10.5982690748862));
#23997=CARTESIAN_POINT('Ctrl Pts',(17.2495576082467,15.2485979050477,10.5851458477437));
#23998=CARTESIAN_POINT('Ctrl Pts',(17.2617643752446,15.4776646622055,10.5793320921389));
#23999=CARTESIAN_POINT('Ctrl Pts',(17.1990672566315,15.9104000163754,10.5671552873218));
#24000=CARTESIAN_POINT('Ctrl Pts',(17.1306302329423,16.111882863495,10.5608366679547));
#24001=CARTESIAN_POINT('Ctrl Pts',(16.9166251728486,16.4935678847174,10.5474332016161));
#24002=CARTESIAN_POINT('Ctrl Pts',(16.7678269424465,16.6673647635456,10.5404564545199));
#24003=CARTESIAN_POINT('Ctrl Pts',(16.4380554774367,16.9263243700677,10.5282450923));
#24004=CARTESIAN_POINT('Ctrl Pts',(16.2402954424824,17.0406955316445,10.5224302623191));
#24005=CARTESIAN_POINT('Ctrl Pts',(15.8342695059919,17.1526817172619,10.509800195559));
#24006=CARTESIAN_POINT('Ctrl Pts',(15.6670883207619,17.1725541316419,10.504554130581));
#24007=CARTESIAN_POINT('Ctrl Pts',(15.4999999894161,17.167259526084,10.4992595260838));
#24008=CARTESIAN_POINT('',(14.5577835109666,14.2313848221087,10.4122393431954));
#24009=CARTESIAN_POINT('Ctrl Pts',(14.5577835109666,14.2313848221087,10.4122393431954));
#24010=CARTESIAN_POINT('Ctrl Pts',(14.3868137807237,14.3303710903281,10.434715023448));
#24011=CARTESIAN_POINT('Ctrl Pts',(14.2351133713102,14.4592007076274,10.4582727675337));
#24012=CARTESIAN_POINT('Ctrl Pts',(13.9801784966279,14.7697452365986,10.5059067908511));
#24013=CARTESIAN_POINT('Ctrl Pts',(13.8810021159297,14.9504857682191,10.5295757840868));
#24014=CARTESIAN_POINT('Ctrl Pts',(13.7335179124459,15.4007358199769,10.5809089218035));
#24015=CARTESIAN_POINT('Ctrl Pts',(13.725231095046,15.6393119361218,10.6025326156897));
#24016=CARTESIAN_POINT('Ctrl Pts',(13.7544578969435,16.0071202507932,10.640635919774));
#24017=CARTESIAN_POINT('Ctrl Pts',(13.7957662195588,16.185771073299,10.6600613989296));
#24018=CARTESIAN_POINT('Ctrl Pts',(13.9306559184154,16.5282411323019,10.69908932827));
#24019=CARTESIAN_POINT('Ctrl Pts',(14.0244109494044,16.6897880532997,10.7184707369844));
#24020=CARTESIAN_POINT('Ctrl Pts',(14.1407339385614,16.8346987578534,10.7369999999982));
#24021=CARTESIAN_POINT('',(13.9406937133188,15.2436352774332,10.4122401610704));
#24022=CARTESIAN_POINT('Origin',(15.4999999999998,15.5000000000002,10.4122404735808));
#24023=CARTESIAN_POINT('Ctrl Pts',(15.4999999894161,17.167259526084,10.4992595260838));
#24024=CARTESIAN_POINT('Ctrl Pts',(15.4589933982536,17.1659601311847,10.4979601314448));
#24025=CARTESIAN_POINT('Ctrl Pts',(15.4179923936001,17.1631450533035,10.4966578716315));
#24026=CARTESIAN_POINT('Ctrl Pts',(15.1578207073548,17.1355603869399,10.4883749005484));
#24027=CARTESIAN_POINT('Ctrl Pts',(14.9453351142122,17.0690262278694,10.481518711204));
#24028=CARTESIAN_POINT('Ctrl Pts',(14.5384028686677,16.8460543493053,10.468240993811));
#24029=CARTESIAN_POINT('Ctrl Pts',(14.3848385798272,16.7012184907442,10.4620910771019));
#24030=CARTESIAN_POINT('Ctrl Pts',(14.1456891974921,16.4090783980489,10.4500509032622));
#24031=CARTESIAN_POINT('Ctrl Pts',(14.0468505782134,16.2259194615347,10.4432455275567));
#24032=CARTESIAN_POINT('Ctrl Pts',(13.9464878894004,15.9056854193956,10.4323954781023));
#24033=CARTESIAN_POINT('Ctrl Pts',(13.9227846102335,15.7780439261173,10.4283074238911));
#24034=CARTESIAN_POINT('Ctrl Pts',(13.9059874790066,15.5139662922165,10.4203309872464));
#24035=CARTESIAN_POINT('Ctrl Pts',(13.9143467252667,15.3775784311783,10.4165083253794));
#24036=CARTESIAN_POINT('Ctrl Pts',(13.9406937133188,15.2436352774332,10.4122401610704));
#24037=CARTESIAN_POINT('',(15.4999999999998,17.6550000000003,10.9870000000001));
#24038=CARTESIAN_POINT('',(15.4999999999998,17.6550000000002,10.987));
#24039=CARTESIAN_POINT('Origin',(15.5,15.5,10.987));
#24040=CARTESIAN_POINT('Origin',(-15.5,15.5,10.987));
#24041=CARTESIAN_POINT('',(-17.1672595260838,15.4999999947082,10.4992595260838));
#24042=CARTESIAN_POINT('Ctrl Pts',(-15.5000000000296,13.5949999999993,10.7370000000007));
#24043=CARTESIAN_POINT('Ctrl Pts',(-15.2564355648662,13.600849788101,10.7311502118952));
#24044=CARTESIAN_POINT('Ctrl Pts',(-15.0667953438228,13.6509446513211,10.7259167101345));
#24045=CARTESIAN_POINT('Ctrl Pts',(-14.7648541061942,13.7548661865872,10.7172082071429));
#24046=CARTESIAN_POINT('Ctrl Pts',(-14.6050214266715,13.8368618391195,10.712185257751));
#24047=CARTESIAN_POINT('Ctrl Pts',(-14.27044236549,14.0739704881962,10.7006604618163));
#24048=CARTESIAN_POINT('Ctrl Pts',(-14.1080191324201,14.2414766708108,10.6942562020704));
#24049=CARTESIAN_POINT('Ctrl Pts',(-13.8453173047464,14.6374778586467,10.681998762104));
#24050=CARTESIAN_POINT('Ctrl Pts',(-13.7520840601298,14.8639328565725,10.6760021091637));
#24051=CARTESIAN_POINT('Ctrl Pts',(-13.661477191621,15.336403902218,10.6624990364376));
#24052=CARTESIAN_POINT('Ctrl Pts',(-13.6626363666926,15.5758065143984,10.6555822859649));
#24053=CARTESIAN_POINT('Ctrl Pts',(-13.7609513162606,16.0629129998141,10.6413472559492));
#24054=CARTESIAN_POINT('Ctrl Pts',(-13.8578641877541,16.2635040621222,10.635409866047));
#24055=CARTESIAN_POINT('Ctrl Pts',(-14.0672823720874,16.6035611311796,10.6252403230958));
#24056=CARTESIAN_POINT('Ctrl Pts',(-14.2283948799295,16.7766690301937,10.6186368111928));
#24057=CARTESIAN_POINT('Ctrl Pts',(-14.6023972131106,17.0457728351544,10.6050799280782));
#24058=CARTESIAN_POINT('Ctrl Pts',(-14.8099919664681,17.1416118806874,10.5982690748874));
#24059=CARTESIAN_POINT('Ctrl Pts',(-15.2485979050077,17.2495576082419,10.5851458477448));
#24060=CARTESIAN_POINT('Ctrl Pts',(-15.4776646621617,17.2617643752449,10.57933209214));
#24061=CARTESIAN_POINT('Ctrl Pts',(-15.9104000163284,17.1990672566442,10.5671552873232));
#24062=CARTESIAN_POINT('Ctrl Pts',(-16.1118828634489,17.1306302329612,10.5608366679562));
#24063=CARTESIAN_POINT('Ctrl Pts',(-16.4935678846754,16.9166251728798,10.5474332016177));
#24064=CARTESIAN_POINT('Ctrl Pts',(-16.667364763507,16.767826942484,10.5404564545215));
#24065=CARTESIAN_POINT('Ctrl Pts',(-16.9263243700374,16.4380554774851,10.5282450923016));
#24066=CARTESIAN_POINT('Ctrl Pts',(-17.0406955316219,16.2402954425337,10.5224302623207));
#24067=CARTESIAN_POINT('Ctrl Pts',(-17.1526817172575,15.8342695060273,10.5098001955601));
#24068=CARTESIAN_POINT('Ctrl Pts',(-17.1725541316423,15.6670883207797,10.5045541305816));
#24069=CARTESIAN_POINT('Ctrl Pts',(-17.1672595260838,15.4999999894163,10.4992595260838));
#24070=CARTESIAN_POINT('',(-14.2313898004749,14.5577749122403,10.4122404735808));
#24071=CARTESIAN_POINT('Ctrl Pts',(-14.2313898004748,14.5577749122403,10.4122404735809));
#24072=CARTESIAN_POINT('Ctrl Pts',(-14.330374396146,14.3868080708335,10.4347157740671));
#24073=CARTESIAN_POINT('Ctrl Pts',(-14.4592032863654,14.2351112543341,10.4582731630844));
#24074=CARTESIAN_POINT('Ctrl Pts',(-14.7697452366637,13.9801784965913,10.5059067908598));
#24075=CARTESIAN_POINT('Ctrl Pts',(-14.9504857682593,13.8810021159152,10.5295757840915));
#24076=CARTESIAN_POINT('Ctrl Pts',(-15.400735820047,13.7335179124251,10.5809089218113));
#24077=CARTESIAN_POINT('Ctrl Pts',(-15.6393119362485,13.72523109504,10.6025326157022));
#24078=CARTESIAN_POINT('Ctrl Pts',(-16.0071202509296,13.7544578969706,10.6406359197886));
#24079=CARTESIAN_POINT('Ctrl Pts',(-16.1857710734102,13.7957662195931,10.6600613989418));
#24080=CARTESIAN_POINT('Ctrl Pts',(-16.5282411323567,13.9306559184475,10.6990893282765));
#24081=CARTESIAN_POINT('Ctrl Pts',(-16.689788053325,14.0244109494249,10.7184707369876));
#24082=CARTESIAN_POINT('Ctrl Pts',(-16.8346987578547,14.140733938563,10.7369999999983));
#24083=CARTESIAN_POINT('',(-15.2436450846258,13.9406917842497,10.4122404735808));
#24084=CARTESIAN_POINT('Origin',(-15.5,15.5,10.4122404735808));
#24085=CARTESIAN_POINT('Ctrl Pts',(-17.1672595260838,15.4999999894163,10.4992595260838));
#24086=CARTESIAN_POINT('Ctrl Pts',(-17.1659601311851,15.4589933982724,10.4979601314454));
#24087=CARTESIAN_POINT('Ctrl Pts',(-17.1631450533059,15.4179923936375,10.4966578716326));
#24088=CARTESIAN_POINT('Ctrl Pts',(-17.135560386953,15.1578207074097,10.4883749005502));
#24089=CARTESIAN_POINT('Ctrl Pts',(-17.0690262278895,14.9453351142648,10.4815187112057));
#24090=CARTESIAN_POINT('Ctrl Pts',(-16.8460543493517,14.5384028687359,10.4682409938133));
#24091=CARTESIAN_POINT('Ctrl Pts',(-16.7012184908016,14.3848385798802,10.4620910771043));
#24092=CARTESIAN_POINT('Ctrl Pts',(-16.4090783980845,14.1456891975148,10.4500509032636));
#24093=CARTESIAN_POINT('Ctrl Pts',(-16.2259194615737,14.0468505782317,10.4432455275581));
#24094=CARTESIAN_POINT('Ctrl Pts',(-15.9056854194317,13.9464878894083,10.4323954781035));
#24095=CARTESIAN_POINT('Ctrl Pts',(-15.7780439261473,13.9227846102375,10.428307423892));
#24096=CARTESIAN_POINT('Ctrl Pts',(-15.5139662922323,13.9059874790058,10.4203309872468));
#24097=CARTESIAN_POINT('Ctrl Pts',(-15.3775884074022,13.914345653723,10.4165086268908));
#24098=CARTESIAN_POINT('Ctrl Pts',(-15.2436450846239,13.9406917842501,10.4122404735808));
#24099=CARTESIAN_POINT('',(-17.655,15.5,10.987));
#24100=CARTESIAN_POINT('',(-17.655,15.5,10.987));
#24101=CARTESIAN_POINT('Origin',(-15.5,15.5,10.987));
#24102=CARTESIAN_POINT('Ctrl Pts',(-15.5,17.0802317716412,11.1745050240672));
#24103=CARTESIAN_POINT('Ctrl Pts',(-16.4123472387391,17.0802317716412,11.1328383574005));
#24104=CARTESIAN_POINT('Ctrl Pts',(-16.8685208581086,16.2901158858206,11.0911716907338));
#24105=CARTESIAN_POINT('Ctrl Pts',(-17.3246944774781,15.5,11.0495050240672));
#24106=CARTESIAN_POINT('Ctrl Pts',(-16.8685208581086,14.7098841141794,11.0078383574005));
#24107=CARTESIAN_POINT('Ctrl Pts',(-16.4123472387391,13.9197682283588,10.9661716907338));
#24108=CARTESIAN_POINT('Ctrl Pts',(-15.5,13.9197682283588,10.9245050240672));
#24109=CARTESIAN_POINT('Ctrl Pts',(-14.5876527612609,13.9197682283588,10.8828383574005));
#24110=CARTESIAN_POINT('Ctrl Pts',(-14.1314791418914,14.7098841141794,10.8411716907338));
#24111=CARTESIAN_POINT('Ctrl Pts',(-13.6753055225219,15.5,10.7995050240672));
#24112=CARTESIAN_POINT('Ctrl Pts',(-14.1314791418914,16.2901158858206,10.7578383574005));
#24113=CARTESIAN_POINT('Ctrl Pts',(-14.5876527612609,17.0802317716412,10.7161716907338));
#24114=CARTESIAN_POINT('Ctrl Pts',(-15.5,17.0802317716412,10.6745050240672));
#24115=CARTESIAN_POINT('Ctrl Pts',(-16.4123472387391,17.0802317716412,10.6328383574005));
#24116=CARTESIAN_POINT('Ctrl Pts',(-16.8685208581086,16.2901158858206,10.5911716907338));
#24117=CARTESIAN_POINT('Ctrl Pts',(-17.3246944774781,15.5,10.5495050240672));
#24118=CARTESIAN_POINT('Ctrl Pts',(-16.8685208581086,14.7098841141794,10.5078383574005));
#24119=CARTESIAN_POINT('Ctrl Pts',(-16.4123472387391,13.9197682283588,10.4661716907338));
#24120=CARTESIAN_POINT('Ctrl Pts',(-15.5,13.9197682283588,10.4245050240672));
#24121=CARTESIAN_POINT('Ctrl Pts',(-14.5876527612609,13.9197682283588,10.3828383574005));
#24122=CARTESIAN_POINT('Ctrl Pts',(-14.1314791418914,14.7098841141794,10.3411716907338));
#24123=CARTESIAN_POINT('Ctrl Pts',(-13.6753055225219,15.5,10.2995050240672));
#24124=CARTESIAN_POINT('Ctrl Pts',(-14.1314791418914,16.2901158858206,10.2578383574005));
#24125=CARTESIAN_POINT('Ctrl Pts',(-14.5876527612609,17.0802317716412,10.2161716907338));
#24126=CARTESIAN_POINT('Ctrl Pts',(-15.5,17.0802317716412,10.1745050240672));
#24127=CARTESIAN_POINT('Ctrl Pts',(-16.4123472387391,17.0802317716412,10.1328383574005));
#24128=CARTESIAN_POINT('Ctrl Pts',(-16.8685208581086,16.2901158858206,10.0911716907338));
#24129=CARTESIAN_POINT('Ctrl Pts',(-17.3246944774781,15.5,10.0495050240672));
#24130=CARTESIAN_POINT('Ctrl Pts',(-16.8685208581086,14.7098841141794,10.0078383574005));
#24131=CARTESIAN_POINT('Ctrl Pts',(-16.4123472387391,13.9197682283588,9.96617169073382));
#24132=CARTESIAN_POINT('Ctrl Pts',(-15.5,13.9197682283588,9.92450502406715));
#24133=CARTESIAN_POINT('Ctrl Pts',(-14.5876527612609,13.9197682283588,9.88283835740048));
#24134=CARTESIAN_POINT('Ctrl Pts',(-14.1314791418914,14.7098841141794,9.84117169073382));
#24135=CARTESIAN_POINT('Ctrl Pts',(-13.6753055225219,15.5,9.79950502406715));
#24136=CARTESIAN_POINT('Ctrl Pts',(-14.1314791418914,16.2901158858206,9.75783835740048));
#24137=CARTESIAN_POINT('Ctrl Pts',(-14.5876527612609,17.0802317716412,9.71617169073381));
#24138=CARTESIAN_POINT('Ctrl Pts',(-15.5,17.0802317716412,9.67450502406715));
#24139=CARTESIAN_POINT('Ctrl Pts',(-16.4123472387391,17.0802317716412,9.63283835740048));
#24140=CARTESIAN_POINT('Ctrl Pts',(-16.8685208581086,16.2901158858206,9.59117169073381));
#24141=CARTESIAN_POINT('Ctrl Pts',(-17.3246944774781,15.5,9.54950502406714));
#24142=CARTESIAN_POINT('Ctrl Pts',(-16.8685208581086,14.7098841141794,9.50783835740048));
#24143=CARTESIAN_POINT('Ctrl Pts',(-16.4123472387391,13.9197682283588,9.46617169073381));
#24144=CARTESIAN_POINT('Ctrl Pts',(-15.5,13.9197682283588,9.42450502406714));
#24145=CARTESIAN_POINT('Ctrl Pts',(-14.5876527612609,13.9197682283588,9.38283835740048));
#24146=CARTESIAN_POINT('Ctrl Pts',(-14.1314791418914,14.7098841141794,9.34117169073381));
#24147=CARTESIAN_POINT('Ctrl Pts',(-13.6753055225219,15.5,9.29950502406714));
#24148=CARTESIAN_POINT('Ctrl Pts',(-14.1314791418914,16.2901158858206,9.25783835740048));
#24149=CARTESIAN_POINT('Ctrl Pts',(-14.5876527612609,17.0802317716412,9.21617169073381));
#24150=CARTESIAN_POINT('Ctrl Pts',(-15.5,17.0802317716412,9.17450502406714));
#24151=CARTESIAN_POINT('Ctrl Pts',(-16.4123472387391,17.0802317716412,9.13283835740047));
#24152=CARTESIAN_POINT('Ctrl Pts',(-16.8685208581086,16.2901158858206,9.09117169073381));
#24153=CARTESIAN_POINT('Ctrl Pts',(-17.3246944774781,15.5,9.04950502406714));
#24154=CARTESIAN_POINT('Ctrl Pts',(-16.8685208581086,14.7098841141794,9.00783835740047));
#24155=CARTESIAN_POINT('Ctrl Pts',(-16.4123472387391,13.9197682283588,8.9661716907338));
#24156=CARTESIAN_POINT('Ctrl Pts',(-15.5,13.9197682283588,8.92450502406714));
#24157=CARTESIAN_POINT('Ctrl Pts',(-14.5876527612609,13.9197682283588,8.88283835740047));
#24158=CARTESIAN_POINT('Ctrl Pts',(-14.1314791418914,14.7098841141794,8.8411716907338));
#24159=CARTESIAN_POINT('Ctrl Pts',(-13.6753055225219,15.5,8.79950502406713));
#24160=CARTESIAN_POINT('Ctrl Pts',(-14.1314791418914,16.2901158858206,8.75783835740047));
#24161=CARTESIAN_POINT('Ctrl Pts',(-14.5876527612609,17.0802317716412,8.7161716907338));
#24162=CARTESIAN_POINT('Ctrl Pts',(-15.5,17.0802317716412,8.67450502406713));
#24163=CARTESIAN_POINT('Ctrl Pts',(-16.4123472387391,17.0802317716412,8.63283835740047));
#24164=CARTESIAN_POINT('Ctrl Pts',(-16.8685208581086,16.2901158858206,8.5911716907338));
#24165=CARTESIAN_POINT('Ctrl Pts',(-17.3246944774781,15.5,8.54950502406713));
#24166=CARTESIAN_POINT('Ctrl Pts',(-16.8685208581086,14.7098841141794,8.50783835740046));
#24167=CARTESIAN_POINT('Ctrl Pts',(-16.4123472387391,13.9197682283588,8.4661716907338));
#24168=CARTESIAN_POINT('Ctrl Pts',(-15.5,13.9197682283588,8.42450502406713));
#24169=CARTESIAN_POINT('Ctrl Pts',(-14.5876527612609,13.9197682283588,8.38283835740046));
#24170=CARTESIAN_POINT('Ctrl Pts',(-14.1314791418914,14.7098841141794,8.3411716907338));
#24171=CARTESIAN_POINT('Ctrl Pts',(-13.6753055225219,15.5,8.29950502406713));
#24172=CARTESIAN_POINT('Ctrl Pts',(-14.1314791418914,16.2901158858206,8.25783835740046));
#24173=CARTESIAN_POINT('Ctrl Pts',(-14.5876527612609,17.0802317716412,8.21617169073379));
#24174=CARTESIAN_POINT('Ctrl Pts',(-15.5,17.0802317716412,8.17450502406713));
#24175=CARTESIAN_POINT('Ctrl Pts',(-16.4123472387391,17.0802317716412,8.13283835740046));
#24176=CARTESIAN_POINT('Ctrl Pts',(-16.8685208581086,16.2901158858206,8.09117169073379));
#24177=CARTESIAN_POINT('Ctrl Pts',(-17.3246944774781,15.5,8.04950502406713));
#24178=CARTESIAN_POINT('Ctrl Pts',(-16.8685208581086,14.7098841141794,8.00783835740046));
#24179=CARTESIAN_POINT('Ctrl Pts',(-16.4123472387391,13.9197682283588,7.96617169073379));
#24180=CARTESIAN_POINT('Ctrl Pts',(-15.5,13.9197682283588,7.92450502406712));
#24181=CARTESIAN_POINT('Ctrl Pts',(-14.5876527612609,13.9197682283588,7.88283835740046));
#24182=CARTESIAN_POINT('Ctrl Pts',(-14.1314791418914,14.7098841141794,7.84117169073379));
#24183=CARTESIAN_POINT('Ctrl Pts',(-13.6753055225219,15.5,7.79950502406712));
#24184=CARTESIAN_POINT('Ctrl Pts',(-14.1314791418914,16.2901158858206,7.75783835740046));
#24185=CARTESIAN_POINT('Ctrl Pts',(-14.5876527612609,17.0802317716412,7.71617169073378));
#24186=CARTESIAN_POINT('Ctrl Pts',(-15.5,17.0802317716412,7.67450502406712));
#24187=CARTESIAN_POINT('Ctrl Pts',(-16.4123472387391,17.0802317716412,7.63283835740045));
#24188=CARTESIAN_POINT('Ctrl Pts',(-16.8685208581086,16.2901158858206,7.59117169073379));
#24189=CARTESIAN_POINT('Ctrl Pts',(-17.3246944774781,15.5,7.54950502406712));
#24190=CARTESIAN_POINT('Ctrl Pts',(-16.8685208581086,14.7098841141794,7.50783835740045));
#24191=CARTESIAN_POINT('Ctrl Pts',(-16.4123472387391,13.9197682283588,7.46617169073379));
#24192=CARTESIAN_POINT('Ctrl Pts',(-15.5,13.9197682283588,7.42450502406712));
#24193=CARTESIAN_POINT('Ctrl Pts',(-14.5876527612609,13.9197682283588,7.38283835740045));
#24194=CARTESIAN_POINT('Ctrl Pts',(-14.1314791418914,14.7098841141794,7.34117169073378));
#24195=CARTESIAN_POINT('Ctrl Pts',(-13.6753055225219,15.5,7.29950502406711));
#24196=CARTESIAN_POINT('Ctrl Pts',(-14.1314791418914,16.2901158858206,7.25783835740045));
#24197=CARTESIAN_POINT('Ctrl Pts',(-14.5876527612609,17.0802317716412,7.21617169073378));
#24198=CARTESIAN_POINT('Ctrl Pts',(-15.5,17.0802317716412,7.17450502406711));
#24199=CARTESIAN_POINT('Ctrl Pts',(-16.4123472387391,17.0802317716412,7.13283835740044));
#24200=CARTESIAN_POINT('Ctrl Pts',(-16.8685208581086,16.2901158858206,7.09117169073378));
#24201=CARTESIAN_POINT('Ctrl Pts',(-17.3246944774781,15.5,7.04950502406711));
#24202=CARTESIAN_POINT('Ctrl Pts',(-16.8685208581086,14.7098841141794,7.00783835740045));
#24203=CARTESIAN_POINT('Ctrl Pts',(-16.4123472387391,13.9197682283588,6.96617169073378));
#24204=CARTESIAN_POINT('Ctrl Pts',(-15.5,13.9197682283588,6.92450502406711));
#24205=CARTESIAN_POINT('Ctrl Pts',(-14.5876527612609,13.9197682283588,6.88283835740044));
#24206=CARTESIAN_POINT('Ctrl Pts',(-14.1314791418914,14.7098841141794,6.84117169073378));
#24207=CARTESIAN_POINT('Ctrl Pts',(-13.6753055225219,15.5,6.79950502406711));
#24208=CARTESIAN_POINT('Ctrl Pts',(-14.1314791418914,16.2901158858206,6.75783835740044));
#24209=CARTESIAN_POINT('Ctrl Pts',(-14.5876527612609,17.0802317716412,6.71617169073377));
#24210=CARTESIAN_POINT('Ctrl Pts',(-15.5,17.0802317716412,6.67450502406711));
#24211=CARTESIAN_POINT('Ctrl Pts',(-16.4123472387391,17.0802317716412,6.63283835740044));
#24212=CARTESIAN_POINT('Ctrl Pts',(-16.8685208581086,16.2901158858206,6.59117169073377));
#24213=CARTESIAN_POINT('Ctrl Pts',(-17.3246944774781,15.5,6.54950502406711));
#24214=CARTESIAN_POINT('Ctrl Pts',(-16.8685208581086,14.7098841141794,6.50783835740044));
#24215=CARTESIAN_POINT('Ctrl Pts',(-16.4123472387391,13.9197682283588,6.46617169073377));
#24216=CARTESIAN_POINT('Ctrl Pts',(-15.5,13.9197682283588,6.4245050240671));
#24217=CARTESIAN_POINT('Ctrl Pts',(-14.5876527612609,13.9197682283588,6.38283835740044));
#24218=CARTESIAN_POINT('Ctrl Pts',(-14.1314791418914,14.7098841141794,6.34117169073377));
#24219=CARTESIAN_POINT('Ctrl Pts',(-13.6753055225219,15.5,6.2995050240671));
#24220=CARTESIAN_POINT('Ctrl Pts',(-14.1314791418914,16.2901158858206,6.25783835740044));
#24221=CARTESIAN_POINT('Ctrl Pts',(-14.5876527612609,17.0802317716412,6.21617169073377));
#24222=CARTESIAN_POINT('Ctrl Pts',(-15.5,17.0802317716412,6.1745050240671));
#24223=CARTESIAN_POINT('Ctrl Pts',(-16.4123472387391,17.0802317716412,6.13283835740043));
#24224=CARTESIAN_POINT('Ctrl Pts',(-16.8685208581086,16.2901158858206,6.09117169073377));
#24225=CARTESIAN_POINT('Ctrl Pts',(-17.3246944774781,15.5,6.0495050240671));
#24226=CARTESIAN_POINT('Ctrl Pts',(-16.8685208581086,14.7098841141794,6.00783835740043));
#24227=CARTESIAN_POINT('Ctrl Pts',(-16.4123472387391,13.9197682283588,5.96617169073376));
#24228=CARTESIAN_POINT('Ctrl Pts',(-15.5,13.9197682283588,5.9245050240671));
#24229=CARTESIAN_POINT('Ctrl Pts',(-14.5876527612609,13.9197682283588,5.88283835740043));
#24230=CARTESIAN_POINT('Ctrl Pts',(-14.1314791418914,14.7098841141794,5.84117169073376));
#24231=CARTESIAN_POINT('Ctrl Pts',(-13.6753055225219,15.5,5.79950502406709));
#24232=CARTESIAN_POINT('Ctrl Pts',(-14.1314791418914,16.2901158858206,5.75783835740043));
#24233=CARTESIAN_POINT('Ctrl Pts',(-14.5876527612609,17.0802317716412,5.71617169073376));
#24234=CARTESIAN_POINT('Ctrl Pts',(-15.5,17.0802317716412,5.67450502406709));
#24235=CARTESIAN_POINT('Ctrl Pts',(-16.4123472387391,17.0802317716412,5.63283835740043));
#24236=CARTESIAN_POINT('Ctrl Pts',(-16.8685208581086,16.2901158858206,5.59117169073376));
#24237=CARTESIAN_POINT('Ctrl Pts',(-17.3246944774781,15.5,5.54950502406709));
#24238=CARTESIAN_POINT('Ctrl Pts',(-16.8685208581086,14.7098841141794,5.50783835740043));
#24239=CARTESIAN_POINT('Ctrl Pts',(-16.4123472387391,13.9197682283588,5.46617169073376));
#24240=CARTESIAN_POINT('Ctrl Pts',(-15.5,13.9197682283588,5.42450502406709));
#24241=CARTESIAN_POINT('Ctrl Pts',(-14.5876527612609,13.9197682283588,5.38283835740042));
#24242=CARTESIAN_POINT('Ctrl Pts',(-14.1314791418914,14.7098841141794,5.34117169073376));
#24243=CARTESIAN_POINT('Ctrl Pts',(-13.6753055225219,15.5,5.29950502406709));
#24244=CARTESIAN_POINT('Ctrl Pts',(-14.1314791418914,16.2901158858206,5.25783835740042));
#24245=CARTESIAN_POINT('Ctrl Pts',(-14.5876527612609,17.0802317716412,5.21617169073375));
#24246=CARTESIAN_POINT('Ctrl Pts',(-15.5,17.0802317716412,5.17450502406709));
#24247=CARTESIAN_POINT('Ctrl Pts',(-16.4123472387391,17.0802317716412,5.13283835740042));
#24248=CARTESIAN_POINT('Ctrl Pts',(-16.8685208581086,16.2901158858206,5.09117169073375));
#24249=CARTESIAN_POINT('Ctrl Pts',(-17.3246944774781,15.5,5.04950502406708));
#24250=CARTESIAN_POINT('Ctrl Pts',(-16.8685208581086,14.7098841141794,5.00783835740042));
#24251=CARTESIAN_POINT('Ctrl Pts',(-16.4123472387391,13.9197682283588,4.96617169073375));
#24252=CARTESIAN_POINT('Ctrl Pts',(-15.5,13.9197682283588,4.92450502406708));
#24253=CARTESIAN_POINT('Ctrl Pts',(-14.5876527612609,13.9197682283588,4.88283835740042));
#24254=CARTESIAN_POINT('Ctrl Pts',(-14.1314791418914,14.7098841141794,4.84117169073375));
#24255=CARTESIAN_POINT('Ctrl Pts',(-13.6753055225219,15.5,4.79950502406708));
#24256=CARTESIAN_POINT('Ctrl Pts',(-14.1314791418914,16.2901158858206,4.75783835740041));
#24257=CARTESIAN_POINT('Ctrl Pts',(-14.5876527612609,17.0802317716412,4.71617169073375));
#24258=CARTESIAN_POINT('Ctrl Pts',(-15.5,17.0802317716412,4.67450502406708));
#24259=CARTESIAN_POINT('Ctrl Pts',(-16.4123472387391,17.0802317716412,4.63283835740041));
#24260=CARTESIAN_POINT('Ctrl Pts',(-16.8685208581086,16.2901158858206,4.59117169073375));
#24261=CARTESIAN_POINT('Ctrl Pts',(-17.3246944774781,15.5,4.54950502406708));
#24262=CARTESIAN_POINT('Ctrl Pts',(-16.8685208581086,14.7098841141794,4.50783835740041));
#24263=CARTESIAN_POINT('Ctrl Pts',(-16.4123472387391,13.9197682283588,4.46617169073374));
#24264=CARTESIAN_POINT('Ctrl Pts',(-15.5,13.9197682283588,4.42450502406708));
#24265=CARTESIAN_POINT('Ctrl Pts',(-14.5876527612609,13.9197682283588,4.38283835740041));
#24266=CARTESIAN_POINT('Ctrl Pts',(-14.1314791418914,14.7098841141794,4.34117169073374));
#24267=CARTESIAN_POINT('Ctrl Pts',(-13.6753055225219,15.5,4.29950502406708));
#24268=CARTESIAN_POINT('Ctrl Pts',(-14.1314791418914,16.2901158858206,4.25783835740041));
#24269=CARTESIAN_POINT('Ctrl Pts',(-14.5876527612609,17.0802317716412,4.21617169073374));
#24270=CARTESIAN_POINT('Ctrl Pts',(-15.5,17.0802317716412,4.17450502406707));
#24271=CARTESIAN_POINT('Ctrl Pts',(-16.4123472387391,17.0802317716412,4.13283835740041));
#24272=CARTESIAN_POINT('Ctrl Pts',(-16.8685208581086,16.2901158858206,4.09117169073374));
#24273=CARTESIAN_POINT('Ctrl Pts',(-17.3246944774781,15.5,4.04950502406707));
#24274=CARTESIAN_POINT('Ctrl Pts',(-16.8685208581086,14.7098841141794,4.0078383574004));
#24275=CARTESIAN_POINT('Ctrl Pts',(-16.4123472387391,13.9197682283588,3.96617169073374));
#24276=CARTESIAN_POINT('Ctrl Pts',(-15.5,13.9197682283588,3.92450502406707));
#24277=CARTESIAN_POINT('Ctrl Pts',(-14.5876527612609,13.9197682283588,3.8828383574004));
#24278=CARTESIAN_POINT('Ctrl Pts',(-14.1314791418914,14.7098841141794,3.84117169073374));
#24279=CARTESIAN_POINT('Ctrl Pts',(-13.6753055225219,15.5,3.79950502406707));
#24280=CARTESIAN_POINT('Ctrl Pts',(-14.1314791418914,16.2901158858206,3.7578383574004));
#24281=CARTESIAN_POINT('Ctrl Pts',(-14.5876527612609,17.0802317716412,3.71617169073373));
#24282=CARTESIAN_POINT('Ctrl Pts',(-15.5,17.0802317716412,3.67450502406707));
#24283=CARTESIAN_POINT('Ctrl Pts',(-16.4123472387391,17.0802317716412,3.6328383574004));
#24284=CARTESIAN_POINT('Ctrl Pts',(-16.8685208581086,16.2901158858206,3.59117169073373));
#24285=CARTESIAN_POINT('Ctrl Pts',(-17.3246944774781,15.5,3.54950502406707));
#24286=CARTESIAN_POINT('Ctrl Pts',(-16.8685208581086,14.7098841141794,3.5078383574004));
#24287=CARTESIAN_POINT('Ctrl Pts',(-16.4123472387391,13.9197682283588,3.46617169073373));
#24288=CARTESIAN_POINT('Ctrl Pts',(-15.5,13.9197682283588,3.42450502406706));
#24289=CARTESIAN_POINT('Ctrl Pts',(-14.5876527612609,13.9197682283588,3.3828383574004));
#24290=CARTESIAN_POINT('Ctrl Pts',(-14.1314791418914,14.7098841141794,3.34117169073373));
#24291=CARTESIAN_POINT('Ctrl Pts',(-13.6753055225219,15.5,3.29950502406706));
#24292=CARTESIAN_POINT('Ctrl Pts',(-14.1314791418914,16.2901158858206,3.2578383574004));
#24293=CARTESIAN_POINT('Ctrl Pts',(-14.5876527612609,17.0802317716412,3.21617169073373));
#24294=CARTESIAN_POINT('Ctrl Pts',(-15.5,17.0802317716412,3.17450502406706));
#24295=CARTESIAN_POINT('Ctrl Pts',(-16.4123472387391,17.0802317716412,3.13283835740039));
#24296=CARTESIAN_POINT('Ctrl Pts',(-16.8685208581086,16.2901158858206,3.09117169073373));
#24297=CARTESIAN_POINT('Ctrl Pts',(-17.3246944774781,15.5,3.04950502406706));
#24298=CARTESIAN_POINT('Ctrl Pts',(-16.8685208581086,14.7098841141794,3.00783835740039));
#24299=CARTESIAN_POINT('Ctrl Pts',(-16.4123472387391,13.9197682283588,2.96617169073372));
#24300=CARTESIAN_POINT('Ctrl Pts',(-15.5,13.9197682283588,2.92450502406706));
#24301=CARTESIAN_POINT('Ctrl Pts',(-14.5876527612609,13.9197682283588,2.88283835740039));
#24302=CARTESIAN_POINT('Ctrl Pts',(-14.1314791418914,14.7098841141794,2.84117169073372));
#24303=CARTESIAN_POINT('Ctrl Pts',(-13.6753055225219,15.5,2.79950502406705));
#24304=CARTESIAN_POINT('Ctrl Pts',(-14.1314791418914,16.2901158858206,2.75783835740039));
#24305=CARTESIAN_POINT('Ctrl Pts',(-14.5876527612609,17.0802317716412,2.71617169073372));
#24306=CARTESIAN_POINT('Ctrl Pts',(-15.5,17.0802317716412,2.67450502406705));
#24307=CARTESIAN_POINT('Ctrl Pts',(-16.4123472387391,17.0802317716412,2.63283835740039));
#24308=CARTESIAN_POINT('Ctrl Pts',(-16.8685208581086,16.2901158858206,2.59117169073372));
#24309=CARTESIAN_POINT('Ctrl Pts',(-17.3246944774781,15.5,2.54950502406705));
#24310=CARTESIAN_POINT('Ctrl Pts',(-16.8685208581086,14.7098841141794,2.50783835740038));
#24311=CARTESIAN_POINT('Ctrl Pts',(-16.4123472387391,13.9197682283588,2.46617169073372));
#24312=CARTESIAN_POINT('Ctrl Pts',(-15.5,13.9197682283588,2.42450502406705));
#24313=CARTESIAN_POINT('Ctrl Pts',(-14.5876527612609,13.9197682283588,2.38283835740038));
#24314=CARTESIAN_POINT('Ctrl Pts',(-14.1314791418914,14.7098841141794,2.34117169073371));
#24315=CARTESIAN_POINT('Ctrl Pts',(-13.6753055225219,15.5,2.29950502406705));
#24316=CARTESIAN_POINT('Ctrl Pts',(-14.1314791418914,16.2901158858206,2.25783835740038));
#24317=CARTESIAN_POINT('Ctrl Pts',(-14.5876527612609,17.0802317716412,2.21617169073371));
#24318=CARTESIAN_POINT('Ctrl Pts',(-15.5,17.0802317716412,2.17450502406705));
#24319=CARTESIAN_POINT('Ctrl Pts',(-16.4123472387391,17.0802317716412,2.13283835740038));
#24320=CARTESIAN_POINT('Ctrl Pts',(-16.8685208581086,16.2901158858206,2.09117169073371));
#24321=CARTESIAN_POINT('Ctrl Pts',(-17.3246944774781,15.5,2.04950502406705));
#24322=CARTESIAN_POINT('Ctrl Pts',(-16.8685208581086,14.7098841141794,2.00783835740038));
#24323=CARTESIAN_POINT('Ctrl Pts',(-16.4123472387391,13.9197682283588,1.96617169073371));
#24324=CARTESIAN_POINT('Ctrl Pts',(-15.5,13.9197682283588,1.92450502406704));
#24325=CARTESIAN_POINT('Ctrl Pts',(-14.5876527612609,13.9197682283588,1.88283835740038));
#24326=CARTESIAN_POINT('Ctrl Pts',(-14.1314791418914,14.7098841141794,1.84117169073371));
#24327=CARTESIAN_POINT('Ctrl Pts',(-13.6753055225219,15.5,1.79950502406704));
#24328=CARTESIAN_POINT('Ctrl Pts',(-14.1314791418914,16.2901158858206,1.75783835740037));
#24329=CARTESIAN_POINT('Ctrl Pts',(-14.5876527612609,17.0802317716412,1.71617169073371));
#24330=CARTESIAN_POINT('Ctrl Pts',(-15.5,17.0802317716412,1.67450502406704));
#24331=CARTESIAN_POINT('Ctrl Pts',(-16.4123472387391,17.0802317716412,1.63283835740037));
#24332=CARTESIAN_POINT('Ctrl Pts',(-16.8685208581086,16.2901158858206,1.59117169073371));
#24333=CARTESIAN_POINT('Ctrl Pts',(-17.3246944774781,15.5,1.54950502406704));
#24334=CARTESIAN_POINT('Ctrl Pts',(-16.8685208581086,14.7098841141794,1.50783835740037));
#24335=CARTESIAN_POINT('Ctrl Pts',(-16.4123472387391,13.9197682283588,1.4661716907337));
#24336=CARTESIAN_POINT('Ctrl Pts',(-15.5,13.9197682283588,1.42450502406704));
#24337=CARTESIAN_POINT('Ctrl Pts',(-14.5876527612609,13.9197682283588,1.38283835740037));
#24338=CARTESIAN_POINT('Ctrl Pts',(-14.1314791418914,14.7098841141794,1.3411716907337));
#24339=CARTESIAN_POINT('Ctrl Pts',(-13.6753055225219,15.5,1.29950502406703));
#24340=CARTESIAN_POINT('Ctrl Pts',(-14.1314791418914,16.2901158858206,1.25783835740037));
#24341=CARTESIAN_POINT('Ctrl Pts',(-14.5876527612609,17.0802317716412,1.2161716907337));
#24342=CARTESIAN_POINT('Ctrl Pts',(-15.5,17.0802317716412,1.17450502406703));
#24343=CARTESIAN_POINT('Ctrl Pts',(-16.4123472387391,17.0802317716412,1.13283835740037));
#24344=CARTESIAN_POINT('Ctrl Pts',(-16.8685208581086,16.2901158858206,1.0911716907337));
#24345=CARTESIAN_POINT('Ctrl Pts',(-17.3246944774781,15.5,1.04950502406703));
#24346=CARTESIAN_POINT('Ctrl Pts',(-16.8685208581086,14.7098841141794,1.00783835740037));
#24347=CARTESIAN_POINT('Ctrl Pts',(-16.4123472387391,13.9197682283588,0.966171690733698));
#24348=CARTESIAN_POINT('Ctrl Pts',(-15.5,13.9197682283588,0.924505024067031));
#24349=CARTESIAN_POINT('Ctrl Pts',(-14.5876527612609,13.9197682283588,0.882838357400363));
#24350=CARTESIAN_POINT('Ctrl Pts',(-14.1314791418914,14.7098841141794,0.841171690733696));
#24351=CARTESIAN_POINT('Ctrl Pts',(-13.6753055225219,15.5,0.799505024067029));
#24352=CARTESIAN_POINT('Ctrl Pts',(-14.1314791418914,16.2901158858206,0.757838357400362));
#24353=CARTESIAN_POINT('Ctrl Pts',(-14.5876527612609,17.0802317716412,0.716171690733694));
#24354=CARTESIAN_POINT('Ctrl Pts',(-15.5,17.0802317716412,0.674505024067027));
#24355=CARTESIAN_POINT('Ctrl Pts',(-16.4123472387391,17.0802317716412,0.632838357400359));
#24356=CARTESIAN_POINT('Ctrl Pts',(-16.8685208581086,16.2901158858206,0.591171690733692));
#24357=CARTESIAN_POINT('Ctrl Pts',(-17.3246944774781,15.5,0.549505024067025));
#24358=CARTESIAN_POINT('Ctrl Pts',(-16.8685208581086,14.7098841141794,0.507838357400358));
#24359=CARTESIAN_POINT('Ctrl Pts',(-16.4123472387391,13.9197682283588,0.46617169073369));
#24360=CARTESIAN_POINT('Ctrl Pts',(-15.5,13.9197682283588,0.424505024067023));
#24361=CARTESIAN_POINT('Ctrl Pts',(-14.5876527612609,13.9197682283588,0.382838357400356));
#24362=CARTESIAN_POINT('Ctrl Pts',(-14.1314791418914,14.7098841141794,0.341171690733689));
#24363=CARTESIAN_POINT('Ctrl Pts',(-13.6753055225219,15.5,0.299505024067021));
#24364=CARTESIAN_POINT('Ctrl Pts',(-14.1314791418914,16.2901158858206,0.257838357400354));
#24365=CARTESIAN_POINT('Ctrl Pts',(-14.5876527612609,17.0802317716412,0.216171690733687));
#24366=CARTESIAN_POINT('Ctrl Pts',(-15.5,17.0802317716412,0.174505024067019));
#24367=CARTESIAN_POINT('Ctrl Pts',(-16.4123472387391,17.0802317716412,0.132838357400352));
#24368=CARTESIAN_POINT('Ctrl Pts',(-16.8685208581086,16.2901158858206,0.0911716907336849));
#24369=CARTESIAN_POINT('Ctrl Pts',(-17.3246944774781,15.5,0.0495050240670176));
#24370=CARTESIAN_POINT('Ctrl Pts',(-16.8685208581086,14.7098841141794,0.00783835740035031));
#24371=CARTESIAN_POINT('Ctrl Pts',(-16.4123472387391,13.9197682283588,-0.033828309266317));
#24372=CARTESIAN_POINT('Ctrl Pts',(-15.5,13.9197682283588,-0.0754949759329843));
#24373=CARTESIAN_POINT('Ctrl Pts',(-14.5876527612609,13.9197682283588,-0.11716164259965));
#24374=CARTESIAN_POINT('Ctrl Pts',(-14.1314791418914,14.7098841141794,-0.158828309266317));
#24375=CARTESIAN_POINT('Ctrl Pts',(-13.6753055225219,15.5,-0.200494975932984));
#24376=CARTESIAN_POINT('Ctrl Pts',(-14.1314791418914,16.2901158858206,-0.242161642599652));
#24377=CARTESIAN_POINT('Ctrl Pts',(-14.5876527612609,17.0802317716412,-0.283828309266319));
#24378=CARTESIAN_POINT('Ctrl Pts',(-15.5,17.0802317716412,-0.325494975932986));
#24379=CARTESIAN_POINT('Ctrl Pts',(-16.4123472387391,17.0802317716412,-0.367161642599654));
#24380=CARTESIAN_POINT('Ctrl Pts',(-16.8685208581086,16.2901158858206,-0.408828309266321));
#24381=CARTESIAN_POINT('Ctrl Pts',(-17.3246944774781,15.5,-0.450494975932988));
#24382=CARTESIAN_POINT('Ctrl Pts',(-16.8685208581086,14.7098841141794,-0.492161642599655));
#24383=CARTESIAN_POINT('Ctrl Pts',(-16.4123472387391,13.9197682283588,-0.533828309266323));
#24384=CARTESIAN_POINT('Ctrl Pts',(-15.5,13.9197682283588,-0.57549497593299));
#24385=CARTESIAN_POINT('Ctrl Pts',(-14.5876527612609,13.9197682283588,-0.617161642599657));
#24386=CARTESIAN_POINT('Ctrl Pts',(-14.1314791418914,14.7098841141794,-0.658828309266325));
#24387=CARTESIAN_POINT('Ctrl Pts',(-13.6753055225219,15.5,-0.700494975932992));
#24388=CARTESIAN_POINT('Ctrl Pts',(-14.1314791418914,16.2901158858206,-0.742161642599659));
#24389=CARTESIAN_POINT('Ctrl Pts',(-14.5876527612609,17.0802317716412,-0.783828309266326));
#24390=CARTESIAN_POINT('Ctrl Pts',(-15.5,17.0802317716412,-0.825494975932993));
#24391=CARTESIAN_POINT('Ctrl Pts',(-16.4123472387391,17.0802317716412,-0.867161642599661));
#24392=CARTESIAN_POINT('Ctrl Pts',(-16.8685208581086,16.2901158858206,-0.908828309266328));
#24393=CARTESIAN_POINT('Ctrl Pts',(-17.3246944774781,15.5,-0.950494975932995));
#24394=CARTESIAN_POINT('Ctrl Pts',(-16.8685208581086,14.7098841141794,-0.992161642599663));
#24395=CARTESIAN_POINT('Ctrl Pts',(-16.4123472387391,13.9197682283588,-1.03382830926633));
#24396=CARTESIAN_POINT('Ctrl Pts',(-15.5,13.9197682283588,-1.075494975933));
#24397=CARTESIAN_POINT('Ctrl Pts',(-14.5876527612609,13.9197682283588,-1.11716164259966));
#24398=CARTESIAN_POINT('Ctrl Pts',(-14.1314791418914,14.7098841141794,-1.15882830926633));
#24399=CARTESIAN_POINT('Ctrl Pts',(-13.6753055225219,15.5,-1.200494975933));
#24400=CARTESIAN_POINT('Ctrl Pts',(-14.1314791418914,16.2901158858206,-1.24216164259967));
#24401=CARTESIAN_POINT('Ctrl Pts',(-14.5876527612609,17.0802317716412,-1.28382830926633));
#24402=CARTESIAN_POINT('Ctrl Pts',(-15.5,17.0802317716412,-1.325494975933));
#24403=CARTESIAN_POINT('Ctrl Pts',(-16.4123472387391,17.0802317716412,-1.36716164259967));
#24404=CARTESIAN_POINT('Ctrl Pts',(-16.8685208581086,16.2901158858206,-1.40882830926633));
#24405=CARTESIAN_POINT('Ctrl Pts',(-17.3246944774781,15.5,-1.450494975933));
#24406=CARTESIAN_POINT('Ctrl Pts',(-16.8685208581086,14.7098841141794,-1.49216164259967));
#24407=CARTESIAN_POINT('Ctrl Pts',(-16.4123472387391,13.9197682283588,-1.53382830926634));
#24408=CARTESIAN_POINT('Ctrl Pts',(-15.5,13.9197682283588,-1.575494975933));
#24409=CARTESIAN_POINT('Ctrl Pts',(-14.5876527612609,13.9197682283588,-1.61716164259967));
#24410=CARTESIAN_POINT('Ctrl Pts',(-14.1314791418914,14.7098841141794,-1.65882830926634));
#24411=CARTESIAN_POINT('Ctrl Pts',(-13.6753055225219,15.5,-1.70049497593301));
#24412=CARTESIAN_POINT('Ctrl Pts',(-14.1314791418914,16.2901158858206,-1.74216164259967));
#24413=CARTESIAN_POINT('Ctrl Pts',(-14.5876527612609,17.0802317716412,-1.78382830926634));
#24414=CARTESIAN_POINT('Ctrl Pts',(-15.5,17.0802317716412,-1.82549497593301));
#24415=CARTESIAN_POINT('Ctrl Pts',(-16.4123472387391,17.0802317716412,-1.86716164259967));
#24416=CARTESIAN_POINT('Ctrl Pts',(-16.8685208581086,16.2901158858206,-1.90882830926634));
#24417=CARTESIAN_POINT('Ctrl Pts',(-17.3246944774781,15.5,-1.95049497593301));
#24418=CARTESIAN_POINT('Ctrl Pts',(-16.8685208581086,14.7098841141794,-1.99216164259968));
#24419=CARTESIAN_POINT('Ctrl Pts',(-16.7005726719216,14.4189893226644,-2.00750194461187));
#24420=CARTESIAN_POINT('Ctrl Pts',(-16.4288249477777,14.2215569357652,-2.02511838079831));
#24421=CARTESIAN_POINT('Ctrl Pts',(-15.5,17.4320632938683,10.971375));
#24422=CARTESIAN_POINT('Ctrl Pts',(-16.6154772628062,17.4320632938683,10.9297083333333));
#24423=CARTESIAN_POINT('Ctrl Pts',(-17.1732158942094,16.4660316469341,10.8880416666667));
#24424=CARTESIAN_POINT('Ctrl Pts',(-17.7309545256125,15.5,10.846375));
#24425=CARTESIAN_POINT('Ctrl Pts',(-17.1732158942094,14.5339683530659,10.8047083333333));
#24426=CARTESIAN_POINT('Ctrl Pts',(-16.6154772628062,13.5679367061317,10.7630416666667));
#24427=CARTESIAN_POINT('Ctrl Pts',(-15.5,13.5679367061317,10.721375));
#24428=CARTESIAN_POINT('Ctrl Pts',(-14.3845227371938,13.5679367061317,10.6797083333333));
#24429=CARTESIAN_POINT('Ctrl Pts',(-13.8267841057906,14.5339683530659,10.6380416666667));
#24430=CARTESIAN_POINT('Ctrl Pts',(-13.2690454743875,15.5,10.596375));
#24431=CARTESIAN_POINT('Ctrl Pts',(-13.8267841057906,16.4660316469341,10.5547083333333));
#24432=CARTESIAN_POINT('Ctrl Pts',(-14.3845227371938,17.4320632938683,10.5130416666667));
#24433=CARTESIAN_POINT('Ctrl Pts',(-15.5,17.4320632938683,10.471375));
#24434=CARTESIAN_POINT('Ctrl Pts',(-16.6154772628062,17.4320632938683,10.4297083333333));
#24435=CARTESIAN_POINT('Ctrl Pts',(-17.1732158942094,16.4660316469341,10.3880416666667));
#24436=CARTESIAN_POINT('Ctrl Pts',(-17.7309545256125,15.5,10.346375));
#24437=CARTESIAN_POINT('Ctrl Pts',(-17.1732158942094,14.5339683530659,10.3047083333333));
#24438=CARTESIAN_POINT('Ctrl Pts',(-16.6154772628062,13.5679367061317,10.2630416666667));
#24439=CARTESIAN_POINT('Ctrl Pts',(-15.5,13.5679367061317,10.221375));
#24440=CARTESIAN_POINT('Ctrl Pts',(-14.3845227371938,13.5679367061317,10.1797083333333));
#24441=CARTESIAN_POINT('Ctrl Pts',(-13.8267841057906,14.5339683530659,10.1380416666667));
#24442=CARTESIAN_POINT('Ctrl Pts',(-13.2690454743875,15.5,10.096375));
#24443=CARTESIAN_POINT('Ctrl Pts',(-13.8267841057906,16.4660316469341,10.0547083333333));
#24444=CARTESIAN_POINT('Ctrl Pts',(-14.3845227371938,17.4320632938683,10.0130416666666));
#24445=CARTESIAN_POINT('Ctrl Pts',(-15.5,17.4320632938683,9.97137499999998));
#24446=CARTESIAN_POINT('Ctrl Pts',(-16.6154772628062,17.4320632938683,9.92970833333332));
#24447=CARTESIAN_POINT('Ctrl Pts',(-17.1732158942094,16.4660316469341,9.88804166666665));
#24448=CARTESIAN_POINT('Ctrl Pts',(-17.7309545256125,15.5,9.84637499999998));
#24449=CARTESIAN_POINT('Ctrl Pts',(-17.1732158942094,14.5339683530659,9.80470833333331));
#24450=CARTESIAN_POINT('Ctrl Pts',(-16.6154772628062,13.5679367061317,9.76304166666665));
#24451=CARTESIAN_POINT('Ctrl Pts',(-15.5,13.5679367061317,9.72137499999998));
#24452=CARTESIAN_POINT('Ctrl Pts',(-14.3845227371938,13.5679367061317,9.67970833333331));
#24453=CARTESIAN_POINT('Ctrl Pts',(-13.8267841057906,14.5339683530659,9.63804166666664));
#24454=CARTESIAN_POINT('Ctrl Pts',(-13.2690454743875,15.5,9.59637499999998));
#24455=CARTESIAN_POINT('Ctrl Pts',(-13.8267841057906,16.4660316469341,9.55470833333331));
#24456=CARTESIAN_POINT('Ctrl Pts',(-14.3845227371938,17.4320632938683,9.51304166666664));
#24457=CARTESIAN_POINT('Ctrl Pts',(-15.5,17.4320632938683,9.47137499999998));
#24458=CARTESIAN_POINT('Ctrl Pts',(-16.6154772628062,17.4320632938683,9.42970833333331));
#24459=CARTESIAN_POINT('Ctrl Pts',(-17.1732158942094,16.4660316469341,9.38804166666664));
#24460=CARTESIAN_POINT('Ctrl Pts',(-17.7309545256125,15.5,9.34637499999997));
#24461=CARTESIAN_POINT('Ctrl Pts',(-17.1732158942094,14.5339683530659,9.30470833333331));
#24462=CARTESIAN_POINT('Ctrl Pts',(-16.6154772628062,13.5679367061317,9.26304166666664));
#24463=CARTESIAN_POINT('Ctrl Pts',(-15.5,13.5679367061317,9.22137499999997));
#24464=CARTESIAN_POINT('Ctrl Pts',(-14.3845227371938,13.5679367061317,9.1797083333333));
#24465=CARTESIAN_POINT('Ctrl Pts',(-13.8267841057906,14.5339683530659,9.13804166666664));
#24466=CARTESIAN_POINT('Ctrl Pts',(-13.2690454743875,15.5,9.09637499999997));
#24467=CARTESIAN_POINT('Ctrl Pts',(-13.8267841057906,16.4660316469341,9.0547083333333));
#24468=CARTESIAN_POINT('Ctrl Pts',(-14.3845227371938,17.4320632938683,9.01304166666664));
#24469=CARTESIAN_POINT('Ctrl Pts',(-15.5,17.4320632938683,8.97137499999997));
#24470=CARTESIAN_POINT('Ctrl Pts',(-16.6154772628062,17.4320632938683,8.9297083333333));
#24471=CARTESIAN_POINT('Ctrl Pts',(-17.1732158942094,16.4660316469341,8.88804166666663));
#24472=CARTESIAN_POINT('Ctrl Pts',(-17.7309545256125,15.5,8.84637499999997));
#24473=CARTESIAN_POINT('Ctrl Pts',(-17.1732158942094,14.5339683530659,8.8047083333333));
#24474=CARTESIAN_POINT('Ctrl Pts',(-16.6154772628062,13.5679367061317,8.76304166666663));
#24475=CARTESIAN_POINT('Ctrl Pts',(-15.5,13.5679367061317,8.72137499999997));
#24476=CARTESIAN_POINT('Ctrl Pts',(-14.3845227371938,13.5679367061317,8.6797083333333));
#24477=CARTESIAN_POINT('Ctrl Pts',(-13.8267841057906,14.5339683530659,8.63804166666663));
#24478=CARTESIAN_POINT('Ctrl Pts',(-13.2690454743875,15.5,8.59637499999996));
#24479=CARTESIAN_POINT('Ctrl Pts',(-13.8267841057906,16.4660316469341,8.5547083333333));
#24480=CARTESIAN_POINT('Ctrl Pts',(-14.3845227371938,17.4320632938683,8.51304166666663));
#24481=CARTESIAN_POINT('Ctrl Pts',(-15.5,17.4320632938683,8.47137499999996));
#24482=CARTESIAN_POINT('Ctrl Pts',(-16.6154772628062,17.4320632938683,8.42970833333329));
#24483=CARTESIAN_POINT('Ctrl Pts',(-17.1732158942094,16.4660316469341,8.38804166666663));
#24484=CARTESIAN_POINT('Ctrl Pts',(-17.7309545256125,15.5,8.34637499999996));
#24485=CARTESIAN_POINT('Ctrl Pts',(-17.1732158942094,14.5339683530659,8.30470833333329));
#24486=CARTESIAN_POINT('Ctrl Pts',(-16.6154772628062,13.5679367061317,8.26304166666663));
#24487=CARTESIAN_POINT('Ctrl Pts',(-15.5,13.5679367061317,8.22137499999996));
#24488=CARTESIAN_POINT('Ctrl Pts',(-14.3845227371938,13.5679367061317,8.17970833333329));
#24489=CARTESIAN_POINT('Ctrl Pts',(-13.8267841057906,14.5339683530659,8.13804166666662));
#24490=CARTESIAN_POINT('Ctrl Pts',(-13.2690454743875,15.5,8.09637499999996));
#24491=CARTESIAN_POINT('Ctrl Pts',(-13.8267841057906,16.4660316469341,8.05470833333329));
#24492=CARTESIAN_POINT('Ctrl Pts',(-14.3845227371938,17.4320632938683,8.01304166666662));
#24493=CARTESIAN_POINT('Ctrl Pts',(-15.5,17.4320632938683,7.97137499999995));
#24494=CARTESIAN_POINT('Ctrl Pts',(-16.6154772628062,17.4320632938683,7.92970833333329));
#24495=CARTESIAN_POINT('Ctrl Pts',(-17.1732158942094,16.4660316469341,7.88804166666662));
#24496=CARTESIAN_POINT('Ctrl Pts',(-17.7309545256125,15.5,7.84637499999995));
#24497=CARTESIAN_POINT('Ctrl Pts',(-17.1732158942094,14.5339683530659,7.80470833333329));
#24498=CARTESIAN_POINT('Ctrl Pts',(-16.6154772628062,13.5679367061317,7.76304166666662));
#24499=CARTESIAN_POINT('Ctrl Pts',(-15.5,13.5679367061317,7.72137499999995));
#24500=CARTESIAN_POINT('Ctrl Pts',(-14.3845227371938,13.5679367061317,7.67970833333329));
#24501=CARTESIAN_POINT('Ctrl Pts',(-13.8267841057906,14.5339683530659,7.63804166666662));
#24502=CARTESIAN_POINT('Ctrl Pts',(-13.2690454743875,15.5,7.59637499999995));
#24503=CARTESIAN_POINT('Ctrl Pts',(-13.8267841057906,16.4660316469341,7.55470833333328));
#24504=CARTESIAN_POINT('Ctrl Pts',(-14.3845227371938,17.4320632938683,7.51304166666662));
#24505=CARTESIAN_POINT('Ctrl Pts',(-15.5,17.4320632938683,7.47137499999995));
#24506=CARTESIAN_POINT('Ctrl Pts',(-16.6154772628062,17.4320632938683,7.42970833333328));
#24507=CARTESIAN_POINT('Ctrl Pts',(-17.1732158942094,16.4660316469341,7.38804166666661));
#24508=CARTESIAN_POINT('Ctrl Pts',(-17.7309545256125,15.5,7.34637499999995));
#24509=CARTESIAN_POINT('Ctrl Pts',(-17.1732158942094,14.5339683530659,7.30470833333328));
#24510=CARTESIAN_POINT('Ctrl Pts',(-16.6154772628062,13.5679367061317,7.26304166666661));
#24511=CARTESIAN_POINT('Ctrl Pts',(-15.5,13.5679367061317,7.22137499999994));
#24512=CARTESIAN_POINT('Ctrl Pts',(-14.3845227371938,13.5679367061317,7.17970833333328));
#24513=CARTESIAN_POINT('Ctrl Pts',(-13.8267841057906,14.5339683530659,7.13804166666661));
#24514=CARTESIAN_POINT('Ctrl Pts',(-13.2690454743875,15.5,7.09637499999995));
#24515=CARTESIAN_POINT('Ctrl Pts',(-13.8267841057906,16.4660316469341,7.05470833333328));
#24516=CARTESIAN_POINT('Ctrl Pts',(-14.3845227371938,17.4320632938683,7.01304166666661));
#24517=CARTESIAN_POINT('Ctrl Pts',(-15.5,17.4320632938683,6.97137499999994));
#24518=CARTESIAN_POINT('Ctrl Pts',(-16.6154772628062,17.4320632938683,6.92970833333328));
#24519=CARTESIAN_POINT('Ctrl Pts',(-17.1732158942094,16.4660316469341,6.88804166666661));
#24520=CARTESIAN_POINT('Ctrl Pts',(-17.7309545256125,15.5,6.84637499999994));
#24521=CARTESIAN_POINT('Ctrl Pts',(-17.1732158942094,14.5339683530659,6.80470833333327));
#24522=CARTESIAN_POINT('Ctrl Pts',(-16.6154772628062,13.5679367061317,6.76304166666661));
#24523=CARTESIAN_POINT('Ctrl Pts',(-15.5,13.5679367061317,6.72137499999994));
#24524=CARTESIAN_POINT('Ctrl Pts',(-14.3845227371938,13.5679367061317,6.67970833333327));
#24525=CARTESIAN_POINT('Ctrl Pts',(-13.8267841057906,14.5339683530659,6.6380416666666));
#24526=CARTESIAN_POINT('Ctrl Pts',(-13.2690454743875,15.5,6.59637499999994));
#24527=CARTESIAN_POINT('Ctrl Pts',(-13.8267841057906,16.4660316469341,6.55470833333327));
#24528=CARTESIAN_POINT('Ctrl Pts',(-14.3845227371938,17.4320632938683,6.5130416666666));
#24529=CARTESIAN_POINT('Ctrl Pts',(-15.5,17.4320632938683,6.47137499999994));
#24530=CARTESIAN_POINT('Ctrl Pts',(-16.6154772628062,17.4320632938683,6.42970833333327));
#24531=CARTESIAN_POINT('Ctrl Pts',(-17.1732158942094,16.4660316469341,6.3880416666666));
#24532=CARTESIAN_POINT('Ctrl Pts',(-17.7309545256125,15.5,6.34637499999993));
#24533=CARTESIAN_POINT('Ctrl Pts',(-17.1732158942094,14.5339683530659,6.30470833333327));
#24534=CARTESIAN_POINT('Ctrl Pts',(-16.6154772628062,13.5679367061317,6.2630416666666));
#24535=CARTESIAN_POINT('Ctrl Pts',(-15.5,13.5679367061317,6.22137499999993));
#24536=CARTESIAN_POINT('Ctrl Pts',(-14.3845227371938,13.5679367061317,6.17970833333327));
#24537=CARTESIAN_POINT('Ctrl Pts',(-13.8267841057906,14.5339683530659,6.1380416666666));
#24538=CARTESIAN_POINT('Ctrl Pts',(-13.2690454743875,15.5,6.09637499999993));
#24539=CARTESIAN_POINT('Ctrl Pts',(-13.8267841057906,16.4660316469341,6.05470833333326));
#24540=CARTESIAN_POINT('Ctrl Pts',(-14.3845227371938,17.4320632938683,6.0130416666666));
#24541=CARTESIAN_POINT('Ctrl Pts',(-15.5,17.4320632938683,5.97137499999993));
#24542=CARTESIAN_POINT('Ctrl Pts',(-16.6154772628062,17.4320632938683,5.92970833333326));
#24543=CARTESIAN_POINT('Ctrl Pts',(-17.1732158942094,16.4660316469341,5.8880416666666));
#24544=CARTESIAN_POINT('Ctrl Pts',(-17.7309545256125,15.5,5.84637499999993));
#24545=CARTESIAN_POINT('Ctrl Pts',(-17.1732158942094,14.5339683530659,5.80470833333326));
#24546=CARTESIAN_POINT('Ctrl Pts',(-16.6154772628062,13.5679367061317,5.76304166666659));
#24547=CARTESIAN_POINT('Ctrl Pts',(-15.5,13.5679367061317,5.72137499999993));
#24548=CARTESIAN_POINT('Ctrl Pts',(-14.3845227371938,13.5679367061317,5.67970833333326));
#24549=CARTESIAN_POINT('Ctrl Pts',(-13.8267841057906,14.5339683530659,5.63804166666659));
#24550=CARTESIAN_POINT('Ctrl Pts',(-13.2690454743875,15.5,5.59637499999992));
#24551=CARTESIAN_POINT('Ctrl Pts',(-13.8267841057906,16.4660316469341,5.55470833333326));
#24552=CARTESIAN_POINT('Ctrl Pts',(-14.3845227371938,17.4320632938683,5.51304166666659));
#24553=CARTESIAN_POINT('Ctrl Pts',(-15.5,17.4320632938683,5.47137499999992));
#24554=CARTESIAN_POINT('Ctrl Pts',(-16.6154772628062,17.4320632938683,5.42970833333325));
#24555=CARTESIAN_POINT('Ctrl Pts',(-17.1732158942094,16.4660316469341,5.38804166666659));
#24556=CARTESIAN_POINT('Ctrl Pts',(-17.7309545256125,15.5,5.34637499999992));
#24557=CARTESIAN_POINT('Ctrl Pts',(-17.1732158942094,14.5339683530659,5.30470833333325));
#24558=CARTESIAN_POINT('Ctrl Pts',(-16.6154772628062,13.5679367061317,5.26304166666659));
#24559=CARTESIAN_POINT('Ctrl Pts',(-15.5,13.5679367061317,5.22137499999992));
#24560=CARTESIAN_POINT('Ctrl Pts',(-14.3845227371938,13.5679367061317,5.17970833333325));
#24561=CARTESIAN_POINT('Ctrl Pts',(-13.8267841057906,14.5339683530659,5.13804166666659));
#24562=CARTESIAN_POINT('Ctrl Pts',(-13.2690454743875,15.5,5.09637499999992));
#24563=CARTESIAN_POINT('Ctrl Pts',(-13.8267841057906,16.4660316469341,5.05470833333325));
#24564=CARTESIAN_POINT('Ctrl Pts',(-14.3845227371938,17.4320632938683,5.01304166666658));
#24565=CARTESIAN_POINT('Ctrl Pts',(-15.5,17.4320632938683,4.97137499999991));
#24566=CARTESIAN_POINT('Ctrl Pts',(-16.6154772628062,17.4320632938683,4.92970833333325));
#24567=CARTESIAN_POINT('Ctrl Pts',(-17.1732158942094,16.4660316469341,4.88804166666658));
#24568=CARTESIAN_POINT('Ctrl Pts',(-17.7309545256125,15.5,4.84637499999991));
#24569=CARTESIAN_POINT('Ctrl Pts',(-17.1732158942094,14.5339683530659,4.80470833333325));
#24570=CARTESIAN_POINT('Ctrl Pts',(-16.6154772628062,13.5679367061317,4.76304166666658));
#24571=CARTESIAN_POINT('Ctrl Pts',(-15.5,13.5679367061317,4.72137499999991));
#24572=CARTESIAN_POINT('Ctrl Pts',(-14.3845227371938,13.5679367061317,4.67970833333325));
#24573=CARTESIAN_POINT('Ctrl Pts',(-13.8267841057906,14.5339683530659,4.63804166666658));
#24574=CARTESIAN_POINT('Ctrl Pts',(-13.2690454743875,15.5,4.59637499999991));
#24575=CARTESIAN_POINT('Ctrl Pts',(-13.8267841057906,16.4660316469341,4.55470833333324));
#24576=CARTESIAN_POINT('Ctrl Pts',(-14.3845227371938,17.4320632938683,4.51304166666658));
#24577=CARTESIAN_POINT('Ctrl Pts',(-15.5,17.4320632938683,4.47137499999991));
#24578=CARTESIAN_POINT('Ctrl Pts',(-16.6154772628062,17.4320632938683,4.42970833333324));
#24579=CARTESIAN_POINT('Ctrl Pts',(-17.1732158942094,16.4660316469341,4.38804166666657));
#24580=CARTESIAN_POINT('Ctrl Pts',(-17.7309545256125,15.5,4.34637499999991));
#24581=CARTESIAN_POINT('Ctrl Pts',(-17.1732158942094,14.5339683530659,4.30470833333324));
#24582=CARTESIAN_POINT('Ctrl Pts',(-16.6154772628062,13.5679367061317,4.26304166666657));
#24583=CARTESIAN_POINT('Ctrl Pts',(-15.5,13.5679367061317,4.22137499999991));
#24584=CARTESIAN_POINT('Ctrl Pts',(-14.3845227371938,13.5679367061317,4.17970833333324));
#24585=CARTESIAN_POINT('Ctrl Pts',(-13.8267841057906,14.5339683530659,4.13804166666657));
#24586=CARTESIAN_POINT('Ctrl Pts',(-13.2690454743875,15.5,4.0963749999999));
#24587=CARTESIAN_POINT('Ctrl Pts',(-13.8267841057906,16.4660316469341,4.05470833333324));
#24588=CARTESIAN_POINT('Ctrl Pts',(-14.3845227371938,17.4320632938683,4.01304166666657));
#24589=CARTESIAN_POINT('Ctrl Pts',(-15.5,17.4320632938683,3.9713749999999));
#24590=CARTESIAN_POINT('Ctrl Pts',(-16.6154772628062,17.4320632938683,3.92970833333323));
#24591=CARTESIAN_POINT('Ctrl Pts',(-17.1732158942094,16.4660316469341,3.88804166666657));
#24592=CARTESIAN_POINT('Ctrl Pts',(-17.7309545256125,15.5,3.8463749999999));
#24593=CARTESIAN_POINT('Ctrl Pts',(-17.1732158942094,14.5339683530659,3.80470833333323));
#24594=CARTESIAN_POINT('Ctrl Pts',(-16.6154772628062,13.5679367061317,3.76304166666656));
#24595=CARTESIAN_POINT('Ctrl Pts',(-15.5,13.5679367061317,3.7213749999999));
#24596=CARTESIAN_POINT('Ctrl Pts',(-14.3845227371938,13.5679367061317,3.67970833333323));
#24597=CARTESIAN_POINT('Ctrl Pts',(-13.8267841057906,14.5339683530659,3.63804166666656));
#24598=CARTESIAN_POINT('Ctrl Pts',(-13.2690454743875,15.5,3.5963749999999));
#24599=CARTESIAN_POINT('Ctrl Pts',(-13.8267841057906,16.4660316469341,3.55470833333323));
#24600=CARTESIAN_POINT('Ctrl Pts',(-14.3845227371938,17.4320632938683,3.51304166666656));
#24601=CARTESIAN_POINT('Ctrl Pts',(-15.5,17.4320632938683,3.4713749999999));
#24602=CARTESIAN_POINT('Ctrl Pts',(-16.6154772628062,17.4320632938683,3.42970833333323));
#24603=CARTESIAN_POINT('Ctrl Pts',(-17.1732158942094,16.4660316469341,3.38804166666656));
#24604=CARTESIAN_POINT('Ctrl Pts',(-17.7309545256125,15.5,3.34637499999989));
#24605=CARTESIAN_POINT('Ctrl Pts',(-17.1732158942094,14.5339683530659,3.30470833333323));
#24606=CARTESIAN_POINT('Ctrl Pts',(-16.6154772628062,13.5679367061317,3.26304166666656));
#24607=CARTESIAN_POINT('Ctrl Pts',(-15.5,13.5679367061317,3.22137499999989));
#24608=CARTESIAN_POINT('Ctrl Pts',(-14.3845227371938,13.5679367061317,3.17970833333322));
#24609=CARTESIAN_POINT('Ctrl Pts',(-13.8267841057906,14.5339683530659,3.13804166666656));
#24610=CARTESIAN_POINT('Ctrl Pts',(-13.2690454743875,15.5,3.09637499999989));
#24611=CARTESIAN_POINT('Ctrl Pts',(-13.8267841057906,16.4660316469341,3.05470833333322));
#24612=CARTESIAN_POINT('Ctrl Pts',(-14.3845227371938,17.4320632938683,3.01304166666656));
#24613=CARTESIAN_POINT('Ctrl Pts',(-15.5,17.4320632938683,2.97137499999989));
#24614=CARTESIAN_POINT('Ctrl Pts',(-16.6154772628062,17.4320632938683,2.92970833333322));
#24615=CARTESIAN_POINT('Ctrl Pts',(-17.1732158942094,16.4660316469341,2.88804166666655));
#24616=CARTESIAN_POINT('Ctrl Pts',(-17.7309545256125,15.5,2.84637499999989));
#24617=CARTESIAN_POINT('Ctrl Pts',(-17.1732158942094,14.5339683530659,2.80470833333322));
#24618=CARTESIAN_POINT('Ctrl Pts',(-16.6154772628062,13.5679367061317,2.76304166666655));
#24619=CARTESIAN_POINT('Ctrl Pts',(-15.5,13.5679367061317,2.72137499999989));
#24620=CARTESIAN_POINT('Ctrl Pts',(-14.3845227371938,13.5679367061317,2.67970833333322));
#24621=CARTESIAN_POINT('Ctrl Pts',(-13.8267841057906,14.5339683530659,2.63804166666655));
#24622=CARTESIAN_POINT('Ctrl Pts',(-13.2690454743875,15.5,2.59637499999988));
#24623=CARTESIAN_POINT('Ctrl Pts',(-13.8267841057906,16.4660316469341,2.55470833333322));
#24624=CARTESIAN_POINT('Ctrl Pts',(-14.3845227371938,17.4320632938683,2.51304166666655));
#24625=CARTESIAN_POINT('Ctrl Pts',(-15.5,17.4320632938683,2.47137499999988));
#24626=CARTESIAN_POINT('Ctrl Pts',(-16.6154772628062,17.4320632938683,2.42970833333321));
#24627=CARTESIAN_POINT('Ctrl Pts',(-17.1732158942094,16.4660316469341,2.38804166666655));
#24628=CARTESIAN_POINT('Ctrl Pts',(-17.7309545256125,15.5,2.34637499999988));
#24629=CARTESIAN_POINT('Ctrl Pts',(-17.1732158942094,14.5339683530659,2.30470833333321));
#24630=CARTESIAN_POINT('Ctrl Pts',(-16.6154772628062,13.5679367061317,2.26304166666655));
#24631=CARTESIAN_POINT('Ctrl Pts',(-15.5,13.5679367061317,2.22137499999988));
#24632=CARTESIAN_POINT('Ctrl Pts',(-14.3845227371938,13.5679367061317,2.17970833333321));
#24633=CARTESIAN_POINT('Ctrl Pts',(-13.8267841057906,14.5339683530659,2.13804166666654));
#24634=CARTESIAN_POINT('Ctrl Pts',(-13.2690454743875,15.5,2.09637499999988));
#24635=CARTESIAN_POINT('Ctrl Pts',(-13.8267841057906,16.4660316469341,2.05470833333321));
#24636=CARTESIAN_POINT('Ctrl Pts',(-14.3845227371938,17.4320632938683,2.01304166666654));
#24637=CARTESIAN_POINT('Ctrl Pts',(-15.5,17.4320632938683,1.97137499999988));
#24638=CARTESIAN_POINT('Ctrl Pts',(-16.6154772628062,17.4320632938683,1.92970833333321));
#24639=CARTESIAN_POINT('Ctrl Pts',(-17.1732158942094,16.4660316469341,1.88804166666654));
#24640=CARTESIAN_POINT('Ctrl Pts',(-17.7309545256125,15.5,1.84637499999987));
#24641=CARTESIAN_POINT('Ctrl Pts',(-17.1732158942094,14.5339683530659,1.80470833333321));
#24642=CARTESIAN_POINT('Ctrl Pts',(-16.6154772628062,13.5679367061317,1.76304166666654));
#24643=CARTESIAN_POINT('Ctrl Pts',(-15.5,13.5679367061317,1.72137499999987));
#24644=CARTESIAN_POINT('Ctrl Pts',(-14.3845227371938,13.5679367061317,1.67970833333321));
#24645=CARTESIAN_POINT('Ctrl Pts',(-13.8267841057906,14.5339683530659,1.63804166666654));
#24646=CARTESIAN_POINT('Ctrl Pts',(-13.2690454743875,15.5,1.59637499999987));
#24647=CARTESIAN_POINT('Ctrl Pts',(-13.8267841057906,16.4660316469341,1.5547083333332));
#24648=CARTESIAN_POINT('Ctrl Pts',(-14.3845227371938,17.4320632938683,1.51304166666654));
#24649=CARTESIAN_POINT('Ctrl Pts',(-15.5,17.4320632938683,1.47137499999987));
#24650=CARTESIAN_POINT('Ctrl Pts',(-16.6154772628062,17.4320632938683,1.4297083333332));
#24651=CARTESIAN_POINT('Ctrl Pts',(-17.1732158942094,16.4660316469341,1.38804166666653));
#24652=CARTESIAN_POINT('Ctrl Pts',(-17.7309545256125,15.5,1.34637499999987));
#24653=CARTESIAN_POINT('Ctrl Pts',(-17.1732158942094,14.5339683530659,1.3047083333332));
#24654=CARTESIAN_POINT('Ctrl Pts',(-16.6154772628062,13.5679367061317,1.26304166666653));
#24655=CARTESIAN_POINT('Ctrl Pts',(-15.5,13.5679367061317,1.22137499999987));
#24656=CARTESIAN_POINT('Ctrl Pts',(-14.3845227371938,13.5679367061317,1.1797083333332));
#24657=CARTESIAN_POINT('Ctrl Pts',(-13.8267841057906,14.5339683530659,1.13804166666653));
#24658=CARTESIAN_POINT('Ctrl Pts',(-13.2690454743875,15.5,1.09637499999986));
#24659=CARTESIAN_POINT('Ctrl Pts',(-13.8267841057906,16.4660316469341,1.0547083333332));
#24660=CARTESIAN_POINT('Ctrl Pts',(-14.3845227371938,17.4320632938683,1.01304166666653));
#24661=CARTESIAN_POINT('Ctrl Pts',(-15.5,17.4320632938683,0.971374999999861));
#24662=CARTESIAN_POINT('Ctrl Pts',(-16.6154772628062,17.4320632938683,0.929708333333194));
#24663=CARTESIAN_POINT('Ctrl Pts',(-17.1732158942094,16.4660316469341,0.888041666666528));
#24664=CARTESIAN_POINT('Ctrl Pts',(-17.7309545256125,15.5,0.846374999999861));
#24665=CARTESIAN_POINT('Ctrl Pts',(-17.1732158942094,14.5339683530659,0.804708333333194));
#24666=CARTESIAN_POINT('Ctrl Pts',(-16.6154772628062,13.5679367061317,0.763041666666526));
#24667=CARTESIAN_POINT('Ctrl Pts',(-15.5,13.5679367061317,0.721374999999859));
#24668=CARTESIAN_POINT('Ctrl Pts',(-14.3845227371938,13.5679367061317,0.679708333333192));
#24669=CARTESIAN_POINT('Ctrl Pts',(-13.8267841057906,14.5339683530659,0.638041666666525));
#24670=CARTESIAN_POINT('Ctrl Pts',(-13.2690454743875,15.5,0.596374999999858));
#24671=CARTESIAN_POINT('Ctrl Pts',(-13.8267841057906,16.4660316469341,0.55470833333319));
#24672=CARTESIAN_POINT('Ctrl Pts',(-14.3845227371938,17.4320632938683,0.513041666666523));
#24673=CARTESIAN_POINT('Ctrl Pts',(-15.5,17.4320632938683,0.471374999999856));
#24674=CARTESIAN_POINT('Ctrl Pts',(-16.6154772628062,17.4320632938683,0.429708333333188));
#24675=CARTESIAN_POINT('Ctrl Pts',(-17.1732158942094,16.4660316469341,0.388041666666521));
#24676=CARTESIAN_POINT('Ctrl Pts',(-17.7309545256125,15.5,0.346374999999854));
#24677=CARTESIAN_POINT('Ctrl Pts',(-17.1732158942094,14.5339683530659,0.304708333333186));
#24678=CARTESIAN_POINT('Ctrl Pts',(-16.6154772628062,13.5679367061317,0.263041666666519));
#24679=CARTESIAN_POINT('Ctrl Pts',(-15.5,13.5679367061317,0.221374999999852));
#24680=CARTESIAN_POINT('Ctrl Pts',(-14.3845227371938,13.5679367061317,0.179708333333185));
#24681=CARTESIAN_POINT('Ctrl Pts',(-13.8267841057906,14.5339683530659,0.138041666666517));
#24682=CARTESIAN_POINT('Ctrl Pts',(-13.2690454743875,15.5,0.0963749999998501));
#24683=CARTESIAN_POINT('Ctrl Pts',(-13.8267841057906,16.4660316469341,0.0547083333331828));
#24684=CARTESIAN_POINT('Ctrl Pts',(-14.3845227371938,17.4320632938683,0.0130416666665155));
#24685=CARTESIAN_POINT('Ctrl Pts',(-15.5,17.4320632938683,-0.0286250000001518));
#24686=CARTESIAN_POINT('Ctrl Pts',(-16.6154772628062,17.4320632938683,-0.0702916666668191));
#24687=CARTESIAN_POINT('Ctrl Pts',(-17.1732158942094,16.4660316469341,-0.111958333333486));
#24688=CARTESIAN_POINT('Ctrl Pts',(-17.7309545256125,15.5,-0.153625000000154));
#24689=CARTESIAN_POINT('Ctrl Pts',(-17.1732158942094,14.5339683530659,-0.195291666666821));
#24690=CARTESIAN_POINT('Ctrl Pts',(-16.6154772628062,13.5679367061317,-0.236958333333488));
#24691=CARTESIAN_POINT('Ctrl Pts',(-15.5,13.5679367061317,-0.278625000000155));
#24692=CARTESIAN_POINT('Ctrl Pts',(-14.3845227371938,13.5679367061317,-0.320291666666821));
#24693=CARTESIAN_POINT('Ctrl Pts',(-13.8267841057906,14.5339683530659,-0.361958333333488));
#24694=CARTESIAN_POINT('Ctrl Pts',(-13.2690454743875,15.5,-0.403625000000156));
#24695=CARTESIAN_POINT('Ctrl Pts',(-13.8267841057906,16.4660316469341,-0.445291666666823));
#24696=CARTESIAN_POINT('Ctrl Pts',(-14.3845227371938,17.4320632938683,-0.48695833333349));
#24697=CARTESIAN_POINT('Ctrl Pts',(-15.5,17.4320632938683,-0.528625000000157));
#24698=CARTESIAN_POINT('Ctrl Pts',(-16.6154772628062,17.4320632938683,-0.570291666666825));
#24699=CARTESIAN_POINT('Ctrl Pts',(-17.1732158942094,16.4660316469341,-0.611958333333492));
#24700=CARTESIAN_POINT('Ctrl Pts',(-17.7309545256125,15.5,-0.653625000000159));
#24701=CARTESIAN_POINT('Ctrl Pts',(-17.1732158942094,14.5339683530659,-0.695291666666827));
#24702=CARTESIAN_POINT('Ctrl Pts',(-16.6154772628062,13.5679367061317,-0.736958333333494));
#24703=CARTESIAN_POINT('Ctrl Pts',(-15.5,13.5679367061317,-0.778625000000161));
#24704=CARTESIAN_POINT('Ctrl Pts',(-14.3845227371938,13.5679367061317,-0.820291666666829));
#24705=CARTESIAN_POINT('Ctrl Pts',(-13.8267841057906,14.5339683530659,-0.861958333333496));
#24706=CARTESIAN_POINT('Ctrl Pts',(-13.2690454743875,15.5,-0.903625000000163));
#24707=CARTESIAN_POINT('Ctrl Pts',(-13.8267841057906,16.4660316469341,-0.94529166666683));
#24708=CARTESIAN_POINT('Ctrl Pts',(-14.3845227371938,17.4320632938683,-0.986958333333498));
#24709=CARTESIAN_POINT('Ctrl Pts',(-15.5,17.4320632938683,-1.02862500000016));
#24710=CARTESIAN_POINT('Ctrl Pts',(-16.6154772628062,17.4320632938683,-1.07029166666683));
#24711=CARTESIAN_POINT('Ctrl Pts',(-17.1732158942094,16.4660316469341,-1.1119583333335));
#24712=CARTESIAN_POINT('Ctrl Pts',(-17.7309545256125,15.5,-1.15362500000017));
#24713=CARTESIAN_POINT('Ctrl Pts',(-17.1732158942094,14.5339683530659,-1.19529166666683));
#24714=CARTESIAN_POINT('Ctrl Pts',(-16.6154772628062,13.5679367061317,-1.2369583333335));
#24715=CARTESIAN_POINT('Ctrl Pts',(-15.5,13.5679367061317,-1.27862500000017));
#24716=CARTESIAN_POINT('Ctrl Pts',(-14.3845227371938,13.5679367061317,-1.32029166666684));
#24717=CARTESIAN_POINT('Ctrl Pts',(-13.8267841057906,14.5339683530659,-1.3619583333335));
#24718=CARTESIAN_POINT('Ctrl Pts',(-13.2690454743875,15.5,-1.40362500000017));
#24719=CARTESIAN_POINT('Ctrl Pts',(-13.8267841057906,16.4660316469341,-1.44529166666684));
#24720=CARTESIAN_POINT('Ctrl Pts',(-14.3845227371938,17.4320632938683,-1.4869583333335));
#24721=CARTESIAN_POINT('Ctrl Pts',(-15.5,17.4320632938683,-1.52862500000017));
#24722=CARTESIAN_POINT('Ctrl Pts',(-16.6154772628062,17.4320632938683,-1.57029166666684));
#24723=CARTESIAN_POINT('Ctrl Pts',(-17.1732158942094,16.4660316469341,-1.61195833333351));
#24724=CARTESIAN_POINT('Ctrl Pts',(-17.7309545256125,15.5,-1.65362500000017));
#24725=CARTESIAN_POINT('Ctrl Pts',(-17.1732158942094,14.5339683530659,-1.69529166666684));
#24726=CARTESIAN_POINT('Ctrl Pts',(-16.6154772628062,13.5679367061317,-1.73695833333351));
#24727=CARTESIAN_POINT('Ctrl Pts',(-15.5,13.5679367061317,-1.77862500000017));
#24728=CARTESIAN_POINT('Ctrl Pts',(-14.3845227371938,13.5679367061317,-1.82029166666684));
#24729=CARTESIAN_POINT('Ctrl Pts',(-13.8267841057906,14.5339683530659,-1.86195833333351));
#24730=CARTESIAN_POINT('Ctrl Pts',(-13.2690454743875,15.5,-1.90362500000018));
#24731=CARTESIAN_POINT('Ctrl Pts',(-13.8267841057906,16.4660316469341,-1.94529166666684));
#24732=CARTESIAN_POINT('Ctrl Pts',(-14.3845227371938,17.4320632938683,-1.98695833333351));
#24733=CARTESIAN_POINT('Ctrl Pts',(-15.5,17.4320632938683,-2.02862500000018));
#24734=CARTESIAN_POINT('Ctrl Pts',(-16.6154772628062,17.4320632938683,-2.07029166666685));
#24735=CARTESIAN_POINT('Ctrl Pts',(-17.1732158942094,16.4660316469341,-2.11195833333351));
#24736=CARTESIAN_POINT('Ctrl Pts',(-17.7309545256125,15.5,-2.15362500000018));
#24737=CARTESIAN_POINT('Ctrl Pts',(-17.1732158942094,14.5339683530659,-2.19529166666685));
#24738=CARTESIAN_POINT('Ctrl Pts',(-16.9678747970191,14.1783071398504,-2.21063196867905));
#24739=CARTESIAN_POINT('Ctrl Pts',(-16.6356236599184,13.9369173167914,-2.22824840486548));
#24740=CARTESIAN_POINT('Origin',(-15.5080107655896,15.6430062215135,1.38580563032467));
#24741=CARTESIAN_POINT('',(-16.4288320706156,14.2215513317122,-2.02512305032214));
#24742=CARTESIAN_POINT('Ctrl Pts',(-15.2436450846258,13.9406917842497,10.4122404735808));
#24743=CARTESIAN_POINT('Ctrl Pts',(-14.5054990725557,14.0620451873462,10.3753299573543));
#24744=CARTESIAN_POINT('Ctrl Pts',(-14.1314716057906,14.7098797632096,10.3411666666667));
#24745=CARTESIAN_POINT('Ctrl Pts',(-13.6752954743875,15.5,10.2995));
#24746=CARTESIAN_POINT('Ctrl Pts',(-14.1314716057906,16.2901202367904,10.2578333333333));
#24747=CARTESIAN_POINT('Ctrl Pts',(-14.5876477371938,17.0802404735808,10.2161666666667));
#24748=CARTESIAN_POINT('Ctrl Pts',(-15.5,17.0802404735808,10.1745));
#24749=CARTESIAN_POINT('Ctrl Pts',(-16.4123522628062,17.0802404735808,10.1328333333333));
#24750=CARTESIAN_POINT('Ctrl Pts',(-16.8685283942094,16.2901202367904,10.0911666666667));
#24751=CARTESIAN_POINT('Ctrl Pts',(-17.3247045256125,15.5,10.0495));
#24752=CARTESIAN_POINT('Ctrl Pts',(-16.8685283942094,14.7098797632096,10.0078333333333));
#24753=CARTESIAN_POINT('Ctrl Pts',(-16.4123522628062,13.9197595264192,9.96616666666665));
#24754=CARTESIAN_POINT('Ctrl Pts',(-15.5,13.9197595264192,9.92449999999998));
#24755=CARTESIAN_POINT('Ctrl Pts',(-14.5876477371938,13.9197595264192,9.88283333333331));
#24756=CARTESIAN_POINT('Ctrl Pts',(-14.1314716057906,14.7098797632096,9.84116666666665));
#24757=CARTESIAN_POINT('Ctrl Pts',(-13.6752954743875,15.5,9.79949999999998));
#24758=CARTESIAN_POINT('Ctrl Pts',(-14.1314716057906,16.2901202367904,9.75783333333331));
#24759=CARTESIAN_POINT('Ctrl Pts',(-14.5876477371938,17.0802404735808,9.71616666666665));
#24760=CARTESIAN_POINT('Ctrl Pts',(-15.5,17.0802404735808,9.67449999999998));
#24761=CARTESIAN_POINT('Ctrl Pts',(-16.4123522628062,17.0802404735808,9.63283333333331));
#24762=CARTESIAN_POINT('Ctrl Pts',(-16.8685283942094,16.2901202367904,9.59116666666664));
#24763=CARTESIAN_POINT('Ctrl Pts',(-17.3247045256125,15.5,9.54949999999998));
#24764=CARTESIAN_POINT('Ctrl Pts',(-16.8685283942094,14.7098797632096,9.50783333333331));
#24765=CARTESIAN_POINT('Ctrl Pts',(-16.4123522628062,13.9197595264192,9.46616666666664));
#24766=CARTESIAN_POINT('Ctrl Pts',(-15.5,13.9197595264192,9.42449999999998));
#24767=CARTESIAN_POINT('Ctrl Pts',(-14.5876477371938,13.9197595264192,9.38283333333331));
#24768=CARTESIAN_POINT('Ctrl Pts',(-14.1314716057906,14.7098797632096,9.34116666666664));
#24769=CARTESIAN_POINT('Ctrl Pts',(-13.6752954743875,15.5,9.29949999999997));
#24770=CARTESIAN_POINT('Ctrl Pts',(-14.1314716057906,16.2901202367904,9.25783333333331));
#24771=CARTESIAN_POINT('Ctrl Pts',(-14.5876477371938,17.0802404735808,9.21616666666664));
#24772=CARTESIAN_POINT('Ctrl Pts',(-15.5,17.0802404735808,9.17449999999997));
#24773=CARTESIAN_POINT('Ctrl Pts',(-16.4123522628062,17.0802404735808,9.13283333333331));
#24774=CARTESIAN_POINT('Ctrl Pts',(-16.8685283942094,16.2901202367904,9.09116666666664));
#24775=CARTESIAN_POINT('Ctrl Pts',(-17.3247045256125,15.5,9.04949999999997));
#24776=CARTESIAN_POINT('Ctrl Pts',(-16.8685283942094,14.7098797632096,9.0078333333333));
#24777=CARTESIAN_POINT('Ctrl Pts',(-16.4123522628062,13.9197595264192,8.96616666666664));
#24778=CARTESIAN_POINT('Ctrl Pts',(-15.5,13.9197595264192,8.92449999999997));
#24779=CARTESIAN_POINT('Ctrl Pts',(-14.5876477371938,13.9197595264192,8.8828333333333));
#24780=CARTESIAN_POINT('Ctrl Pts',(-14.1314716057906,14.7098797632096,8.84116666666664));
#24781=CARTESIAN_POINT('Ctrl Pts',(-13.6752954743875,15.5,8.79949999999997));
#24782=CARTESIAN_POINT('Ctrl Pts',(-14.1314716057906,16.2901202367904,8.7578333333333));
#24783=CARTESIAN_POINT('Ctrl Pts',(-14.5876477371938,17.0802404735808,8.71616666666663));
#24784=CARTESIAN_POINT('Ctrl Pts',(-15.5,17.0802404735808,8.67449999999997));
#24785=CARTESIAN_POINT('Ctrl Pts',(-16.4123522628062,17.0802404735808,8.6328333333333));
#24786=CARTESIAN_POINT('Ctrl Pts',(-16.8685283942094,16.2901202367904,8.59116666666663));
#24787=CARTESIAN_POINT('Ctrl Pts',(-17.3247045256125,15.5,8.54949999999996));
#24788=CARTESIAN_POINT('Ctrl Pts',(-16.8685283942094,14.7098797632096,8.50783333333329));
#24789=CARTESIAN_POINT('Ctrl Pts',(-16.4123522628062,13.9197595264192,8.46616666666663));
#24790=CARTESIAN_POINT('Ctrl Pts',(-15.5,13.9197595264192,8.42449999999996));
#24791=CARTESIAN_POINT('Ctrl Pts',(-14.5876477371938,13.9197595264192,8.38283333333329));
#24792=CARTESIAN_POINT('Ctrl Pts',(-14.1314716057906,14.7098797632096,8.34116666666663));
#24793=CARTESIAN_POINT('Ctrl Pts',(-13.6752954743875,15.5,8.29949999999996));
#24794=CARTESIAN_POINT('Ctrl Pts',(-14.1314716057906,16.2901202367904,8.25783333333329));
#24795=CARTESIAN_POINT('Ctrl Pts',(-14.5876477371938,17.0802404735808,8.21616666666663));
#24796=CARTESIAN_POINT('Ctrl Pts',(-15.5,17.0802404735808,8.17449999999996));
#24797=CARTESIAN_POINT('Ctrl Pts',(-16.4123522628062,17.0802404735808,8.13283333333329));
#24798=CARTESIAN_POINT('Ctrl Pts',(-16.8685283942094,16.2901202367904,8.09116666666663));
#24799=CARTESIAN_POINT('Ctrl Pts',(-17.3247045256125,15.5,8.04949999999996));
#24800=CARTESIAN_POINT('Ctrl Pts',(-16.8685283942094,14.7098797632096,8.00783333333329));
#24801=CARTESIAN_POINT('Ctrl Pts',(-16.4123522628062,13.9197595264192,7.96616666666662));
#24802=CARTESIAN_POINT('Ctrl Pts',(-15.5,13.9197595264192,7.92449999999996));
#24803=CARTESIAN_POINT('Ctrl Pts',(-14.5876477371938,13.9197595264192,7.88283333333329));
#24804=CARTESIAN_POINT('Ctrl Pts',(-14.1314716057906,14.7098797632096,7.84116666666662));
#24805=CARTESIAN_POINT('Ctrl Pts',(-13.6752954743875,15.5,7.79949999999995));
#24806=CARTESIAN_POINT('Ctrl Pts',(-14.1314716057906,16.2901202367904,7.75783333333329));
#24807=CARTESIAN_POINT('Ctrl Pts',(-14.5876477371938,17.0802404735808,7.71616666666662));
#24808=CARTESIAN_POINT('Ctrl Pts',(-15.5,17.0802404735808,7.67449999999995));
#24809=CARTESIAN_POINT('Ctrl Pts',(-16.4123522628062,17.0802404735808,7.63283333333328));
#24810=CARTESIAN_POINT('Ctrl Pts',(-16.8685283942094,16.2901202367904,7.59116666666662));
#24811=CARTESIAN_POINT('Ctrl Pts',(-17.3247045256125,15.5,7.54949999999995));
#24812=CARTESIAN_POINT('Ctrl Pts',(-16.8685283942094,14.7098797632096,7.50783333333328));
#24813=CARTESIAN_POINT('Ctrl Pts',(-16.4123522628062,13.9197595264192,7.46616666666662));
#24814=CARTESIAN_POINT('Ctrl Pts',(-15.5,13.9197595264192,7.42449999999995));
#24815=CARTESIAN_POINT('Ctrl Pts',(-14.5876477371938,13.9197595264192,7.38283333333328));
#24816=CARTESIAN_POINT('Ctrl Pts',(-14.1314716057906,14.7098797632096,7.34116666666661));
#24817=CARTESIAN_POINT('Ctrl Pts',(-13.6752954743875,15.5,7.29949999999995));
#24818=CARTESIAN_POINT('Ctrl Pts',(-14.1314716057906,16.2901202367904,7.25783333333328));
#24819=CARTESIAN_POINT('Ctrl Pts',(-14.5876477371938,17.0802404735808,7.21616666666661));
#24820=CARTESIAN_POINT('Ctrl Pts',(-15.5,17.0802404735808,7.17449999999995));
#24821=CARTESIAN_POINT('Ctrl Pts',(-16.4123522628062,17.0802404735808,7.13283333333328));
#24822=CARTESIAN_POINT('Ctrl Pts',(-16.8685283942094,16.2901202367904,7.09116666666661));
#24823=CARTESIAN_POINT('Ctrl Pts',(-17.3247045256125,15.5,7.04949999999994));
#24824=CARTESIAN_POINT('Ctrl Pts',(-16.8685283942094,14.7098797632096,7.00783333333328));
#24825=CARTESIAN_POINT('Ctrl Pts',(-16.4123522628062,13.9197595264192,6.96616666666661));
#24826=CARTESIAN_POINT('Ctrl Pts',(-15.5,13.9197595264192,6.92449999999994));
#24827=CARTESIAN_POINT('Ctrl Pts',(-14.5876477371938,13.9197595264192,6.88283333333327));
#24828=CARTESIAN_POINT('Ctrl Pts',(-14.1314716057906,14.7098797632096,6.84116666666661));
#24829=CARTESIAN_POINT('Ctrl Pts',(-13.6752954743875,15.5,6.79949999999994));
#24830=CARTESIAN_POINT('Ctrl Pts',(-14.1314716057906,16.2901202367904,6.75783333333327));
#24831=CARTESIAN_POINT('Ctrl Pts',(-14.5876477371938,17.0802404735808,6.71616666666661));
#24832=CARTESIAN_POINT('Ctrl Pts',(-15.5,17.0802404735808,6.67449999999994));
#24833=CARTESIAN_POINT('Ctrl Pts',(-16.4123522628062,17.0802404735808,6.63283333333327));
#24834=CARTESIAN_POINT('Ctrl Pts',(-16.8685283942094,16.2901202367904,6.59116666666661));
#24835=CARTESIAN_POINT('Ctrl Pts',(-17.3247045256125,15.5,6.54949999999994));
#24836=CARTESIAN_POINT('Ctrl Pts',(-16.8685283942094,14.7098797632096,6.50783333333327));
#24837=CARTESIAN_POINT('Ctrl Pts',(-16.4123522628062,13.9197595264192,6.4661666666666));
#24838=CARTESIAN_POINT('Ctrl Pts',(-15.5,13.9197595264192,6.42449999999994));
#24839=CARTESIAN_POINT('Ctrl Pts',(-14.5876477371938,13.9197595264192,6.38283333333327));
#24840=CARTESIAN_POINT('Ctrl Pts',(-14.1314716057906,14.7098797632096,6.3411666666666));
#24841=CARTESIAN_POINT('Ctrl Pts',(-13.6752954743875,15.5,6.29949999999993));
#24842=CARTESIAN_POINT('Ctrl Pts',(-14.1314716057906,16.2901202367904,6.25783333333327));
#24843=CARTESIAN_POINT('Ctrl Pts',(-14.5876477371938,17.0802404735808,6.2161666666666));
#24844=CARTESIAN_POINT('Ctrl Pts',(-15.5,17.0802404735808,6.17449999999993));
#24845=CARTESIAN_POINT('Ctrl Pts',(-16.4123522628062,17.0802404735808,6.13283333333326));
#24846=CARTESIAN_POINT('Ctrl Pts',(-16.8685283942094,16.2901202367904,6.0911666666666));
#24847=CARTESIAN_POINT('Ctrl Pts',(-17.3247045256125,15.5,6.04949999999993));
#24848=CARTESIAN_POINT('Ctrl Pts',(-16.8685283942094,14.7098797632096,6.00783333333326));
#24849=CARTESIAN_POINT('Ctrl Pts',(-16.4123522628062,13.9197595264192,5.9661666666666));
#24850=CARTESIAN_POINT('Ctrl Pts',(-15.5,13.9197595264192,5.92449999999993));
#24851=CARTESIAN_POINT('Ctrl Pts',(-14.5876477371938,13.9197595264192,5.88283333333326));
#24852=CARTESIAN_POINT('Ctrl Pts',(-14.1314716057906,14.7098797632096,5.8411666666666));
#24853=CARTESIAN_POINT('Ctrl Pts',(-13.6752954743875,15.5,5.79949999999993));
#24854=CARTESIAN_POINT('Ctrl Pts',(-14.1314716057906,16.2901202367904,5.75783333333326));
#24855=CARTESIAN_POINT('Ctrl Pts',(-14.5876477371938,17.0802404735808,5.71616666666659));
#24856=CARTESIAN_POINT('Ctrl Pts',(-15.5,17.0802404735808,5.67449999999993));
#24857=CARTESIAN_POINT('Ctrl Pts',(-16.4123522628062,17.0802404735808,5.63283333333326));
#24858=CARTESIAN_POINT('Ctrl Pts',(-16.8685283942094,16.2901202367904,5.59116666666659));
#24859=CARTESIAN_POINT('Ctrl Pts',(-17.3247045256125,15.5,5.54949999999992));
#24860=CARTESIAN_POINT('Ctrl Pts',(-16.8685283942094,14.7098797632096,5.50783333333326));
#24861=CARTESIAN_POINT('Ctrl Pts',(-16.4123522628062,13.9197595264192,5.46616666666659));
#24862=CARTESIAN_POINT('Ctrl Pts',(-15.5,13.9197595264192,5.42449999999992));
#24863=CARTESIAN_POINT('Ctrl Pts',(-14.5876477371938,13.9197595264192,5.38283333333326));
#24864=CARTESIAN_POINT('Ctrl Pts',(-14.1314716057906,14.7098797632096,5.34116666666659));
#24865=CARTESIAN_POINT('Ctrl Pts',(-13.6752954743875,15.5,5.29949999999992));
#24866=CARTESIAN_POINT('Ctrl Pts',(-14.1314716057906,16.2901202367904,5.25783333333325));
#24867=CARTESIAN_POINT('Ctrl Pts',(-14.5876477371938,17.0802404735808,5.21616666666659));
#24868=CARTESIAN_POINT('Ctrl Pts',(-15.5,17.0802404735808,5.17449999999992));
#24869=CARTESIAN_POINT('Ctrl Pts',(-16.4123522628062,17.0802404735808,5.13283333333325));
#24870=CARTESIAN_POINT('Ctrl Pts',(-16.8685283942094,16.2901202367904,5.09116666666658));
#24871=CARTESIAN_POINT('Ctrl Pts',(-17.3247045256125,15.5,5.04949999999992));
#24872=CARTESIAN_POINT('Ctrl Pts',(-16.8685283942094,14.7098797632096,5.00783333333325));
#24873=CARTESIAN_POINT('Ctrl Pts',(-16.4123522628062,13.9197595264192,4.96616666666658));
#24874=CARTESIAN_POINT('Ctrl Pts',(-15.5,13.9197595264192,4.92449999999992));
#24875=CARTESIAN_POINT('Ctrl Pts',(-14.5876477371938,13.9197595264192,4.88283333333325));
#24876=CARTESIAN_POINT('Ctrl Pts',(-14.1314716057906,14.7098797632096,4.84116666666658));
#24877=CARTESIAN_POINT('Ctrl Pts',(-13.6752954743875,15.5,4.79949999999991));
#24878=CARTESIAN_POINT('Ctrl Pts',(-14.1314716057906,16.2901202367904,4.75783333333325));
#24879=CARTESIAN_POINT('Ctrl Pts',(-14.5876477371938,17.0802404735808,4.71616666666658));
#24880=CARTESIAN_POINT('Ctrl Pts',(-15.5,17.0802404735808,4.67449999999991));
#24881=CARTESIAN_POINT('Ctrl Pts',(-16.4123522628062,17.0802404735808,4.63283333333325));
#24882=CARTESIAN_POINT('Ctrl Pts',(-16.8685283942094,16.2901202367904,4.59116666666658));
#24883=CARTESIAN_POINT('Ctrl Pts',(-17.3247045256125,15.5,4.54949999999991));
#24884=CARTESIAN_POINT('Ctrl Pts',(-16.8685283942094,14.7098797632096,4.50783333333324));
#24885=CARTESIAN_POINT('Ctrl Pts',(-16.4123522628062,13.9197595264192,4.46616666666658));
#24886=CARTESIAN_POINT('Ctrl Pts',(-15.5,13.9197595264192,4.42449999999991));
#24887=CARTESIAN_POINT('Ctrl Pts',(-14.5876477371938,13.9197595264192,4.38283333333324));
#24888=CARTESIAN_POINT('Ctrl Pts',(-14.1314716057906,14.7098797632096,4.34116666666657));
#24889=CARTESIAN_POINT('Ctrl Pts',(-13.6752954743875,15.5,4.29949999999991));
#24890=CARTESIAN_POINT('Ctrl Pts',(-14.1314716057906,16.2901202367904,4.25783333333324));
#24891=CARTESIAN_POINT('Ctrl Pts',(-14.5876477371938,17.0802404735808,4.21616666666657));
#24892=CARTESIAN_POINT('Ctrl Pts',(-15.5,17.0802404735808,4.17449999999991));
#24893=CARTESIAN_POINT('Ctrl Pts',(-16.4123522628062,17.0802404735808,4.13283333333324));
#24894=CARTESIAN_POINT('Ctrl Pts',(-16.8685283942094,16.2901202367904,4.09116666666657));
#24895=CARTESIAN_POINT('Ctrl Pts',(-17.3247045256125,15.5,4.0494999999999));
#24896=CARTESIAN_POINT('Ctrl Pts',(-16.8685283942094,14.7098797632096,4.00783333333324));
#24897=CARTESIAN_POINT('Ctrl Pts',(-16.4123522628062,13.9197595264192,3.96616666666657));
#24898=CARTESIAN_POINT('Ctrl Pts',(-15.5,13.9197595264192,3.9244999999999));
#24899=CARTESIAN_POINT('Ctrl Pts',(-14.5876477371938,13.9197595264192,3.88283333333323));
#24900=CARTESIAN_POINT('Ctrl Pts',(-14.1314716057906,14.7098797632096,3.84116666666657));
#24901=CARTESIAN_POINT('Ctrl Pts',(-13.6752954743875,15.5,3.7994999999999));
#24902=CARTESIAN_POINT('Ctrl Pts',(-14.1314716057906,16.2901202367904,3.75783333333323));
#24903=CARTESIAN_POINT('Ctrl Pts',(-14.5876477371938,17.0802404735808,3.71616666666657));
#24904=CARTESIAN_POINT('Ctrl Pts',(-15.5,17.0802404735808,3.6744999999999));
#24905=CARTESIAN_POINT('Ctrl Pts',(-16.4123522628062,17.0802404735808,3.63283333333323));
#24906=CARTESIAN_POINT('Ctrl Pts',(-16.8685283942094,16.2901202367904,3.59116666666656));
#24907=CARTESIAN_POINT('Ctrl Pts',(-17.3247045256125,15.5,3.5494999999999));
#24908=CARTESIAN_POINT('Ctrl Pts',(-16.8685283942094,14.7098797632096,3.50783333333323));
#24909=CARTESIAN_POINT('Ctrl Pts',(-16.4123522628062,13.9197595264192,3.46616666666656));
#24910=CARTESIAN_POINT('Ctrl Pts',(-15.5,13.9197595264192,3.4244999999999));
#24911=CARTESIAN_POINT('Ctrl Pts',(-14.5876477371938,13.9197595264192,3.38283333333323));
#24912=CARTESIAN_POINT('Ctrl Pts',(-14.1314716057906,14.7098797632096,3.34116666666656));
#24913=CARTESIAN_POINT('Ctrl Pts',(-13.6752954743875,15.5,3.29949999999989));
#24914=CARTESIAN_POINT('Ctrl Pts',(-14.1314716057906,16.2901202367904,3.25783333333323));
#24915=CARTESIAN_POINT('Ctrl Pts',(-14.5876477371938,17.0802404735808,3.21616666666656));
#24916=CARTESIAN_POINT('Ctrl Pts',(-15.5,17.0802404735808,3.17449999999989));
#24917=CARTESIAN_POINT('Ctrl Pts',(-16.4123522628062,17.0802404735808,3.13283333333323));
#24918=CARTESIAN_POINT('Ctrl Pts',(-16.8685283942094,16.2901202367904,3.09116666666656));
#24919=CARTESIAN_POINT('Ctrl Pts',(-17.3247045256125,15.5,3.04949999999989));
#24920=CARTESIAN_POINT('Ctrl Pts',(-16.8685283942094,14.7098797632096,3.00783333333322));
#24921=CARTESIAN_POINT('Ctrl Pts',(-16.4123522628062,13.9197595264192,2.96616666666656));
#24922=CARTESIAN_POINT('Ctrl Pts',(-15.5,13.9197595264192,2.92449999999989));
#24923=CARTESIAN_POINT('Ctrl Pts',(-14.5876477371938,13.9197595264192,2.88283333333322));
#24924=CARTESIAN_POINT('Ctrl Pts',(-14.1314716057906,14.7098797632096,2.84116666666655));
#24925=CARTESIAN_POINT('Ctrl Pts',(-13.6752954743875,15.5,2.79949999999989));
#24926=CARTESIAN_POINT('Ctrl Pts',(-14.1314716057906,16.2901202367904,2.75783333333322));
#24927=CARTESIAN_POINT('Ctrl Pts',(-14.5876477371938,17.0802404735808,2.71616666666655));
#24928=CARTESIAN_POINT('Ctrl Pts',(-15.5,17.0802404735808,2.67449999999989));
#24929=CARTESIAN_POINT('Ctrl Pts',(-16.4123522628062,17.0802404735808,2.63283333333322));
#24930=CARTESIAN_POINT('Ctrl Pts',(-16.8685283942094,16.2901202367904,2.59116666666655));
#24931=CARTESIAN_POINT('Ctrl Pts',(-17.3247045256125,15.5,2.54949999999988));
#24932=CARTESIAN_POINT('Ctrl Pts',(-16.8685283942094,14.7098797632096,2.50783333333322));
#24933=CARTESIAN_POINT('Ctrl Pts',(-16.4123522628062,13.9197595264192,2.46616666666655));
#24934=CARTESIAN_POINT('Ctrl Pts',(-15.5,13.9197595264192,2.42449999999988));
#24935=CARTESIAN_POINT('Ctrl Pts',(-14.5876477371938,13.9197595264192,2.38283333333321));
#24936=CARTESIAN_POINT('Ctrl Pts',(-14.1314716057906,14.7098797632096,2.34116666666655));
#24937=CARTESIAN_POINT('Ctrl Pts',(-13.6752954743875,15.5,2.29949999999988));
#24938=CARTESIAN_POINT('Ctrl Pts',(-14.1314716057906,16.2901202367904,2.25783333333321));
#24939=CARTESIAN_POINT('Ctrl Pts',(-14.5876477371938,17.0802404735808,2.21616666666655));
#24940=CARTESIAN_POINT('Ctrl Pts',(-15.5,17.0802404735808,2.17449999999988));
#24941=CARTESIAN_POINT('Ctrl Pts',(-16.4123522628062,17.0802404735808,2.13283333333321));
#24942=CARTESIAN_POINT('Ctrl Pts',(-16.8685283942094,16.2901202367904,2.09116666666655));
#24943=CARTESIAN_POINT('Ctrl Pts',(-17.3247045256125,15.5,2.04949999999988));
#24944=CARTESIAN_POINT('Ctrl Pts',(-16.8685283942094,14.7098797632096,2.00783333333321));
#24945=CARTESIAN_POINT('Ctrl Pts',(-16.4123522628062,13.9197595264192,1.96616666666654));
#24946=CARTESIAN_POINT('Ctrl Pts',(-15.5,13.9197595264192,1.92449999999988));
#24947=CARTESIAN_POINT('Ctrl Pts',(-14.5876477371938,13.9197595264192,1.88283333333321));
#24948=CARTESIAN_POINT('Ctrl Pts',(-14.1314716057906,14.7098797632096,1.84116666666654));
#24949=CARTESIAN_POINT('Ctrl Pts',(-13.6752954743875,15.5,1.79949999999987));
#24950=CARTESIAN_POINT('Ctrl Pts',(-14.1314716057906,16.2901202367904,1.75783333333321));
#24951=CARTESIAN_POINT('Ctrl Pts',(-14.5876477371938,17.0802404735808,1.71616666666654));
#24952=CARTESIAN_POINT('Ctrl Pts',(-15.5,17.0802404735808,1.67449999999987));
#24953=CARTESIAN_POINT('Ctrl Pts',(-16.4123522628062,17.0802404735808,1.63283333333321));
#24954=CARTESIAN_POINT('Ctrl Pts',(-16.8685283942094,16.2901202367904,1.59116666666654));
#24955=CARTESIAN_POINT('Ctrl Pts',(-17.3247045256125,15.5,1.54949999999987));
#24956=CARTESIAN_POINT('Ctrl Pts',(-16.8685283942094,14.7098797632096,1.5078333333332));
#24957=CARTESIAN_POINT('Ctrl Pts',(-16.4123522628062,13.9197595264192,1.46616666666654));
#24958=CARTESIAN_POINT('Ctrl Pts',(-15.5,13.9197595264192,1.42449999999987));
#24959=CARTESIAN_POINT('Ctrl Pts',(-14.5876477371938,13.9197595264192,1.3828333333332));
#24960=CARTESIAN_POINT('Ctrl Pts',(-14.1314716057906,14.7098797632096,1.34116666666653));
#24961=CARTESIAN_POINT('Ctrl Pts',(-13.6752954743875,15.5,1.29949999999987));
#24962=CARTESIAN_POINT('Ctrl Pts',(-14.1314716057906,16.2901202367904,1.2578333333332));
#24963=CARTESIAN_POINT('Ctrl Pts',(-14.5876477371938,17.0802404735808,1.21616666666653));
#24964=CARTESIAN_POINT('Ctrl Pts',(-15.5,17.0802404735808,1.17449999999986));
#24965=CARTESIAN_POINT('Ctrl Pts',(-16.4123522628062,17.0802404735808,1.1328333333332));
#24966=CARTESIAN_POINT('Ctrl Pts',(-16.8685283942094,16.2901202367904,1.09116666666653));
#24967=CARTESIAN_POINT('Ctrl Pts',(-17.3247045256125,15.5,1.04949999999987));
#24968=CARTESIAN_POINT('Ctrl Pts',(-16.8685283942094,14.7098797632096,1.0078333333332));
#24969=CARTESIAN_POINT('Ctrl Pts',(-16.4123522628062,13.9197595264192,0.96616666666653));
#24970=CARTESIAN_POINT('Ctrl Pts',(-15.5,13.9197595264192,0.924499999999863));
#24971=CARTESIAN_POINT('Ctrl Pts',(-14.5876477371938,13.9197595264192,0.882833333333196));
#24972=CARTESIAN_POINT('Ctrl Pts',(-14.1314716057906,14.7098797632096,0.841166666666529));
#24973=CARTESIAN_POINT('Ctrl Pts',(-13.6752954743875,15.5,0.799499999999861));
#24974=CARTESIAN_POINT('Ctrl Pts',(-14.1314716057906,16.2901202367904,0.757833333333194));
#24975=CARTESIAN_POINT('Ctrl Pts',(-14.5876477371938,17.0802404735808,0.716166666666527));
#24976=CARTESIAN_POINT('Ctrl Pts',(-15.5,17.0802404735808,0.674499999999859));
#24977=CARTESIAN_POINT('Ctrl Pts',(-16.4123522628062,17.0802404735808,0.632833333333192));
#24978=CARTESIAN_POINT('Ctrl Pts',(-16.8685283942094,16.2901202367904,0.591166666666525));
#24979=CARTESIAN_POINT('Ctrl Pts',(-17.3247045256125,15.5,0.549499999999857));
#24980=CARTESIAN_POINT('Ctrl Pts',(-16.8685283942094,14.7098797632096,0.50783333333319));
#24981=CARTESIAN_POINT('Ctrl Pts',(-16.4123522628062,13.9197595264192,0.466166666666523));
#24982=CARTESIAN_POINT('Ctrl Pts',(-15.5,13.9197595264192,0.424499999999856));
#24983=CARTESIAN_POINT('Ctrl Pts',(-14.5876477371938,13.9197595264192,0.382833333333188));
#24984=CARTESIAN_POINT('Ctrl Pts',(-14.1314716057906,14.7098797632096,0.341166666666521));
#24985=CARTESIAN_POINT('Ctrl Pts',(-13.6752954743875,15.5,0.299499999999854));
#24986=CARTESIAN_POINT('Ctrl Pts',(-14.1314716057906,16.2901202367904,0.257833333333186));
#24987=CARTESIAN_POINT('Ctrl Pts',(-14.5876477371938,17.0802404735808,0.216166666666519));
#24988=CARTESIAN_POINT('Ctrl Pts',(-15.5,17.0802404735808,0.174499999999852));
#24989=CARTESIAN_POINT('Ctrl Pts',(-16.4123522628062,17.0802404735808,0.132833333333185));
#24990=CARTESIAN_POINT('Ctrl Pts',(-16.8685283942094,16.2901202367904,0.0911666666665173));
#24991=CARTESIAN_POINT('Ctrl Pts',(-17.3247045256125,15.5,0.04949999999985));
#24992=CARTESIAN_POINT('Ctrl Pts',(-16.8685283942094,14.7098797632096,0.00783333333318273));
#24993=CARTESIAN_POINT('Ctrl Pts',(-16.4123522628062,13.9197595264192,-0.0338333333334846));
#24994=CARTESIAN_POINT('Ctrl Pts',(-15.5,13.9197595264192,-0.0755000000001518));
#24995=CARTESIAN_POINT('Ctrl Pts',(-14.5876477371938,13.9197595264192,-0.117166666666817));
#24996=CARTESIAN_POINT('Ctrl Pts',(-14.1314716057906,14.7098797632096,-0.158833333333485));
#24997=CARTESIAN_POINT('Ctrl Pts',(-13.6752954743875,15.5,-0.200500000000152));
#24998=CARTESIAN_POINT('Ctrl Pts',(-14.1314716057906,16.2901202367904,-0.242166666666819));
#24999=CARTESIAN_POINT('Ctrl Pts',(-14.5876477371938,17.0802404735808,-0.283833333333487));
#25000=CARTESIAN_POINT('Ctrl Pts',(-15.5,17.0802404735808,-0.325500000000154));
#25001=CARTESIAN_POINT('Ctrl Pts',(-16.4123522628062,17.0802404735808,-0.367166666666821));
#25002=CARTESIAN_POINT('Ctrl Pts',(-16.8685283942094,16.2901202367904,-0.408833333333488));
#25003=CARTESIAN_POINT('Ctrl Pts',(-17.3247045256125,15.5,-0.450500000000156));
#25004=CARTESIAN_POINT('Ctrl Pts',(-16.8685283942094,14.7098797632096,-0.492166666666823));
#25005=CARTESIAN_POINT('Ctrl Pts',(-16.4123522628062,13.9197595264192,-0.53383333333349));
#25006=CARTESIAN_POINT('Ctrl Pts',(-15.5,13.9197595264192,-0.575500000000157));
#25007=CARTESIAN_POINT('Ctrl Pts',(-14.5876477371938,13.9197595264192,-0.617166666666825));
#25008=CARTESIAN_POINT('Ctrl Pts',(-14.1314716057906,14.7098797632096,-0.658833333333492));
#25009=CARTESIAN_POINT('Ctrl Pts',(-13.6752954743875,15.5,-0.700500000000159));
#25010=CARTESIAN_POINT('Ctrl Pts',(-14.1314716057906,16.2901202367904,-0.742166666666827));
#25011=CARTESIAN_POINT('Ctrl Pts',(-14.5876477371938,17.0802404735808,-0.783833333333494));
#25012=CARTESIAN_POINT('Ctrl Pts',(-15.5,17.0802404735808,-0.825500000000161));
#25013=CARTESIAN_POINT('Ctrl Pts',(-16.4123522628062,17.0802404735808,-0.867166666666829));
#25014=CARTESIAN_POINT('Ctrl Pts',(-16.8685283942094,16.2901202367904,-0.908833333333496));
#25015=CARTESIAN_POINT('Ctrl Pts',(-17.3247045256125,15.5,-0.950500000000163));
#25016=CARTESIAN_POINT('Ctrl Pts',(-16.8685283942094,14.7098797632096,-0.99216666666683));
#25017=CARTESIAN_POINT('Ctrl Pts',(-16.4123522628062,13.9197595264192,-1.0338333333335));
#25018=CARTESIAN_POINT('Ctrl Pts',(-15.5,13.9197595264192,-1.07550000000016));
#25019=CARTESIAN_POINT('Ctrl Pts',(-14.5876477371938,13.9197595264192,-1.11716666666683));
#25020=CARTESIAN_POINT('Ctrl Pts',(-14.1314716057906,14.7098797632096,-1.1588333333335));
#25021=CARTESIAN_POINT('Ctrl Pts',(-13.6752954743875,15.5,-1.20050000000017));
#25022=CARTESIAN_POINT('Ctrl Pts',(-14.1314716057906,16.2901202367904,-1.24216666666683));
#25023=CARTESIAN_POINT('Ctrl Pts',(-14.5876477371938,17.0802404735808,-1.2838333333335));
#25024=CARTESIAN_POINT('Ctrl Pts',(-15.5,17.0802404735808,-1.32550000000017));
#25025=CARTESIAN_POINT('Ctrl Pts',(-16.4123522628062,17.0802404735808,-1.36716666666683));
#25026=CARTESIAN_POINT('Ctrl Pts',(-16.8685283942094,16.2901202367904,-1.4088333333335));
#25027=CARTESIAN_POINT('Ctrl Pts',(-17.3247045256125,15.5,-1.45050000000017));
#25028=CARTESIAN_POINT('Ctrl Pts',(-16.8685283942094,14.7098797632096,-1.49216666666684));
#25029=CARTESIAN_POINT('Ctrl Pts',(-16.4123522628062,13.9197595264192,-1.5338333333335));
#25030=CARTESIAN_POINT('Ctrl Pts',(-15.5,13.9197595264192,-1.57550000000017));
#25031=CARTESIAN_POINT('Ctrl Pts',(-14.5876477371938,13.9197595264192,-1.61716666666684));
#25032=CARTESIAN_POINT('Ctrl Pts',(-14.1314716057906,14.7098797632096,-1.65883333333351));
#25033=CARTESIAN_POINT('Ctrl Pts',(-13.6752954743875,15.5,-1.70050000000017));
#25034=CARTESIAN_POINT('Ctrl Pts',(-14.1314716057906,16.2901202367904,-1.74216666666684));
#25035=CARTESIAN_POINT('Ctrl Pts',(-14.5876477371938,17.0802404735808,-1.78383333333351));
#25036=CARTESIAN_POINT('Ctrl Pts',(-15.5,17.0802404735808,-1.82550000000017));
#25037=CARTESIAN_POINT('Ctrl Pts',(-16.4123522628062,17.0802404735808,-1.86716666666684));
#25038=CARTESIAN_POINT('Ctrl Pts',(-16.8685283942094,16.2901202367904,-1.90883333333351));
#25039=CARTESIAN_POINT('Ctrl Pts',(-17.3247045256125,15.5,-1.95050000000018));
#25040=CARTESIAN_POINT('Ctrl Pts',(-16.8685283942094,14.7098797632096,-1.99216666666684));
#25041=CARTESIAN_POINT('Ctrl Pts',(-16.7005831533691,14.4189900731849,-2.00750661517932));
#25042=CARTESIAN_POINT('Ctrl Pts',(-16.4288360540161,14.2215542486879,-2.02512301646327));
#25043=CARTESIAN_POINT('',(-16.6356236599184,13.9369173167914,-2.22824840486548));
#25044=CARTESIAN_POINT('Ctrl Pts',(-15.5,17.4320632938683,11.440125));
#25045=CARTESIAN_POINT('Ctrl Pts',(-16.6154772628062,17.4320632938683,11.3984583333333));
#25046=CARTESIAN_POINT('Ctrl Pts',(-17.1732158942094,16.4660316469341,11.3567916666667));
#25047=CARTESIAN_POINT('Ctrl Pts',(-17.7309545256125,15.5,11.315125));
#25048=CARTESIAN_POINT('Ctrl Pts',(-17.1732158942094,14.5339683530659,11.2734583333333));
#25049=CARTESIAN_POINT('Ctrl Pts',(-16.6154772628062,13.5679367061317,11.2317916666667));
#25050=CARTESIAN_POINT('Ctrl Pts',(-15.5,13.5679367061317,11.190125));
#25051=CARTESIAN_POINT('Ctrl Pts',(-14.3845227371938,13.5679367061317,11.1484583333333));
#25052=CARTESIAN_POINT('Ctrl Pts',(-13.8267841057906,14.5339683530659,11.1067916666667));
#25053=CARTESIAN_POINT('Ctrl Pts',(-13.2690454743875,15.5,11.065125));
#25054=CARTESIAN_POINT('Ctrl Pts',(-13.8267841057906,16.4660316469341,11.0234583333333));
#25055=CARTESIAN_POINT('Ctrl Pts',(-14.3845227371938,17.4320632938683,10.9817916666667));
#25056=CARTESIAN_POINT('Ctrl Pts',(-15.5,17.4320632938683,10.940125));
#25057=CARTESIAN_POINT('Ctrl Pts',(-16.6154772628062,17.4320632938683,10.8984583333333));
#25058=CARTESIAN_POINT('Ctrl Pts',(-17.1732158942094,16.4660316469341,10.8567916666667));
#25059=CARTESIAN_POINT('Ctrl Pts',(-17.7309545256125,15.5,10.815125));
#25060=CARTESIAN_POINT('Ctrl Pts',(-17.1732158942094,14.5339683530659,10.7734583333333));
#25061=CARTESIAN_POINT('Ctrl Pts',(-16.6154772628062,13.5679367061317,10.7317916666667));
#25062=CARTESIAN_POINT('Ctrl Pts',(-15.5,13.5679367061317,10.690125));
#25063=CARTESIAN_POINT('Ctrl Pts',(-14.3845227371938,13.5679367061317,10.6484583333333));
#25064=CARTESIAN_POINT('Ctrl Pts',(-13.8267841057906,14.5339683530659,10.6067916666667));
#25065=CARTESIAN_POINT('Ctrl Pts',(-13.2690454743875,15.5,10.565125));
#25066=CARTESIAN_POINT('Ctrl Pts',(-13.8267841057906,16.4660316469341,10.5234583333333));
#25067=CARTESIAN_POINT('Ctrl Pts',(-14.3845227371938,17.4320632938683,10.4817916666667));
#25068=CARTESIAN_POINT('Ctrl Pts',(-15.5,17.4320632938683,10.440125));
#25069=CARTESIAN_POINT('Ctrl Pts',(-16.6154772628062,17.4320632938683,10.3984583333333));
#25070=CARTESIAN_POINT('Ctrl Pts',(-17.1732158942094,16.4660316469341,10.3567916666667));
#25071=CARTESIAN_POINT('Ctrl Pts',(-17.7309545256125,15.5,10.315125));
#25072=CARTESIAN_POINT('Ctrl Pts',(-17.1732158942094,14.5339683530659,10.2734583333333));
#25073=CARTESIAN_POINT('Ctrl Pts',(-16.6154772628062,13.5679367061317,10.2317916666667));
#25074=CARTESIAN_POINT('Ctrl Pts',(-15.5,13.5679367061317,10.190125));
#25075=CARTESIAN_POINT('Ctrl Pts',(-14.3845227371938,13.5679367061317,10.1484583333333));
#25076=CARTESIAN_POINT('Ctrl Pts',(-13.8267841057906,14.5339683530659,10.1067916666666));
#25077=CARTESIAN_POINT('Ctrl Pts',(-13.2690454743875,15.5,10.065125));
#25078=CARTESIAN_POINT('Ctrl Pts',(-13.8267841057906,16.4660316469341,10.0234583333333));
#25079=CARTESIAN_POINT('Ctrl Pts',(-14.3845227371938,17.4320632938683,9.98179166666664));
#25080=CARTESIAN_POINT('Ctrl Pts',(-15.5,17.4320632938683,9.94012499999998));
#25081=CARTESIAN_POINT('Ctrl Pts',(-16.6154772628062,17.4320632938683,9.89845833333331));
#25082=CARTESIAN_POINT('Ctrl Pts',(-17.1732158942094,16.4660316469341,9.85679166666664));
#25083=CARTESIAN_POINT('Ctrl Pts',(-17.7309545256125,15.5,9.81512499999998));
#25084=CARTESIAN_POINT('Ctrl Pts',(-17.1732158942094,14.5339683530659,9.77345833333331));
#25085=CARTESIAN_POINT('Ctrl Pts',(-16.6154772628062,13.5679367061317,9.73179166666664));
#25086=CARTESIAN_POINT('Ctrl Pts',(-15.5,13.5679367061317,9.69012499999998));
#25087=CARTESIAN_POINT('Ctrl Pts',(-14.3845227371938,13.5679367061317,9.64845833333331));
#25088=CARTESIAN_POINT('Ctrl Pts',(-13.8267841057906,14.5339683530659,9.60679166666664));
#25089=CARTESIAN_POINT('Ctrl Pts',(-13.2690454743875,15.5,9.56512499999998));
#25090=CARTESIAN_POINT('Ctrl Pts',(-13.8267841057906,16.4660316469341,9.52345833333331));
#25091=CARTESIAN_POINT('Ctrl Pts',(-14.3845227371938,17.4320632938683,9.48179166666664));
#25092=CARTESIAN_POINT('Ctrl Pts',(-15.5,17.4320632938683,9.44012499999997));
#25093=CARTESIAN_POINT('Ctrl Pts',(-16.6154772628062,17.4320632938683,9.39845833333331));
#25094=CARTESIAN_POINT('Ctrl Pts',(-17.1732158942094,16.4660316469341,9.35679166666664));
#25095=CARTESIAN_POINT('Ctrl Pts',(-17.7309545256125,15.5,9.31512499999997));
#25096=CARTESIAN_POINT('Ctrl Pts',(-17.1732158942094,14.5339683530659,9.2734583333333));
#25097=CARTESIAN_POINT('Ctrl Pts',(-16.6154772628062,13.5679367061317,9.23179166666664));
#25098=CARTESIAN_POINT('Ctrl Pts',(-15.5,13.5679367061317,9.19012499999997));
#25099=CARTESIAN_POINT('Ctrl Pts',(-14.3845227371938,13.5679367061317,9.1484583333333));
#25100=CARTESIAN_POINT('Ctrl Pts',(-13.8267841057906,14.5339683530659,9.10679166666664));
#25101=CARTESIAN_POINT('Ctrl Pts',(-13.2690454743875,15.5,9.06512499999997));
#25102=CARTESIAN_POINT('Ctrl Pts',(-13.8267841057906,16.4660316469341,9.0234583333333));
#25103=CARTESIAN_POINT('Ctrl Pts',(-14.3845227371938,17.4320632938683,8.98179166666663));
#25104=CARTESIAN_POINT('Ctrl Pts',(-15.5,17.4320632938683,8.94012499999997));
#25105=CARTESIAN_POINT('Ctrl Pts',(-16.6154772628062,17.4320632938683,8.8984583333333));
#25106=CARTESIAN_POINT('Ctrl Pts',(-17.1732158942094,16.4660316469341,8.85679166666663));
#25107=CARTESIAN_POINT('Ctrl Pts',(-17.7309545256125,15.5,8.81512499999996));
#25108=CARTESIAN_POINT('Ctrl Pts',(-17.1732158942094,14.5339683530659,8.7734583333333));
#25109=CARTESIAN_POINT('Ctrl Pts',(-16.6154772628062,13.5679367061317,8.73179166666663));
#25110=CARTESIAN_POINT('Ctrl Pts',(-15.5,13.5679367061317,8.69012499999996));
#25111=CARTESIAN_POINT('Ctrl Pts',(-14.3845227371938,13.5679367061317,8.64845833333329));
#25112=CARTESIAN_POINT('Ctrl Pts',(-13.8267841057906,14.5339683530659,8.60679166666663));
#25113=CARTESIAN_POINT('Ctrl Pts',(-13.2690454743875,15.5,8.56512499999996));
#25114=CARTESIAN_POINT('Ctrl Pts',(-13.8267841057906,16.4660316469341,8.52345833333329));
#25115=CARTESIAN_POINT('Ctrl Pts',(-14.3845227371938,17.4320632938683,8.48179166666663));
#25116=CARTESIAN_POINT('Ctrl Pts',(-15.5,17.4320632938683,8.44012499999996));
#25117=CARTESIAN_POINT('Ctrl Pts',(-16.6154772628062,17.4320632938683,8.39845833333329));
#25118=CARTESIAN_POINT('Ctrl Pts',(-17.1732158942094,16.4660316469341,8.35679166666662));
#25119=CARTESIAN_POINT('Ctrl Pts',(-17.7309545256125,15.5,8.31512499999996));
#25120=CARTESIAN_POINT('Ctrl Pts',(-17.1732158942094,14.5339683530659,8.27345833333329));
#25121=CARTESIAN_POINT('Ctrl Pts',(-16.6154772628062,13.5679367061317,8.23179166666662));
#25122=CARTESIAN_POINT('Ctrl Pts',(-15.5,13.5679367061317,8.19012499999996));
#25123=CARTESIAN_POINT('Ctrl Pts',(-14.3845227371938,13.5679367061317,8.14845833333329));
#25124=CARTESIAN_POINT('Ctrl Pts',(-13.8267841057906,14.5339683530659,8.10679166666662));
#25125=CARTESIAN_POINT('Ctrl Pts',(-13.2690454743875,15.5,8.06512499999995));
#25126=CARTESIAN_POINT('Ctrl Pts',(-13.8267841057906,16.4660316469341,8.02345833333329));
#25127=CARTESIAN_POINT('Ctrl Pts',(-14.3845227371938,17.4320632938683,7.98179166666662));
#25128=CARTESIAN_POINT('Ctrl Pts',(-15.5,17.4320632938683,7.94012499999995));
#25129=CARTESIAN_POINT('Ctrl Pts',(-16.6154772628062,17.4320632938683,7.89845833333329));
#25130=CARTESIAN_POINT('Ctrl Pts',(-17.1732158942094,16.4660316469341,7.85679166666662));
#25131=CARTESIAN_POINT('Ctrl Pts',(-17.7309545256125,15.5,7.81512499999995));
#25132=CARTESIAN_POINT('Ctrl Pts',(-17.1732158942094,14.5339683530659,7.77345833333328));
#25133=CARTESIAN_POINT('Ctrl Pts',(-16.6154772628062,13.5679367061317,7.73179166666662));
#25134=CARTESIAN_POINT('Ctrl Pts',(-15.5,13.5679367061317,7.69012499999995));
#25135=CARTESIAN_POINT('Ctrl Pts',(-14.3845227371938,13.5679367061317,7.64845833333328));
#25136=CARTESIAN_POINT('Ctrl Pts',(-13.8267841057906,14.5339683530659,7.60679166666661));
#25137=CARTESIAN_POINT('Ctrl Pts',(-13.2690454743875,15.5,7.56512499999995));
#25138=CARTESIAN_POINT('Ctrl Pts',(-13.8267841057906,16.4660316469341,7.52345833333328));
#25139=CARTESIAN_POINT('Ctrl Pts',(-14.3845227371938,17.4320632938683,7.48179166666661));
#25140=CARTESIAN_POINT('Ctrl Pts',(-15.5,17.4320632938683,7.44012499999995));
#25141=CARTESIAN_POINT('Ctrl Pts',(-16.6154772628062,17.4320632938683,7.39845833333328));
#25142=CARTESIAN_POINT('Ctrl Pts',(-17.1732158942094,16.4660316469341,7.35679166666661));
#25143=CARTESIAN_POINT('Ctrl Pts',(-17.7309545256125,15.5,7.31512499999995));
#25144=CARTESIAN_POINT('Ctrl Pts',(-17.1732158942094,14.5339683530659,7.27345833333328));
#25145=CARTESIAN_POINT('Ctrl Pts',(-16.6154772628062,13.5679367061317,7.23179166666661));
#25146=CARTESIAN_POINT('Ctrl Pts',(-15.5,13.5679367061317,7.19012499999994));
#25147=CARTESIAN_POINT('Ctrl Pts',(-14.3845227371938,13.5679367061317,7.14845833333328));
#25148=CARTESIAN_POINT('Ctrl Pts',(-13.8267841057906,14.5339683530659,7.10679166666661));
#25149=CARTESIAN_POINT('Ctrl Pts',(-13.2690454743875,15.5,7.06512499999994));
#25150=CARTESIAN_POINT('Ctrl Pts',(-13.8267841057906,16.4660316469341,7.02345833333327));
#25151=CARTESIAN_POINT('Ctrl Pts',(-14.3845227371938,17.4320632938683,6.98179166666661));
#25152=CARTESIAN_POINT('Ctrl Pts',(-15.5,17.4320632938683,6.94012499999994));
#25153=CARTESIAN_POINT('Ctrl Pts',(-16.6154772628062,17.4320632938683,6.89845833333327));
#25154=CARTESIAN_POINT('Ctrl Pts',(-17.1732158942094,16.4660316469341,6.8567916666666));
#25155=CARTESIAN_POINT('Ctrl Pts',(-17.7309545256125,15.5,6.81512499999994));
#25156=CARTESIAN_POINT('Ctrl Pts',(-17.1732158942094,14.5339683530659,6.77345833333327));
#25157=CARTESIAN_POINT('Ctrl Pts',(-16.6154772628062,13.5679367061317,6.7317916666666));
#25158=CARTESIAN_POINT('Ctrl Pts',(-15.5,13.5679367061317,6.69012499999994));
#25159=CARTESIAN_POINT('Ctrl Pts',(-14.3845227371938,13.5679367061317,6.64845833333327));
#25160=CARTESIAN_POINT('Ctrl Pts',(-13.8267841057906,14.5339683530659,6.6067916666666));
#25161=CARTESIAN_POINT('Ctrl Pts',(-13.2690454743875,15.5,6.56512499999993));
#25162=CARTESIAN_POINT('Ctrl Pts',(-13.8267841057906,16.4660316469341,6.52345833333327));
#25163=CARTESIAN_POINT('Ctrl Pts',(-14.3845227371938,17.4320632938683,6.4817916666666));
#25164=CARTESIAN_POINT('Ctrl Pts',(-15.5,17.4320632938683,6.44012499999993));
#25165=CARTESIAN_POINT('Ctrl Pts',(-16.6154772628062,17.4320632938683,6.39845833333327));
#25166=CARTESIAN_POINT('Ctrl Pts',(-17.1732158942094,16.4660316469341,6.3567916666666));
#25167=CARTESIAN_POINT('Ctrl Pts',(-17.7309545256125,15.5,6.31512499999993));
#25168=CARTESIAN_POINT('Ctrl Pts',(-17.1732158942094,14.5339683530659,6.27345833333326));
#25169=CARTESIAN_POINT('Ctrl Pts',(-16.6154772628062,13.5679367061317,6.2317916666666));
#25170=CARTESIAN_POINT('Ctrl Pts',(-15.5,13.5679367061317,6.19012499999993));
#25171=CARTESIAN_POINT('Ctrl Pts',(-14.3845227371938,13.5679367061317,6.14845833333326));
#25172=CARTESIAN_POINT('Ctrl Pts',(-13.8267841057906,14.5339683530659,6.10679166666659));
#25173=CARTESIAN_POINT('Ctrl Pts',(-13.2690454743875,15.5,6.06512499999993));
#25174=CARTESIAN_POINT('Ctrl Pts',(-13.8267841057906,16.4660316469341,6.02345833333326));
#25175=CARTESIAN_POINT('Ctrl Pts',(-14.3845227371938,17.4320632938683,5.98179166666659));
#25176=CARTESIAN_POINT('Ctrl Pts',(-15.5,17.4320632938683,5.94012499999993));
#25177=CARTESIAN_POINT('Ctrl Pts',(-16.6154772628062,17.4320632938683,5.89845833333326));
#25178=CARTESIAN_POINT('Ctrl Pts',(-17.1732158942094,16.4660316469341,5.85679166666659));
#25179=CARTESIAN_POINT('Ctrl Pts',(-17.7309545256125,15.5,5.81512499999992));
#25180=CARTESIAN_POINT('Ctrl Pts',(-17.1732158942094,14.5339683530659,5.77345833333326));
#25181=CARTESIAN_POINT('Ctrl Pts',(-16.6154772628062,13.5679367061317,5.73179166666659));
#25182=CARTESIAN_POINT('Ctrl Pts',(-15.5,13.5679367061317,5.69012499999992));
#25183=CARTESIAN_POINT('Ctrl Pts',(-14.3845227371938,13.5679367061317,5.64845833333326));
#25184=CARTESIAN_POINT('Ctrl Pts',(-13.8267841057906,14.5339683530659,5.60679166666659));
#25185=CARTESIAN_POINT('Ctrl Pts',(-13.2690454743875,15.5,5.56512499999992));
#25186=CARTESIAN_POINT('Ctrl Pts',(-13.8267841057906,16.4660316469341,5.52345833333325));
#25187=CARTESIAN_POINT('Ctrl Pts',(-14.3845227371938,17.4320632938683,5.48179166666659));
#25188=CARTESIAN_POINT('Ctrl Pts',(-15.5,17.4320632938683,5.44012499999992));
#25189=CARTESIAN_POINT('Ctrl Pts',(-16.6154772628062,17.4320632938683,5.39845833333325));
#25190=CARTESIAN_POINT('Ctrl Pts',(-17.1732158942094,16.4660316469341,5.35679166666658));
#25191=CARTESIAN_POINT('Ctrl Pts',(-17.7309545256125,15.5,5.31512499999992));
#25192=CARTESIAN_POINT('Ctrl Pts',(-17.1732158942094,14.5339683530659,5.27345833333325));
#25193=CARTESIAN_POINT('Ctrl Pts',(-16.6154772628062,13.5679367061317,5.23179166666658));
#25194=CARTESIAN_POINT('Ctrl Pts',(-15.5,13.5679367061317,5.19012499999992));
#25195=CARTESIAN_POINT('Ctrl Pts',(-14.3845227371938,13.5679367061317,5.14845833333325));
#25196=CARTESIAN_POINT('Ctrl Pts',(-13.8267841057906,14.5339683530659,5.10679166666658));
#25197=CARTESIAN_POINT('Ctrl Pts',(-13.2690454743875,15.5,5.06512499999991));
#25198=CARTESIAN_POINT('Ctrl Pts',(-13.8267841057906,16.4660316469341,5.02345833333325));
#25199=CARTESIAN_POINT('Ctrl Pts',(-14.3845227371938,17.4320632938683,4.98179166666658));
#25200=CARTESIAN_POINT('Ctrl Pts',(-15.5,17.4320632938683,4.94012499999991));
#25201=CARTESIAN_POINT('Ctrl Pts',(-16.6154772628062,17.4320632938683,4.89845833333325));
#25202=CARTESIAN_POINT('Ctrl Pts',(-17.1732158942094,16.4660316469341,4.85679166666658));
#25203=CARTESIAN_POINT('Ctrl Pts',(-17.7309545256125,15.5,4.81512499999991));
#25204=CARTESIAN_POINT('Ctrl Pts',(-17.1732158942094,14.5339683530659,4.77345833333324));
#25205=CARTESIAN_POINT('Ctrl Pts',(-16.6154772628062,13.5679367061317,4.73179166666658));
#25206=CARTESIAN_POINT('Ctrl Pts',(-15.5,13.5679367061317,4.69012499999991));
#25207=CARTESIAN_POINT('Ctrl Pts',(-14.3845227371938,13.5679367061317,4.64845833333324));
#25208=CARTESIAN_POINT('Ctrl Pts',(-13.8267841057906,14.5339683530659,4.60679166666657));
#25209=CARTESIAN_POINT('Ctrl Pts',(-13.2690454743875,15.5,4.56512499999991));
#25210=CARTESIAN_POINT('Ctrl Pts',(-13.8267841057906,16.4660316469341,4.52345833333324));
#25211=CARTESIAN_POINT('Ctrl Pts',(-14.3845227371938,17.4320632938683,4.48179166666657));
#25212=CARTESIAN_POINT('Ctrl Pts',(-15.5,17.4320632938683,4.44012499999991));
#25213=CARTESIAN_POINT('Ctrl Pts',(-16.6154772628062,17.4320632938683,4.39845833333324));
#25214=CARTESIAN_POINT('Ctrl Pts',(-17.1732158942094,16.4660316469341,4.35679166666657));
#25215=CARTESIAN_POINT('Ctrl Pts',(-17.7309545256125,15.5,4.31512499999991));
#25216=CARTESIAN_POINT('Ctrl Pts',(-17.1732158942094,14.5339683530659,4.27345833333324));
#25217=CARTESIAN_POINT('Ctrl Pts',(-16.6154772628062,13.5679367061317,4.23179166666657));
#25218=CARTESIAN_POINT('Ctrl Pts',(-15.5,13.5679367061317,4.1901249999999));
#25219=CARTESIAN_POINT('Ctrl Pts',(-14.3845227371938,13.5679367061317,4.14845833333324));
#25220=CARTESIAN_POINT('Ctrl Pts',(-13.8267841057906,14.5339683530659,4.10679166666657));
#25221=CARTESIAN_POINT('Ctrl Pts',(-13.2690454743875,15.5,4.0651249999999));
#25222=CARTESIAN_POINT('Ctrl Pts',(-13.8267841057906,16.4660316469341,4.02345833333323));
#25223=CARTESIAN_POINT('Ctrl Pts',(-14.3845227371938,17.4320632938683,3.98179166666657));
#25224=CARTESIAN_POINT('Ctrl Pts',(-15.5,17.4320632938683,3.9401249999999));
#25225=CARTESIAN_POINT('Ctrl Pts',(-16.6154772628062,17.4320632938683,3.89845833333323));
#25226=CARTESIAN_POINT('Ctrl Pts',(-17.1732158942094,16.4660316469341,3.85679166666657));
#25227=CARTESIAN_POINT('Ctrl Pts',(-17.7309545256125,15.5,3.8151249999999));
#25228=CARTESIAN_POINT('Ctrl Pts',(-17.1732158942094,14.5339683530659,3.77345833333323));
#25229=CARTESIAN_POINT('Ctrl Pts',(-16.6154772628062,13.5679367061317,3.73179166666656));
#25230=CARTESIAN_POINT('Ctrl Pts',(-15.5,13.5679367061317,3.6901249999999));
#25231=CARTESIAN_POINT('Ctrl Pts',(-14.3845227371938,13.5679367061317,3.64845833333323));
#25232=CARTESIAN_POINT('Ctrl Pts',(-13.8267841057906,14.5339683530659,3.60679166666656));
#25233=CARTESIAN_POINT('Ctrl Pts',(-13.2690454743875,15.5,3.5651249999999));
#25234=CARTESIAN_POINT('Ctrl Pts',(-13.8267841057906,16.4660316469341,3.52345833333323));
#25235=CARTESIAN_POINT('Ctrl Pts',(-14.3845227371938,17.4320632938683,3.48179166666656));
#25236=CARTESIAN_POINT('Ctrl Pts',(-15.5,17.4320632938683,3.44012499999989));
#25237=CARTESIAN_POINT('Ctrl Pts',(-16.6154772628062,17.4320632938683,3.39845833333323));
#25238=CARTESIAN_POINT('Ctrl Pts',(-17.1732158942094,16.4660316469341,3.35679166666656));
#25239=CARTESIAN_POINT('Ctrl Pts',(-17.7309545256125,15.5,3.31512499999989));
#25240=CARTESIAN_POINT('Ctrl Pts',(-17.1732158942094,14.5339683530659,3.27345833333322));
#25241=CARTESIAN_POINT('Ctrl Pts',(-16.6154772628062,13.5679367061317,3.23179166666656));
#25242=CARTESIAN_POINT('Ctrl Pts',(-15.5,13.5679367061317,3.19012499999989));
#25243=CARTESIAN_POINT('Ctrl Pts',(-14.3845227371938,13.5679367061317,3.14845833333322));
#25244=CARTESIAN_POINT('Ctrl Pts',(-13.8267841057906,14.5339683530659,3.10679166666655));
#25245=CARTESIAN_POINT('Ctrl Pts',(-13.2690454743875,15.5,3.06512499999989));
#25246=CARTESIAN_POINT('Ctrl Pts',(-13.8267841057906,16.4660316469341,3.02345833333322));
#25247=CARTESIAN_POINT('Ctrl Pts',(-14.3845227371938,17.4320632938683,2.98179166666655));
#25248=CARTESIAN_POINT('Ctrl Pts',(-15.5,17.4320632938683,2.94012499999989));
#25249=CARTESIAN_POINT('Ctrl Pts',(-16.6154772628062,17.4320632938683,2.89845833333322));
#25250=CARTESIAN_POINT('Ctrl Pts',(-17.1732158942094,16.4660316469341,2.85679166666655));
#25251=CARTESIAN_POINT('Ctrl Pts',(-17.7309545256125,15.5,2.81512499999988));
#25252=CARTESIAN_POINT('Ctrl Pts',(-17.1732158942094,14.5339683530659,2.77345833333322));
#25253=CARTESIAN_POINT('Ctrl Pts',(-16.6154772628062,13.5679367061317,2.73179166666655));
#25254=CARTESIAN_POINT('Ctrl Pts',(-15.5,13.5679367061317,2.69012499999988));
#25255=CARTESIAN_POINT('Ctrl Pts',(-14.3845227371938,13.5679367061317,2.64845833333321));
#25256=CARTESIAN_POINT('Ctrl Pts',(-13.8267841057906,14.5339683530659,2.60679166666655));
#25257=CARTESIAN_POINT('Ctrl Pts',(-13.2690454743875,15.5,2.56512499999988));
#25258=CARTESIAN_POINT('Ctrl Pts',(-13.8267841057906,16.4660316469341,2.52345833333321));
#25259=CARTESIAN_POINT('Ctrl Pts',(-14.3845227371938,17.4320632938683,2.48179166666655));
#25260=CARTESIAN_POINT('Ctrl Pts',(-15.5,17.4320632938683,2.44012499999988));
#25261=CARTESIAN_POINT('Ctrl Pts',(-16.6154772628062,17.4320632938683,2.39845833333321));
#25262=CARTESIAN_POINT('Ctrl Pts',(-17.1732158942094,16.4660316469341,2.35679166666655));
#25263=CARTESIAN_POINT('Ctrl Pts',(-17.7309545256125,15.5,2.31512499999988));
#25264=CARTESIAN_POINT('Ctrl Pts',(-17.1732158942094,14.5339683530659,2.27345833333321));
#25265=CARTESIAN_POINT('Ctrl Pts',(-16.6154772628062,13.5679367061317,2.23179166666654));
#25266=CARTESIAN_POINT('Ctrl Pts',(-15.5,13.5679367061317,2.19012499999988));
#25267=CARTESIAN_POINT('Ctrl Pts',(-14.3845227371938,13.5679367061317,2.14845833333321));
#25268=CARTESIAN_POINT('Ctrl Pts',(-13.8267841057906,14.5339683530659,2.10679166666654));
#25269=CARTESIAN_POINT('Ctrl Pts',(-13.2690454743875,15.5,2.06512499999987));
#25270=CARTESIAN_POINT('Ctrl Pts',(-13.8267841057906,16.4660316469341,2.02345833333321));
#25271=CARTESIAN_POINT('Ctrl Pts',(-14.3845227371938,17.4320632938683,1.98179166666654));
#25272=CARTESIAN_POINT('Ctrl Pts',(-15.5,17.4320632938683,1.94012499999987));
#25273=CARTESIAN_POINT('Ctrl Pts',(-16.6154772628062,17.4320632938683,1.89845833333321));
#25274=CARTESIAN_POINT('Ctrl Pts',(-17.1732158942094,16.4660316469341,1.85679166666654));
#25275=CARTESIAN_POINT('Ctrl Pts',(-17.7309545256125,15.5,1.81512499999987));
#25276=CARTESIAN_POINT('Ctrl Pts',(-17.1732158942094,14.5339683530659,1.7734583333332));
#25277=CARTESIAN_POINT('Ctrl Pts',(-16.6154772628062,13.5679367061317,1.73179166666654));
#25278=CARTESIAN_POINT('Ctrl Pts',(-15.5,13.5679367061317,1.69012499999987));
#25279=CARTESIAN_POINT('Ctrl Pts',(-14.3845227371938,13.5679367061317,1.6484583333332));
#25280=CARTESIAN_POINT('Ctrl Pts',(-13.8267841057906,14.5339683530659,1.60679166666653));
#25281=CARTESIAN_POINT('Ctrl Pts',(-13.2690454743875,15.5,1.56512499999987));
#25282=CARTESIAN_POINT('Ctrl Pts',(-13.8267841057906,16.4660316469341,1.5234583333332));
#25283=CARTESIAN_POINT('Ctrl Pts',(-14.3845227371938,17.4320632938683,1.48179166666653));
#25284=CARTESIAN_POINT('Ctrl Pts',(-15.5,17.4320632938683,1.44012499999987));
#25285=CARTESIAN_POINT('Ctrl Pts',(-16.6154772628062,17.4320632938683,1.3984583333332));
#25286=CARTESIAN_POINT('Ctrl Pts',(-17.1732158942094,16.4660316469341,1.35679166666653));
#25287=CARTESIAN_POINT('Ctrl Pts',(-17.7309545256125,15.5,1.31512499999987));
#25288=CARTESIAN_POINT('Ctrl Pts',(-17.1732158942094,14.5339683530659,1.2734583333332));
#25289=CARTESIAN_POINT('Ctrl Pts',(-16.6154772628062,13.5679367061317,1.23179166666653));
#25290=CARTESIAN_POINT('Ctrl Pts',(-15.5,13.5679367061317,1.19012499999986));
#25291=CARTESIAN_POINT('Ctrl Pts',(-14.3845227371938,13.5679367061317,1.1484583333332));
#25292=CARTESIAN_POINT('Ctrl Pts',(-13.8267841057906,14.5339683530659,1.10679166666653));
#25293=CARTESIAN_POINT('Ctrl Pts',(-13.2690454743875,15.5,1.06512499999986));
#25294=CARTESIAN_POINT('Ctrl Pts',(-13.8267841057906,16.4660316469341,1.02345833333319));
#25295=CARTESIAN_POINT('Ctrl Pts',(-14.3845227371938,17.4320632938683,0.981791666666527));
#25296=CARTESIAN_POINT('Ctrl Pts',(-15.5,17.4320632938683,0.94012499999986));
#25297=CARTESIAN_POINT('Ctrl Pts',(-16.6154772628062,17.4320632938683,0.898458333333192));
#25298=CARTESIAN_POINT('Ctrl Pts',(-17.1732158942094,16.4660316469341,0.856791666666525));
#25299=CARTESIAN_POINT('Ctrl Pts',(-17.7309545256125,15.5,0.815124999999858));
#25300=CARTESIAN_POINT('Ctrl Pts',(-17.1732158942094,14.5339683530659,0.77345833333319));
#25301=CARTESIAN_POINT('Ctrl Pts',(-16.6154772628062,13.5679367061317,0.731791666666523));
#25302=CARTESIAN_POINT('Ctrl Pts',(-15.5,13.5679367061317,0.690124999999856));
#25303=CARTESIAN_POINT('Ctrl Pts',(-14.3845227371938,13.5679367061317,0.648458333333188));
#25304=CARTESIAN_POINT('Ctrl Pts',(-13.8267841057906,14.5339683530659,0.606791666666521));
#25305=CARTESIAN_POINT('Ctrl Pts',(-13.2690454743875,15.5,0.565124999999854));
#25306=CARTESIAN_POINT('Ctrl Pts',(-13.8267841057906,16.4660316469341,0.523458333333187));
#25307=CARTESIAN_POINT('Ctrl Pts',(-14.3845227371938,17.4320632938683,0.481791666666519));
#25308=CARTESIAN_POINT('Ctrl Pts',(-15.5,17.4320632938683,0.440124999999852));
#25309=CARTESIAN_POINT('Ctrl Pts',(-16.6154772628062,17.4320632938683,0.398458333333185));
#25310=CARTESIAN_POINT('Ctrl Pts',(-17.1732158942094,16.4660316469341,0.356791666666518));
#25311=CARTESIAN_POINT('Ctrl Pts',(-17.7309545256125,15.5,0.31512499999985));
#25312=CARTESIAN_POINT('Ctrl Pts',(-17.1732158942094,14.5339683530659,0.273458333333183));
#25313=CARTESIAN_POINT('Ctrl Pts',(-16.6154772628062,13.5679367061317,0.231791666666516));
#25314=CARTESIAN_POINT('Ctrl Pts',(-15.5,13.5679367061317,0.190124999999848));
#25315=CARTESIAN_POINT('Ctrl Pts',(-14.3845227371938,13.5679367061317,0.148458333333183));
#25316=CARTESIAN_POINT('Ctrl Pts',(-13.8267841057906,14.5339683530659,0.106791666666516));
#25317=CARTESIAN_POINT('Ctrl Pts',(-13.2690454743875,15.5,0.0651249999998483));
#25318=CARTESIAN_POINT('Ctrl Pts',(-13.8267841057906,16.4660316469341,0.023458333333181));
#25319=CARTESIAN_POINT('Ctrl Pts',(-14.3845227371938,17.4320632938683,-0.0182083333334863));
#25320=CARTESIAN_POINT('Ctrl Pts',(-15.5,17.4320632938683,-0.0598750000001536));
#25321=CARTESIAN_POINT('Ctrl Pts',(-16.6154772628062,17.4320632938683,-0.101541666666821));
#25322=CARTESIAN_POINT('Ctrl Pts',(-17.1732158942094,16.4660316469341,-0.143208333333488));
#25323=CARTESIAN_POINT('Ctrl Pts',(-17.7309545256125,15.5,-0.184875000000155));
#25324=CARTESIAN_POINT('Ctrl Pts',(-17.1732158942094,14.5339683530659,-0.226541666666823));
#25325=CARTESIAN_POINT('Ctrl Pts',(-16.6154772628062,13.5679367061317,-0.26820833333349));
#25326=CARTESIAN_POINT('Ctrl Pts',(-15.5,13.5679367061317,-0.309875000000157));
#25327=CARTESIAN_POINT('Ctrl Pts',(-14.3845227371938,13.5679367061317,-0.351541666666825));
#25328=CARTESIAN_POINT('Ctrl Pts',(-13.8267841057906,14.5339683530659,-0.393208333333492));
#25329=CARTESIAN_POINT('Ctrl Pts',(-13.2690454743875,15.5,-0.434875000000159));
#25330=CARTESIAN_POINT('Ctrl Pts',(-13.8267841057906,16.4660316469341,-0.476541666666826));
#25331=CARTESIAN_POINT('Ctrl Pts',(-14.3845227371938,17.4320632938683,-0.518208333333494));
#25332=CARTESIAN_POINT('Ctrl Pts',(-15.5,17.4320632938683,-0.559875000000161));
#25333=CARTESIAN_POINT('Ctrl Pts',(-16.6154772628062,17.4320632938683,-0.601541666666828));
#25334=CARTESIAN_POINT('Ctrl Pts',(-17.1732158942094,16.4660316469341,-0.643208333333495));
#25335=CARTESIAN_POINT('Ctrl Pts',(-17.7309545256125,15.5,-0.684875000000163));
#25336=CARTESIAN_POINT('Ctrl Pts',(-17.1732158942094,14.5339683530659,-0.72654166666683));
#25337=CARTESIAN_POINT('Ctrl Pts',(-16.6154772628062,13.5679367061317,-0.768208333333497));
#25338=CARTESIAN_POINT('Ctrl Pts',(-15.5,13.5679367061317,-0.809875000000165));
#25339=CARTESIAN_POINT('Ctrl Pts',(-14.3845227371938,13.5679367061317,-0.851541666666832));
#25340=CARTESIAN_POINT('Ctrl Pts',(-13.8267841057906,14.5339683530659,-0.893208333333499));
#25341=CARTESIAN_POINT('Ctrl Pts',(-13.2690454743875,15.5,-0.934875000000167));
#25342=CARTESIAN_POINT('Ctrl Pts',(-13.8267841057906,16.4660316469341,-0.976541666666834));
#25343=CARTESIAN_POINT('Ctrl Pts',(-14.3845227371938,17.4320632938683,-1.0182083333335));
#25344=CARTESIAN_POINT('Ctrl Pts',(-15.5,17.4320632938683,-1.05987500000017));
#25345=CARTESIAN_POINT('Ctrl Pts',(-16.6154772628062,17.4320632938683,-1.10154166666683));
#25346=CARTESIAN_POINT('Ctrl Pts',(-17.1732158942094,16.4660316469341,-1.1432083333335));
#25347=CARTESIAN_POINT('Ctrl Pts',(-17.7309545256125,15.5,-1.18487500000017));
#25348=CARTESIAN_POINT('Ctrl Pts',(-17.1732158942094,14.5339683530659,-1.22654166666684));
#25349=CARTESIAN_POINT('Ctrl Pts',(-16.6154772628062,13.5679367061317,-1.2682083333335));
#25350=CARTESIAN_POINT('Ctrl Pts',(-15.5,13.5679367061317,-1.30987500000017));
#25351=CARTESIAN_POINT('Ctrl Pts',(-14.3845227371938,13.5679367061317,-1.35154166666684));
#25352=CARTESIAN_POINT('Ctrl Pts',(-13.8267841057906,14.5339683530659,-1.3932083333335));
#25353=CARTESIAN_POINT('Ctrl Pts',(-13.2690454743875,15.5,-1.43487500000017));
#25354=CARTESIAN_POINT('Ctrl Pts',(-13.8267841057906,16.4660316469341,-1.47654166666684));
#25355=CARTESIAN_POINT('Ctrl Pts',(-14.3845227371938,17.4320632938683,-1.51820833333351));
#25356=CARTESIAN_POINT('Ctrl Pts',(-15.5,17.4320632938683,-1.55987500000017));
#25357=CARTESIAN_POINT('Ctrl Pts',(-16.6154772628062,17.4320632938683,-1.60154166666684));
#25358=CARTESIAN_POINT('Ctrl Pts',(-17.1732158942094,16.4660316469341,-1.64320833333351));
#25359=CARTESIAN_POINT('Ctrl Pts',(-17.7309545256125,15.5,-1.68487500000018));
#25360=CARTESIAN_POINT('Ctrl Pts',(-17.1732158942094,14.5339683530659,-1.72654166666684));
#25361=CARTESIAN_POINT('Ctrl Pts',(-16.9678753992805,14.1783081829978,-1.74188192368624));
#25362=CARTESIAN_POINT('Ctrl Pts',(-16.6356255246375,13.9369186715641,-1.75949830599533));
#25363=CARTESIAN_POINT('Ctrl Pts',(-15.5,17.0802404735808,11.237));
#25364=CARTESIAN_POINT('Ctrl Pts',(-16.4123522628062,17.0802404735808,11.1953333333333));
#25365=CARTESIAN_POINT('Ctrl Pts',(-16.8685283942094,16.2901202367904,11.1536666666667));
#25366=CARTESIAN_POINT('Ctrl Pts',(-17.3247045256125,15.5,11.112));
#25367=CARTESIAN_POINT('Ctrl Pts',(-16.8685283942094,14.7098797632096,11.0703333333333));
#25368=CARTESIAN_POINT('Ctrl Pts',(-16.4123522628062,13.9197595264192,11.0286666666667));
#25369=CARTESIAN_POINT('Ctrl Pts',(-15.5,13.9197595264192,10.987));
#25370=CARTESIAN_POINT('Ctrl Pts',(-14.5876477371938,13.9197595264192,10.9453333333333));
#25371=CARTESIAN_POINT('Ctrl Pts',(-14.1314716057906,14.7098797632096,10.9036666666667));
#25372=CARTESIAN_POINT('Ctrl Pts',(-13.6752954743875,15.5,10.862));
#25373=CARTESIAN_POINT('Ctrl Pts',(-14.1314716057906,16.2901202367904,10.8203333333333));
#25374=CARTESIAN_POINT('Ctrl Pts',(-14.5876477371938,17.0802404735808,10.7786666666667));
#25375=CARTESIAN_POINT('Ctrl Pts',(-15.5,17.0802404735808,10.737));
#25376=CARTESIAN_POINT('Ctrl Pts',(-16.4123522628062,17.0802404735808,10.6953333333333));
#25377=CARTESIAN_POINT('Ctrl Pts',(-16.8685283942094,16.2901202367904,10.6536666666667));
#25378=CARTESIAN_POINT('Ctrl Pts',(-17.3247045256125,15.5,10.612));
#25379=CARTESIAN_POINT('Ctrl Pts',(-16.8685283942094,14.7098797632096,10.5703333333333));
#25380=CARTESIAN_POINT('Ctrl Pts',(-16.4123522628062,13.9197595264192,10.5286666666667));
#25381=CARTESIAN_POINT('Ctrl Pts',(-15.5,13.9197595264192,10.487));
#25382=CARTESIAN_POINT('Ctrl Pts',(-14.5876477371938,13.9197595264192,10.4453333333333));
#25383=CARTESIAN_POINT('Ctrl Pts',(-14.1314716057906,14.7098797632096,10.4036666666667));
#25384=CARTESIAN_POINT('Ctrl Pts',(-13.6752954743875,15.5,10.362));
#25385=CARTESIAN_POINT('Ctrl Pts',(-14.1314716057906,16.2901202367904,10.3203333333333));
#25386=CARTESIAN_POINT('Ctrl Pts',(-14.5876477371938,17.0802404735808,10.2786666666667));
#25387=CARTESIAN_POINT('Ctrl Pts',(-15.5,17.0802404735808,10.237));
#25388=CARTESIAN_POINT('Ctrl Pts',(-16.4123522628062,17.0802404735808,10.1953333333333));
#25389=CARTESIAN_POINT('Ctrl Pts',(-16.8685283942094,16.2901202367904,10.1536666666667));
#25390=CARTESIAN_POINT('Ctrl Pts',(-17.3247045256125,15.5,10.112));
#25391=CARTESIAN_POINT('Ctrl Pts',(-16.8685283942094,14.7098797632096,10.0703333333333));
#25392=CARTESIAN_POINT('Ctrl Pts',(-16.4123522628062,13.9197595264192,10.0286666666667));
#25393=CARTESIAN_POINT('Ctrl Pts',(-15.5,13.9197595264192,9.98699999999998));
#25394=CARTESIAN_POINT('Ctrl Pts',(-14.5876477371938,13.9197595264192,9.94533333333332));
#25395=CARTESIAN_POINT('Ctrl Pts',(-14.1314716057906,14.7098797632096,9.90366666666665));
#25396=CARTESIAN_POINT('Ctrl Pts',(-13.6752954743875,15.5,9.86199999999998));
#25397=CARTESIAN_POINT('Ctrl Pts',(-14.1314716057906,16.2901202367904,9.82033333333331));
#25398=CARTESIAN_POINT('Ctrl Pts',(-14.5876477371938,17.0802404735808,9.77866666666665));
#25399=CARTESIAN_POINT('Ctrl Pts',(-15.5,17.0802404735808,9.73699999999998));
#25400=CARTESIAN_POINT('Ctrl Pts',(-16.4123522628062,17.0802404735808,9.69533333333331));
#25401=CARTESIAN_POINT('Ctrl Pts',(-16.8685283942094,16.2901202367904,9.65366666666664));
#25402=CARTESIAN_POINT('Ctrl Pts',(-17.3247045256125,15.5,9.61199999999998));
#25403=CARTESIAN_POINT('Ctrl Pts',(-16.8685283942094,14.7098797632096,9.57033333333331));
#25404=CARTESIAN_POINT('Ctrl Pts',(-16.4123522628062,13.9197595264192,9.52866666666664));
#25405=CARTESIAN_POINT('Ctrl Pts',(-15.5,13.9197595264192,9.48699999999998));
#25406=CARTESIAN_POINT('Ctrl Pts',(-14.5876477371938,13.9197595264192,9.44533333333331));
#25407=CARTESIAN_POINT('Ctrl Pts',(-14.1314716057906,14.7098797632096,9.40366666666664));
#25408=CARTESIAN_POINT('Ctrl Pts',(-13.6752954743875,15.5,9.36199999999997));
#25409=CARTESIAN_POINT('Ctrl Pts',(-14.1314716057906,16.2901202367904,9.32033333333331));
#25410=CARTESIAN_POINT('Ctrl Pts',(-14.5876477371938,17.0802404735808,9.27866666666664));
#25411=CARTESIAN_POINT('Ctrl Pts',(-15.5,17.0802404735808,9.23699999999997));
#25412=CARTESIAN_POINT('Ctrl Pts',(-16.4123522628062,17.0802404735808,9.19533333333331));
#25413=CARTESIAN_POINT('Ctrl Pts',(-16.8685283942094,16.2901202367904,9.15366666666664));
#25414=CARTESIAN_POINT('Ctrl Pts',(-17.3247045256125,15.5,9.11199999999997));
#25415=CARTESIAN_POINT('Ctrl Pts',(-16.8685283942094,14.7098797632096,9.0703333333333));
#25416=CARTESIAN_POINT('Ctrl Pts',(-16.4123522628062,13.9197595264192,9.02866666666664));
#25417=CARTESIAN_POINT('Ctrl Pts',(-15.5,13.9197595264192,8.98699999999997));
#25418=CARTESIAN_POINT('Ctrl Pts',(-14.5876477371938,13.9197595264192,8.9453333333333));
#25419=CARTESIAN_POINT('Ctrl Pts',(-14.1314716057906,14.7098797632096,8.90366666666664));
#25420=CARTESIAN_POINT('Ctrl Pts',(-13.6752954743875,15.5,8.86199999999997));
#25421=CARTESIAN_POINT('Ctrl Pts',(-14.1314716057906,16.2901202367904,8.8203333333333));
#25422=CARTESIAN_POINT('Ctrl Pts',(-14.5876477371938,17.0802404735808,8.77866666666663));
#25423=CARTESIAN_POINT('Ctrl Pts',(-15.5,17.0802404735808,8.73699999999997));
#25424=CARTESIAN_POINT('Ctrl Pts',(-16.4123522628062,17.0802404735808,8.6953333333333));
#25425=CARTESIAN_POINT('Ctrl Pts',(-16.8685283942094,16.2901202367904,8.65366666666663));
#25426=CARTESIAN_POINT('Ctrl Pts',(-17.3247045256125,15.5,8.61199999999996));
#25427=CARTESIAN_POINT('Ctrl Pts',(-16.8685283942094,14.7098797632096,8.57033333333329));
#25428=CARTESIAN_POINT('Ctrl Pts',(-16.4123522628062,13.9197595264192,8.52866666666663));
#25429=CARTESIAN_POINT('Ctrl Pts',(-15.5,13.9197595264192,8.48699999999996));
#25430=CARTESIAN_POINT('Ctrl Pts',(-14.5876477371938,13.9197595264192,8.44533333333329));
#25431=CARTESIAN_POINT('Ctrl Pts',(-14.1314716057906,14.7098797632096,8.40366666666663));
#25432=CARTESIAN_POINT('Ctrl Pts',(-13.6752954743875,15.5,8.36199999999996));
#25433=CARTESIAN_POINT('Ctrl Pts',(-14.1314716057906,16.2901202367904,8.32033333333329));
#25434=CARTESIAN_POINT('Ctrl Pts',(-14.5876477371938,17.0802404735808,8.27866666666663));
#25435=CARTESIAN_POINT('Ctrl Pts',(-15.5,17.0802404735808,8.23699999999996));
#25436=CARTESIAN_POINT('Ctrl Pts',(-16.4123522628062,17.0802404735808,8.19533333333329));
#25437=CARTESIAN_POINT('Ctrl Pts',(-16.8685283942094,16.2901202367904,8.15366666666663));
#25438=CARTESIAN_POINT('Ctrl Pts',(-17.3247045256125,15.5,8.11199999999996));
#25439=CARTESIAN_POINT('Ctrl Pts',(-16.8685283942094,14.7098797632096,8.07033333333329));
#25440=CARTESIAN_POINT('Ctrl Pts',(-16.4123522628062,13.9197595264192,8.02866666666662));
#25441=CARTESIAN_POINT('Ctrl Pts',(-15.5,13.9197595264192,7.98699999999996));
#25442=CARTESIAN_POINT('Ctrl Pts',(-14.5876477371938,13.9197595264192,7.94533333333329));
#25443=CARTESIAN_POINT('Ctrl Pts',(-14.1314716057906,14.7098797632096,7.90366666666662));
#25444=CARTESIAN_POINT('Ctrl Pts',(-13.6752954743875,15.5,7.86199999999995));
#25445=CARTESIAN_POINT('Ctrl Pts',(-14.1314716057906,16.2901202367904,7.82033333333329));
#25446=CARTESIAN_POINT('Ctrl Pts',(-14.5876477371938,17.0802404735808,7.77866666666662));
#25447=CARTESIAN_POINT('Ctrl Pts',(-15.5,17.0802404735808,7.73699999999995));
#25448=CARTESIAN_POINT('Ctrl Pts',(-16.4123522628062,17.0802404735808,7.69533333333329));
#25449=CARTESIAN_POINT('Ctrl Pts',(-16.8685283942094,16.2901202367904,7.65366666666662));
#25450=CARTESIAN_POINT('Ctrl Pts',(-17.3247045256125,15.5,7.61199999999995));
#25451=CARTESIAN_POINT('Ctrl Pts',(-16.8685283942094,14.7098797632096,7.57033333333328));
#25452=CARTESIAN_POINT('Ctrl Pts',(-16.4123522628062,13.9197595264192,7.52866666666661));
#25453=CARTESIAN_POINT('Ctrl Pts',(-15.5,13.9197595264192,7.48699999999995));
#25454=CARTESIAN_POINT('Ctrl Pts',(-14.5876477371938,13.9197595264192,7.44533333333328));
#25455=CARTESIAN_POINT('Ctrl Pts',(-14.1314716057906,14.7098797632096,7.40366666666661));
#25456=CARTESIAN_POINT('Ctrl Pts',(-13.6752954743875,15.5,7.36199999999995));
#25457=CARTESIAN_POINT('Ctrl Pts',(-14.1314716057906,16.2901202367904,7.32033333333328));
#25458=CARTESIAN_POINT('Ctrl Pts',(-14.5876477371938,17.0802404735808,7.27866666666661));
#25459=CARTESIAN_POINT('Ctrl Pts',(-15.5,17.0802404735808,7.23699999999995));
#25460=CARTESIAN_POINT('Ctrl Pts',(-16.4123522628062,17.0802404735808,7.19533333333328));
#25461=CARTESIAN_POINT('Ctrl Pts',(-16.8685283942094,16.2901202367904,7.15366666666661));
#25462=CARTESIAN_POINT('Ctrl Pts',(-17.3247045256125,15.5,7.11199999999994));
#25463=CARTESIAN_POINT('Ctrl Pts',(-16.8685283942094,14.7098797632096,7.07033333333328));
#25464=CARTESIAN_POINT('Ctrl Pts',(-16.4123522628062,13.9197595264192,7.02866666666661));
#25465=CARTESIAN_POINT('Ctrl Pts',(-15.5,13.9197595264192,6.98699999999994));
#25466=CARTESIAN_POINT('Ctrl Pts',(-14.5876477371938,13.9197595264192,6.94533333333327));
#25467=CARTESIAN_POINT('Ctrl Pts',(-14.1314716057906,14.7098797632096,6.90366666666661));
#25468=CARTESIAN_POINT('Ctrl Pts',(-13.6752954743875,15.5,6.86199999999994));
#25469=CARTESIAN_POINT('Ctrl Pts',(-14.1314716057906,16.2901202367904,6.82033333333327));
#25470=CARTESIAN_POINT('Ctrl Pts',(-14.5876477371938,17.0802404735808,6.77866666666661));
#25471=CARTESIAN_POINT('Ctrl Pts',(-15.5,17.0802404735808,6.73699999999994));
#25472=CARTESIAN_POINT('Ctrl Pts',(-16.4123522628062,17.0802404735808,6.69533333333327));
#25473=CARTESIAN_POINT('Ctrl Pts',(-16.8685283942094,16.2901202367904,6.65366666666661));
#25474=CARTESIAN_POINT('Ctrl Pts',(-17.3247045256125,15.5,6.61199999999994));
#25475=CARTESIAN_POINT('Ctrl Pts',(-16.8685283942094,14.7098797632096,6.57033333333327));
#25476=CARTESIAN_POINT('Ctrl Pts',(-16.4123522628062,13.9197595264192,6.5286666666666));
#25477=CARTESIAN_POINT('Ctrl Pts',(-15.5,13.9197595264192,6.48699999999994));
#25478=CARTESIAN_POINT('Ctrl Pts',(-14.5876477371938,13.9197595264192,6.44533333333327));
#25479=CARTESIAN_POINT('Ctrl Pts',(-14.1314716057906,14.7098797632096,6.4036666666666));
#25480=CARTESIAN_POINT('Ctrl Pts',(-13.6752954743875,15.5,6.36199999999993));
#25481=CARTESIAN_POINT('Ctrl Pts',(-14.1314716057906,16.2901202367904,6.32033333333327));
#25482=CARTESIAN_POINT('Ctrl Pts',(-14.5876477371938,17.0802404735808,6.2786666666666));
#25483=CARTESIAN_POINT('Ctrl Pts',(-15.5,17.0802404735808,6.23699999999993));
#25484=CARTESIAN_POINT('Ctrl Pts',(-16.4123522628062,17.0802404735808,6.19533333333326));
#25485=CARTESIAN_POINT('Ctrl Pts',(-16.8685283942094,16.2901202367904,6.1536666666666));
#25486=CARTESIAN_POINT('Ctrl Pts',(-17.3247045256125,15.5,6.11199999999993));
#25487=CARTESIAN_POINT('Ctrl Pts',(-16.8685283942094,14.7098797632096,6.07033333333326));
#25488=CARTESIAN_POINT('Ctrl Pts',(-16.4123522628062,13.9197595264192,6.0286666666666));
#25489=CARTESIAN_POINT('Ctrl Pts',(-15.5,13.9197595264192,5.98699999999993));
#25490=CARTESIAN_POINT('Ctrl Pts',(-14.5876477371938,13.9197595264192,5.94533333333326));
#25491=CARTESIAN_POINT('Ctrl Pts',(-14.1314716057906,14.7098797632096,5.9036666666666));
#25492=CARTESIAN_POINT('Ctrl Pts',(-13.6752954743875,15.5,5.86199999999993));
#25493=CARTESIAN_POINT('Ctrl Pts',(-14.1314716057906,16.2901202367904,5.82033333333326));
#25494=CARTESIAN_POINT('Ctrl Pts',(-14.5876477371938,17.0802404735808,5.77866666666659));
#25495=CARTESIAN_POINT('Ctrl Pts',(-15.5,17.0802404735808,5.73699999999993));
#25496=CARTESIAN_POINT('Ctrl Pts',(-16.4123522628062,17.0802404735808,5.69533333333326));
#25497=CARTESIAN_POINT('Ctrl Pts',(-16.8685283942094,16.2901202367904,5.65366666666659));
#25498=CARTESIAN_POINT('Ctrl Pts',(-17.3247045256125,15.5,5.61199999999992));
#25499=CARTESIAN_POINT('Ctrl Pts',(-16.8685283942094,14.7098797632096,5.57033333333326));
#25500=CARTESIAN_POINT('Ctrl Pts',(-16.4123522628062,13.9197595264192,5.52866666666659));
#25501=CARTESIAN_POINT('Ctrl Pts',(-15.5,13.9197595264192,5.48699999999992));
#25502=CARTESIAN_POINT('Ctrl Pts',(-14.5876477371938,13.9197595264192,5.44533333333326));
#25503=CARTESIAN_POINT('Ctrl Pts',(-14.1314716057906,14.7098797632096,5.40366666666659));
#25504=CARTESIAN_POINT('Ctrl Pts',(-13.6752954743875,15.5,5.36199999999992));
#25505=CARTESIAN_POINT('Ctrl Pts',(-14.1314716057906,16.2901202367904,5.32033333333325));
#25506=CARTESIAN_POINT('Ctrl Pts',(-14.5876477371938,17.0802404735808,5.27866666666659));
#25507=CARTESIAN_POINT('Ctrl Pts',(-15.5,17.0802404735808,5.23699999999992));
#25508=CARTESIAN_POINT('Ctrl Pts',(-16.4123522628062,17.0802404735808,5.19533333333325));
#25509=CARTESIAN_POINT('Ctrl Pts',(-16.8685283942094,16.2901202367904,5.15366666666658));
#25510=CARTESIAN_POINT('Ctrl Pts',(-17.3247045256125,15.5,5.11199999999992));
#25511=CARTESIAN_POINT('Ctrl Pts',(-16.8685283942094,14.7098797632096,5.07033333333325));
#25512=CARTESIAN_POINT('Ctrl Pts',(-16.4123522628062,13.9197595264192,5.02866666666658));
#25513=CARTESIAN_POINT('Ctrl Pts',(-15.5,13.9197595264192,4.98699999999992));
#25514=CARTESIAN_POINT('Ctrl Pts',(-14.5876477371938,13.9197595264192,4.94533333333325));
#25515=CARTESIAN_POINT('Ctrl Pts',(-14.1314716057906,14.7098797632096,4.90366666666658));
#25516=CARTESIAN_POINT('Ctrl Pts',(-13.6752954743875,15.5,4.86199999999991));
#25517=CARTESIAN_POINT('Ctrl Pts',(-14.1314716057906,16.2901202367904,4.82033333333325));
#25518=CARTESIAN_POINT('Ctrl Pts',(-14.5876477371938,17.0802404735808,4.77866666666658));
#25519=CARTESIAN_POINT('Ctrl Pts',(-15.5,17.0802404735808,4.73699999999991));
#25520=CARTESIAN_POINT('Ctrl Pts',(-16.4123522628062,17.0802404735808,4.69533333333325));
#25521=CARTESIAN_POINT('Ctrl Pts',(-16.8685283942094,16.2901202367904,4.65366666666658));
#25522=CARTESIAN_POINT('Ctrl Pts',(-17.3247045256125,15.5,4.61199999999991));
#25523=CARTESIAN_POINT('Ctrl Pts',(-16.8685283942094,14.7098797632096,4.57033333333324));
#25524=CARTESIAN_POINT('Ctrl Pts',(-16.4123522628062,13.9197595264192,4.52866666666658));
#25525=CARTESIAN_POINT('Ctrl Pts',(-15.5,13.9197595264192,4.48699999999991));
#25526=CARTESIAN_POINT('Ctrl Pts',(-14.5876477371938,13.9197595264192,4.44533333333324));
#25527=CARTESIAN_POINT('Ctrl Pts',(-14.1314716057906,14.7098797632096,4.40366666666658));
#25528=CARTESIAN_POINT('Ctrl Pts',(-13.6752954743875,15.5,4.36199999999991));
#25529=CARTESIAN_POINT('Ctrl Pts',(-14.1314716057906,16.2901202367904,4.32033333333324));
#25530=CARTESIAN_POINT('Ctrl Pts',(-14.5876477371938,17.0802404735808,4.27866666666657));
#25531=CARTESIAN_POINT('Ctrl Pts',(-15.5,17.0802404735808,4.23699999999991));
#25532=CARTESIAN_POINT('Ctrl Pts',(-16.4123522628062,17.0802404735808,4.19533333333324));
#25533=CARTESIAN_POINT('Ctrl Pts',(-16.8685283942094,16.2901202367904,4.15366666666657));
#25534=CARTESIAN_POINT('Ctrl Pts',(-17.3247045256125,15.5,4.1119999999999));
#25535=CARTESIAN_POINT('Ctrl Pts',(-16.8685283942094,14.7098797632096,4.07033333333324));
#25536=CARTESIAN_POINT('Ctrl Pts',(-16.4123522628062,13.9197595264192,4.02866666666657));
#25537=CARTESIAN_POINT('Ctrl Pts',(-15.5,13.9197595264192,3.9869999999999));
#25538=CARTESIAN_POINT('Ctrl Pts',(-14.5876477371938,13.9197595264192,3.94533333333323));
#25539=CARTESIAN_POINT('Ctrl Pts',(-14.1314716057906,14.7098797632096,3.90366666666657));
#25540=CARTESIAN_POINT('Ctrl Pts',(-13.6752954743875,15.5,3.8619999999999));
#25541=CARTESIAN_POINT('Ctrl Pts',(-14.1314716057906,16.2901202367904,3.82033333333323));
#25542=CARTESIAN_POINT('Ctrl Pts',(-14.5876477371938,17.0802404735808,3.77866666666657));
#25543=CARTESIAN_POINT('Ctrl Pts',(-15.5,17.0802404735808,3.7369999999999));
#25544=CARTESIAN_POINT('Ctrl Pts',(-16.4123522628062,17.0802404735808,3.69533333333323));
#25545=CARTESIAN_POINT('Ctrl Pts',(-16.8685283942094,16.2901202367904,3.65366666666656));
#25546=CARTESIAN_POINT('Ctrl Pts',(-17.3247045256125,15.5,3.6119999999999));
#25547=CARTESIAN_POINT('Ctrl Pts',(-16.8685283942094,14.7098797632096,3.57033333333323));
#25548=CARTESIAN_POINT('Ctrl Pts',(-16.4123522628062,13.9197595264192,3.52866666666656));
#25549=CARTESIAN_POINT('Ctrl Pts',(-15.5,13.9197595264192,3.4869999999999));
#25550=CARTESIAN_POINT('Ctrl Pts',(-14.5876477371938,13.9197595264192,3.44533333333323));
#25551=CARTESIAN_POINT('Ctrl Pts',(-14.1314716057906,14.7098797632096,3.40366666666656));
#25552=CARTESIAN_POINT('Ctrl Pts',(-13.6752954743875,15.5,3.36199999999989));
#25553=CARTESIAN_POINT('Ctrl Pts',(-14.1314716057906,16.2901202367904,3.32033333333323));
#25554=CARTESIAN_POINT('Ctrl Pts',(-14.5876477371938,17.0802404735808,3.27866666666656));
#25555=CARTESIAN_POINT('Ctrl Pts',(-15.5,17.0802404735808,3.23699999999989));
#25556=CARTESIAN_POINT('Ctrl Pts',(-16.4123522628062,17.0802404735808,3.19533333333323));
#25557=CARTESIAN_POINT('Ctrl Pts',(-16.8685283942094,16.2901202367904,3.15366666666656));
#25558=CARTESIAN_POINT('Ctrl Pts',(-17.3247045256125,15.5,3.11199999999989));
#25559=CARTESIAN_POINT('Ctrl Pts',(-16.8685283942094,14.7098797632096,3.07033333333322));
#25560=CARTESIAN_POINT('Ctrl Pts',(-16.4123522628062,13.9197595264192,3.02866666666656));
#25561=CARTESIAN_POINT('Ctrl Pts',(-15.5,13.9197595264192,2.98699999999989));
#25562=CARTESIAN_POINT('Ctrl Pts',(-14.5876477371938,13.9197595264192,2.94533333333322));
#25563=CARTESIAN_POINT('Ctrl Pts',(-14.1314716057906,14.7098797632096,2.90366666666656));
#25564=CARTESIAN_POINT('Ctrl Pts',(-13.6752954743875,15.5,2.86199999999989));
#25565=CARTESIAN_POINT('Ctrl Pts',(-14.1314716057906,16.2901202367904,2.82033333333322));
#25566=CARTESIAN_POINT('Ctrl Pts',(-14.5876477371938,17.0802404735808,2.77866666666655));
#25567=CARTESIAN_POINT('Ctrl Pts',(-15.5,17.0802404735808,2.73699999999989));
#25568=CARTESIAN_POINT('Ctrl Pts',(-16.4123522628062,17.0802404735808,2.69533333333322));
#25569=CARTESIAN_POINT('Ctrl Pts',(-16.8685283942094,16.2901202367904,2.65366666666655));
#25570=CARTESIAN_POINT('Ctrl Pts',(-17.3247045256125,15.5,2.61199999999988));
#25571=CARTESIAN_POINT('Ctrl Pts',(-16.8685283942094,14.7098797632096,2.57033333333322));
#25572=CARTESIAN_POINT('Ctrl Pts',(-16.4123522628062,13.9197595264192,2.52866666666655));
#25573=CARTESIAN_POINT('Ctrl Pts',(-15.5,13.9197595264192,2.48699999999988));
#25574=CARTESIAN_POINT('Ctrl Pts',(-14.5876477371938,13.9197595264192,2.44533333333321));
#25575=CARTESIAN_POINT('Ctrl Pts',(-14.1314716057906,14.7098797632096,2.40366666666655));
#25576=CARTESIAN_POINT('Ctrl Pts',(-13.6752954743875,15.5,2.36199999999988));
#25577=CARTESIAN_POINT('Ctrl Pts',(-14.1314716057906,16.2901202367904,2.32033333333321));
#25578=CARTESIAN_POINT('Ctrl Pts',(-14.5876477371938,17.0802404735808,2.27866666666655));
#25579=CARTESIAN_POINT('Ctrl Pts',(-15.5,17.0802404735808,2.23699999999988));
#25580=CARTESIAN_POINT('Ctrl Pts',(-16.4123522628062,17.0802404735808,2.19533333333321));
#25581=CARTESIAN_POINT('Ctrl Pts',(-16.8685283942094,16.2901202367904,2.15366666666655));
#25582=CARTESIAN_POINT('Ctrl Pts',(-17.3247045256125,15.5,2.11199999999988));
#25583=CARTESIAN_POINT('Ctrl Pts',(-16.8685283942094,14.7098797632096,2.07033333333321));
#25584=CARTESIAN_POINT('Ctrl Pts',(-16.4123522628062,13.9197595264192,2.02866666666654));
#25585=CARTESIAN_POINT('Ctrl Pts',(-15.5,13.9197595264192,1.98699999999988));
#25586=CARTESIAN_POINT('Ctrl Pts',(-14.5876477371938,13.9197595264192,1.94533333333321));
#25587=CARTESIAN_POINT('Ctrl Pts',(-14.1314716057906,14.7098797632096,1.90366666666654));
#25588=CARTESIAN_POINT('Ctrl Pts',(-13.6752954743875,15.5,1.86199999999987));
#25589=CARTESIAN_POINT('Ctrl Pts',(-14.1314716057906,16.2901202367904,1.82033333333321));
#25590=CARTESIAN_POINT('Ctrl Pts',(-14.5876477371938,17.0802404735808,1.77866666666654));
#25591=CARTESIAN_POINT('Ctrl Pts',(-15.5,17.0802404735808,1.73699999999987));
#25592=CARTESIAN_POINT('Ctrl Pts',(-16.4123522628062,17.0802404735808,1.6953333333332));
#25593=CARTESIAN_POINT('Ctrl Pts',(-16.8685283942094,16.2901202367904,1.65366666666654));
#25594=CARTESIAN_POINT('Ctrl Pts',(-17.3247045256125,15.5,1.61199999999987));
#25595=CARTESIAN_POINT('Ctrl Pts',(-16.8685283942094,14.7098797632096,1.5703333333332));
#25596=CARTESIAN_POINT('Ctrl Pts',(-16.4123522628062,13.9197595264192,1.52866666666654));
#25597=CARTESIAN_POINT('Ctrl Pts',(-15.5,13.9197595264192,1.48699999999987));
#25598=CARTESIAN_POINT('Ctrl Pts',(-14.5876477371938,13.9197595264192,1.4453333333332));
#25599=CARTESIAN_POINT('Ctrl Pts',(-14.1314716057906,14.7098797632096,1.40366666666653));
#25600=CARTESIAN_POINT('Ctrl Pts',(-13.6752954743875,15.5,1.36199999999987));
#25601=CARTESIAN_POINT('Ctrl Pts',(-14.1314716057906,16.2901202367904,1.3203333333332));
#25602=CARTESIAN_POINT('Ctrl Pts',(-14.5876477371938,17.0802404735808,1.27866666666653));
#25603=CARTESIAN_POINT('Ctrl Pts',(-15.5,17.0802404735808,1.23699999999987));
#25604=CARTESIAN_POINT('Ctrl Pts',(-16.4123522628062,17.0802404735808,1.1953333333332));
#25605=CARTESIAN_POINT('Ctrl Pts',(-16.8685283942094,16.2901202367904,1.15366666666653));
#25606=CARTESIAN_POINT('Ctrl Pts',(-17.3247045256125,15.5,1.11199999999986));
#25607=CARTESIAN_POINT('Ctrl Pts',(-16.8685283942094,14.7098797632096,1.0703333333332));
#25608=CARTESIAN_POINT('Ctrl Pts',(-16.4123522628062,13.9197595264192,1.02866666666653));
#25609=CARTESIAN_POINT('Ctrl Pts',(-15.5,13.9197595264192,0.986999999999863));
#25610=CARTESIAN_POINT('Ctrl Pts',(-14.5876477371938,13.9197595264192,0.945333333333196));
#25611=CARTESIAN_POINT('Ctrl Pts',(-14.1314716057906,14.7098797632096,0.903666666666529));
#25612=CARTESIAN_POINT('Ctrl Pts',(-13.6752954743875,15.5,0.861999999999861));
#25613=CARTESIAN_POINT('Ctrl Pts',(-14.1314716057906,16.2901202367904,0.820333333333194));
#25614=CARTESIAN_POINT('Ctrl Pts',(-14.5876477371938,17.0802404735808,0.778666666666527));
#25615=CARTESIAN_POINT('Ctrl Pts',(-15.5,17.0802404735808,0.736999999999859));
#25616=CARTESIAN_POINT('Ctrl Pts',(-16.4123522628062,17.0802404735808,0.695333333333192));
#25617=CARTESIAN_POINT('Ctrl Pts',(-16.8685283942094,16.2901202367904,0.653666666666525));
#25618=CARTESIAN_POINT('Ctrl Pts',(-17.3247045256125,15.5,0.611999999999857));
#25619=CARTESIAN_POINT('Ctrl Pts',(-16.8685283942094,14.7098797632096,0.57033333333319));
#25620=CARTESIAN_POINT('Ctrl Pts',(-16.4123522628062,13.9197595264192,0.528666666666523));
#25621=CARTESIAN_POINT('Ctrl Pts',(-15.5,13.9197595264192,0.486999999999856));
#25622=CARTESIAN_POINT('Ctrl Pts',(-14.5876477371938,13.9197595264192,0.445333333333188));
#25623=CARTESIAN_POINT('Ctrl Pts',(-14.1314716057906,14.7098797632096,0.403666666666521));
#25624=CARTESIAN_POINT('Ctrl Pts',(-13.6752954743875,15.5,0.361999999999854));
#25625=CARTESIAN_POINT('Ctrl Pts',(-14.1314716057906,16.2901202367904,0.320333333333186));
#25626=CARTESIAN_POINT('Ctrl Pts',(-14.5876477371938,17.0802404735808,0.278666666666519));
#25627=CARTESIAN_POINT('Ctrl Pts',(-15.5,17.0802404735808,0.236999999999852));
#25628=CARTESIAN_POINT('Ctrl Pts',(-16.4123522628062,17.0802404735808,0.195333333333185));
#25629=CARTESIAN_POINT('Ctrl Pts',(-16.8685283942094,16.2901202367904,0.153666666666517));
#25630=CARTESIAN_POINT('Ctrl Pts',(-17.3247045256125,15.5,0.11199999999985));
#25631=CARTESIAN_POINT('Ctrl Pts',(-16.8685283942094,14.7098797632096,0.0703333333331828));
#25632=CARTESIAN_POINT('Ctrl Pts',(-16.4123522628062,13.9197595264192,0.0286666666665155));
#25633=CARTESIAN_POINT('Ctrl Pts',(-15.5,13.9197595264192,-0.0130000000001518));
#25634=CARTESIAN_POINT('Ctrl Pts',(-14.5876477371938,13.9197595264192,-0.0546666666668173));
#25635=CARTESIAN_POINT('Ctrl Pts',(-14.1314716057906,14.7098797632096,-0.0963333333334846));
#25636=CARTESIAN_POINT('Ctrl Pts',(-13.6752954743875,15.5,-0.138000000000152));
#25637=CARTESIAN_POINT('Ctrl Pts',(-14.1314716057906,16.2901202367904,-0.179666666666819));
#25638=CARTESIAN_POINT('Ctrl Pts',(-14.5876477371938,17.0802404735808,-0.221333333333486));
#25639=CARTESIAN_POINT('Ctrl Pts',(-15.5,17.0802404735808,-0.263000000000154));
#25640=CARTESIAN_POINT('Ctrl Pts',(-16.4123522628062,17.0802404735808,-0.304666666666821));
#25641=CARTESIAN_POINT('Ctrl Pts',(-16.8685283942094,16.2901202367904,-0.346333333333488));
#25642=CARTESIAN_POINT('Ctrl Pts',(-17.3247045256125,15.5,-0.388000000000156));
#25643=CARTESIAN_POINT('Ctrl Pts',(-16.8685283942094,14.7098797632096,-0.429666666666823));
#25644=CARTESIAN_POINT('Ctrl Pts',(-16.4123522628062,13.9197595264192,-0.47133333333349));
#25645=CARTESIAN_POINT('Ctrl Pts',(-15.5,13.9197595264192,-0.513000000000157));
#25646=CARTESIAN_POINT('Ctrl Pts',(-14.5876477371938,13.9197595264192,-0.554666666666825));
#25647=CARTESIAN_POINT('Ctrl Pts',(-14.1314716057906,14.7098797632096,-0.596333333333492));
#25648=CARTESIAN_POINT('Ctrl Pts',(-13.6752954743875,15.5,-0.638000000000159));
#25649=CARTESIAN_POINT('Ctrl Pts',(-14.1314716057906,16.2901202367904,-0.679666666666827));
#25650=CARTESIAN_POINT('Ctrl Pts',(-14.5876477371938,17.0802404735808,-0.721333333333494));
#25651=CARTESIAN_POINT('Ctrl Pts',(-15.5,17.0802404735808,-0.763000000000161));
#25652=CARTESIAN_POINT('Ctrl Pts',(-16.4123522628062,17.0802404735808,-0.804666666666829));
#25653=CARTESIAN_POINT('Ctrl Pts',(-16.8685283942094,16.2901202367904,-0.846333333333496));
#25654=CARTESIAN_POINT('Ctrl Pts',(-17.3247045256125,15.5,-0.888000000000163));
#25655=CARTESIAN_POINT('Ctrl Pts',(-16.8685283942094,14.7098797632096,-0.92966666666683));
#25656=CARTESIAN_POINT('Ctrl Pts',(-16.4123522628062,13.9197595264192,-0.971333333333497));
#25657=CARTESIAN_POINT('Ctrl Pts',(-15.5,13.9197595264192,-1.01300000000016));
#25658=CARTESIAN_POINT('Ctrl Pts',(-14.5876477371938,13.9197595264192,-1.05466666666683));
#25659=CARTESIAN_POINT('Ctrl Pts',(-14.1314716057906,14.7098797632096,-1.0963333333335));
#25660=CARTESIAN_POINT('Ctrl Pts',(-13.6752954743875,15.5,-1.13800000000017));
#25661=CARTESIAN_POINT('Ctrl Pts',(-14.1314716057906,16.2901202367904,-1.17966666666683));
#25662=CARTESIAN_POINT('Ctrl Pts',(-14.5876477371938,17.0802404735808,-1.2213333333335));
#25663=CARTESIAN_POINT('Ctrl Pts',(-15.5,17.0802404735808,-1.26300000000017));
#25664=CARTESIAN_POINT('Ctrl Pts',(-16.4123522628062,17.0802404735808,-1.30466666666683));
#25665=CARTESIAN_POINT('Ctrl Pts',(-16.8685283942094,16.2901202367904,-1.3463333333335));
#25666=CARTESIAN_POINT('Ctrl Pts',(-17.3247045256125,15.5,-1.38800000000017));
#25667=CARTESIAN_POINT('Ctrl Pts',(-16.8685283942094,14.7098797632096,-1.42966666666684));
#25668=CARTESIAN_POINT('Ctrl Pts',(-16.4123522628062,13.9197595264192,-1.4713333333335));
#25669=CARTESIAN_POINT('Ctrl Pts',(-15.5,13.9197595264192,-1.51300000000017));
#25670=CARTESIAN_POINT('Ctrl Pts',(-14.5876477371938,13.9197595264192,-1.55466666666684));
#25671=CARTESIAN_POINT('Ctrl Pts',(-14.1314716057906,14.7098797632096,-1.59633333333351));
#25672=CARTESIAN_POINT('Ctrl Pts',(-13.6752954743875,15.5,-1.63800000000017));
#25673=CARTESIAN_POINT('Ctrl Pts',(-14.1314716057906,16.2901202367904,-1.67966666666684));
#25674=CARTESIAN_POINT('Ctrl Pts',(-14.5876477371938,17.0802404735808,-1.72133333333351));
#25675=CARTESIAN_POINT('Ctrl Pts',(-15.5,17.0802404735808,-1.76300000000017));
#25676=CARTESIAN_POINT('Ctrl Pts',(-16.4123522628062,17.0802404735808,-1.80466666666684));
#25677=CARTESIAN_POINT('Ctrl Pts',(-16.8685283942094,16.2901202367904,-1.84633333333351));
#25678=CARTESIAN_POINT('Ctrl Pts',(-17.3247045256125,15.5,-1.88800000000018));
#25679=CARTESIAN_POINT('Ctrl Pts',(-16.8685283942094,14.7098797632096,-1.92966666666684));
#25680=CARTESIAN_POINT('Ctrl Pts',(-16.7005797757653,14.4189842230035,-1.94500692368624));
#25681=CARTESIAN_POINT('Ctrl Pts',(-16.428831587743,14.221551003773,-1.96262330599533));
#25682=CARTESIAN_POINT('Origin',(-15.6296099418937,15.4374167911874,1.3857776251332));
#25683=CARTESIAN_POINT('',(-16.4288315898516,14.2215509627457,-1.96262324188451));
#25684=CARTESIAN_POINT('',(-16.4288304039466,14.2215500160357,-1.96262332703658));
#25685=CARTESIAN_POINT('Ctrl Pts',(-14.2313898004749,14.5577749122403,10.4122404735808));
#25686=CARTESIAN_POINT('Ctrl Pts',(-14.1770441521709,14.6309457974488,10.407829216981));
#25687=CARTESIAN_POINT('Ctrl Pts',(-14.1314716057906,14.7098797632096,10.4036666666667));
#25688=CARTESIAN_POINT('Ctrl Pts',(-13.6752954743875,15.5,10.362));
#25689=CARTESIAN_POINT('Ctrl Pts',(-14.1314716057906,16.2901202367904,10.3203333333333));
#25690=CARTESIAN_POINT('Ctrl Pts',(-14.5876477371938,17.0802404735808,10.2786666666667));
#25691=CARTESIAN_POINT('Ctrl Pts',(-15.5,17.0802404735808,10.237));
#25692=CARTESIAN_POINT('Ctrl Pts',(-16.4123522628062,17.0802404735808,10.1953333333333));
#25693=CARTESIAN_POINT('Ctrl Pts',(-16.8685283942094,16.2901202367904,10.1536666666667));
#25694=CARTESIAN_POINT('Ctrl Pts',(-17.3247045256125,15.5,10.112));
#25695=CARTESIAN_POINT('Ctrl Pts',(-16.8685283942094,14.7098797632096,10.0703333333333));
#25696=CARTESIAN_POINT('Ctrl Pts',(-16.4123522628062,13.9197595264192,10.0286666666667));
#25697=CARTESIAN_POINT('Ctrl Pts',(-15.5,13.9197595264192,9.98699999999998));
#25698=CARTESIAN_POINT('Ctrl Pts',(-14.5876477371938,13.9197595264192,9.94533333333331));
#25699=CARTESIAN_POINT('Ctrl Pts',(-14.1314716057906,14.7098797632096,9.90366666666665));
#25700=CARTESIAN_POINT('Ctrl Pts',(-13.6752954743875,15.5,9.86199999999998));
#25701=CARTESIAN_POINT('Ctrl Pts',(-14.1314716057906,16.2901202367904,9.82033333333331));
#25702=CARTESIAN_POINT('Ctrl Pts',(-14.5876477371938,17.0802404735808,9.77866666666665));
#25703=CARTESIAN_POINT('Ctrl Pts',(-15.5,17.0802404735808,9.73699999999998));
#25704=CARTESIAN_POINT('Ctrl Pts',(-16.4123522628062,17.0802404735808,9.69533333333331));
#25705=CARTESIAN_POINT('Ctrl Pts',(-16.8685283942094,16.2901202367904,9.65366666666664));
#25706=CARTESIAN_POINT('Ctrl Pts',(-17.3247045256125,15.5,9.61199999999998));
#25707=CARTESIAN_POINT('Ctrl Pts',(-16.8685283942094,14.7098797632096,9.57033333333331));
#25708=CARTESIAN_POINT('Ctrl Pts',(-16.4123522628062,13.9197595264192,9.52866666666664));
#25709=CARTESIAN_POINT('Ctrl Pts',(-15.5,13.9197595264192,9.48699999999998));
#25710=CARTESIAN_POINT('Ctrl Pts',(-14.5876477371938,13.9197595264192,9.44533333333331));
#25711=CARTESIAN_POINT('Ctrl Pts',(-14.1314716057906,14.7098797632096,9.40366666666664));
#25712=CARTESIAN_POINT('Ctrl Pts',(-13.6752954743875,15.5,9.36199999999998));
#25713=CARTESIAN_POINT('Ctrl Pts',(-14.1314716057906,16.2901202367904,9.32033333333331));
#25714=CARTESIAN_POINT('Ctrl Pts',(-14.5876477371938,17.0802404735808,9.27866666666664));
#25715=CARTESIAN_POINT('Ctrl Pts',(-15.5,17.0802404735808,9.23699999999997));
#25716=CARTESIAN_POINT('Ctrl Pts',(-16.4123522628062,17.0802404735808,9.19533333333331));
#25717=CARTESIAN_POINT('Ctrl Pts',(-16.8685283942094,16.2901202367904,9.15366666666664));
#25718=CARTESIAN_POINT('Ctrl Pts',(-17.3247045256125,15.5,9.11199999999997));
#25719=CARTESIAN_POINT('Ctrl Pts',(-16.8685283942094,14.7098797632096,9.0703333333333));
#25720=CARTESIAN_POINT('Ctrl Pts',(-16.4123522628062,13.9197595264192,9.02866666666664));
#25721=CARTESIAN_POINT('Ctrl Pts',(-15.5,13.9197595264192,8.98699999999997));
#25722=CARTESIAN_POINT('Ctrl Pts',(-14.5876477371938,13.9197595264192,8.9453333333333));
#25723=CARTESIAN_POINT('Ctrl Pts',(-14.1314716057906,14.7098797632096,8.90366666666664));
#25724=CARTESIAN_POINT('Ctrl Pts',(-13.6752954743875,15.5,8.86199999999997));
#25725=CARTESIAN_POINT('Ctrl Pts',(-14.1314716057906,16.2901202367904,8.8203333333333));
#25726=CARTESIAN_POINT('Ctrl Pts',(-14.5876477371938,17.0802404735808,8.77866666666663));
#25727=CARTESIAN_POINT('Ctrl Pts',(-15.5,17.0802404735808,8.73699999999997));
#25728=CARTESIAN_POINT('Ctrl Pts',(-16.4123522628062,17.0802404735808,8.6953333333333));
#25729=CARTESIAN_POINT('Ctrl Pts',(-16.8685283942094,16.2901202367904,8.65366666666663));
#25730=CARTESIAN_POINT('Ctrl Pts',(-17.3247045256125,15.5,8.61199999999996));
#25731=CARTESIAN_POINT('Ctrl Pts',(-16.8685283942094,14.7098797632096,8.57033333333329));
#25732=CARTESIAN_POINT('Ctrl Pts',(-16.4123522628062,13.9197595264192,8.52866666666663));
#25733=CARTESIAN_POINT('Ctrl Pts',(-15.5,13.9197595264192,8.48699999999996));
#25734=CARTESIAN_POINT('Ctrl Pts',(-14.5876477371938,13.9197595264192,8.44533333333329));
#25735=CARTESIAN_POINT('Ctrl Pts',(-14.1314716057906,14.7098797632096,8.40366666666663));
#25736=CARTESIAN_POINT('Ctrl Pts',(-13.6752954743875,15.5,8.36199999999996));
#25737=CARTESIAN_POINT('Ctrl Pts',(-14.1314716057906,16.2901202367904,8.32033333333329));
#25738=CARTESIAN_POINT('Ctrl Pts',(-14.5876477371938,17.0802404735808,8.27866666666663));
#25739=CARTESIAN_POINT('Ctrl Pts',(-15.5,17.0802404735808,8.23699999999996));
#25740=CARTESIAN_POINT('Ctrl Pts',(-16.4123522628062,17.0802404735808,8.19533333333329));
#25741=CARTESIAN_POINT('Ctrl Pts',(-16.8685283942094,16.2901202367904,8.15366666666663));
#25742=CARTESIAN_POINT('Ctrl Pts',(-17.3247045256125,15.5,8.11199999999996));
#25743=CARTESIAN_POINT('Ctrl Pts',(-16.8685283942094,14.7098797632096,8.07033333333329));
#25744=CARTESIAN_POINT('Ctrl Pts',(-16.4123522628062,13.9197595264192,8.02866666666662));
#25745=CARTESIAN_POINT('Ctrl Pts',(-15.5,13.9197595264192,7.98699999999996));
#25746=CARTESIAN_POINT('Ctrl Pts',(-14.5876477371938,13.9197595264192,7.94533333333329));
#25747=CARTESIAN_POINT('Ctrl Pts',(-14.1314716057906,14.7098797632096,7.90366666666662));
#25748=CARTESIAN_POINT('Ctrl Pts',(-13.6752954743875,15.5,7.86199999999995));
#25749=CARTESIAN_POINT('Ctrl Pts',(-14.1314716057906,16.2901202367904,7.82033333333329));
#25750=CARTESIAN_POINT('Ctrl Pts',(-14.5876477371938,17.0802404735808,7.77866666666662));
#25751=CARTESIAN_POINT('Ctrl Pts',(-15.5,17.0802404735808,7.73699999999995));
#25752=CARTESIAN_POINT('Ctrl Pts',(-16.4123522628062,17.0802404735808,7.69533333333329));
#25753=CARTESIAN_POINT('Ctrl Pts',(-16.8685283942094,16.2901202367904,7.65366666666662));
#25754=CARTESIAN_POINT('Ctrl Pts',(-17.3247045256125,15.5,7.61199999999995));
#25755=CARTESIAN_POINT('Ctrl Pts',(-16.8685283942094,14.7098797632096,7.57033333333328));
#25756=CARTESIAN_POINT('Ctrl Pts',(-16.4123522628062,13.9197595264192,7.52866666666662));
#25757=CARTESIAN_POINT('Ctrl Pts',(-15.5,13.9197595264192,7.48699999999995));
#25758=CARTESIAN_POINT('Ctrl Pts',(-14.5876477371938,13.9197595264192,7.44533333333328));
#25759=CARTESIAN_POINT('Ctrl Pts',(-14.1314716057906,14.7098797632096,7.40366666666661));
#25760=CARTESIAN_POINT('Ctrl Pts',(-13.6752954743875,15.5,7.36199999999995));
#25761=CARTESIAN_POINT('Ctrl Pts',(-14.1314716057906,16.2901202367904,7.32033333333328));
#25762=CARTESIAN_POINT('Ctrl Pts',(-14.5876477371938,17.0802404735808,7.27866666666661));
#25763=CARTESIAN_POINT('Ctrl Pts',(-15.5,17.0802404735808,7.23699999999995));
#25764=CARTESIAN_POINT('Ctrl Pts',(-16.4123522628062,17.0802404735808,7.19533333333328));
#25765=CARTESIAN_POINT('Ctrl Pts',(-16.8685283942094,16.2901202367904,7.15366666666661));
#25766=CARTESIAN_POINT('Ctrl Pts',(-17.3247045256125,15.5,7.11199999999994));
#25767=CARTESIAN_POINT('Ctrl Pts',(-16.8685283942094,14.7098797632096,7.07033333333328));
#25768=CARTESIAN_POINT('Ctrl Pts',(-16.4123522628062,13.9197595264192,7.02866666666661));
#25769=CARTESIAN_POINT('Ctrl Pts',(-15.5,13.9197595264192,6.98699999999994));
#25770=CARTESIAN_POINT('Ctrl Pts',(-14.5876477371938,13.9197595264192,6.94533333333327));
#25771=CARTESIAN_POINT('Ctrl Pts',(-14.1314716057906,14.7098797632096,6.90366666666661));
#25772=CARTESIAN_POINT('Ctrl Pts',(-13.6752954743875,15.5,6.86199999999994));
#25773=CARTESIAN_POINT('Ctrl Pts',(-14.1314716057906,16.2901202367904,6.82033333333327));
#25774=CARTESIAN_POINT('Ctrl Pts',(-14.5876477371938,17.0802404735808,6.77866666666661));
#25775=CARTESIAN_POINT('Ctrl Pts',(-15.5,17.0802404735808,6.73699999999994));
#25776=CARTESIAN_POINT('Ctrl Pts',(-16.4123522628062,17.0802404735808,6.69533333333327));
#25777=CARTESIAN_POINT('Ctrl Pts',(-16.8685283942094,16.2901202367904,6.65366666666661));
#25778=CARTESIAN_POINT('Ctrl Pts',(-17.3247045256125,15.5,6.61199999999994));
#25779=CARTESIAN_POINT('Ctrl Pts',(-16.8685283942094,14.7098797632096,6.57033333333327));
#25780=CARTESIAN_POINT('Ctrl Pts',(-16.4123522628062,13.9197595264192,6.5286666666666));
#25781=CARTESIAN_POINT('Ctrl Pts',(-15.5,13.9197595264192,6.48699999999994));
#25782=CARTESIAN_POINT('Ctrl Pts',(-14.5876477371938,13.9197595264192,6.44533333333327));
#25783=CARTESIAN_POINT('Ctrl Pts',(-14.1314716057906,14.7098797632096,6.4036666666666));
#25784=CARTESIAN_POINT('Ctrl Pts',(-13.6752954743875,15.5,6.36199999999993));
#25785=CARTESIAN_POINT('Ctrl Pts',(-14.1314716057906,16.2901202367904,6.32033333333327));
#25786=CARTESIAN_POINT('Ctrl Pts',(-14.5876477371938,17.0802404735808,6.2786666666666));
#25787=CARTESIAN_POINT('Ctrl Pts',(-15.5,17.0802404735808,6.23699999999993));
#25788=CARTESIAN_POINT('Ctrl Pts',(-16.4123522628062,17.0802404735808,6.19533333333326));
#25789=CARTESIAN_POINT('Ctrl Pts',(-16.8685283942094,16.2901202367904,6.1536666666666));
#25790=CARTESIAN_POINT('Ctrl Pts',(-17.3247045256125,15.5,6.11199999999993));
#25791=CARTESIAN_POINT('Ctrl Pts',(-16.8685283942094,14.7098797632096,6.07033333333326));
#25792=CARTESIAN_POINT('Ctrl Pts',(-16.4123522628062,13.9197595264192,6.0286666666666));
#25793=CARTESIAN_POINT('Ctrl Pts',(-15.5,13.9197595264192,5.98699999999993));
#25794=CARTESIAN_POINT('Ctrl Pts',(-14.5876477371938,13.9197595264192,5.94533333333326));
#25795=CARTESIAN_POINT('Ctrl Pts',(-14.1314716057906,14.7098797632096,5.9036666666666));
#25796=CARTESIAN_POINT('Ctrl Pts',(-13.6752954743875,15.5,5.86199999999993));
#25797=CARTESIAN_POINT('Ctrl Pts',(-14.1314716057906,16.2901202367904,5.82033333333326));
#25798=CARTESIAN_POINT('Ctrl Pts',(-14.5876477371938,17.0802404735808,5.77866666666659));
#25799=CARTESIAN_POINT('Ctrl Pts',(-15.5,17.0802404735808,5.73699999999993));
#25800=CARTESIAN_POINT('Ctrl Pts',(-16.4123522628062,17.0802404735808,5.69533333333326));
#25801=CARTESIAN_POINT('Ctrl Pts',(-16.8685283942094,16.2901202367904,5.65366666666659));
#25802=CARTESIAN_POINT('Ctrl Pts',(-17.3247045256125,15.5,5.61199999999992));
#25803=CARTESIAN_POINT('Ctrl Pts',(-16.8685283942094,14.7098797632096,5.57033333333326));
#25804=CARTESIAN_POINT('Ctrl Pts',(-16.4123522628062,13.9197595264192,5.52866666666659));
#25805=CARTESIAN_POINT('Ctrl Pts',(-15.5,13.9197595264192,5.48699999999992));
#25806=CARTESIAN_POINT('Ctrl Pts',(-14.5876477371938,13.9197595264192,5.44533333333326));
#25807=CARTESIAN_POINT('Ctrl Pts',(-14.1314716057906,14.7098797632096,5.40366666666659));
#25808=CARTESIAN_POINT('Ctrl Pts',(-13.6752954743875,15.5,5.36199999999992));
#25809=CARTESIAN_POINT('Ctrl Pts',(-14.1314716057906,16.2901202367904,5.32033333333325));
#25810=CARTESIAN_POINT('Ctrl Pts',(-14.5876477371938,17.0802404735808,5.27866666666659));
#25811=CARTESIAN_POINT('Ctrl Pts',(-15.5,17.0802404735808,5.23699999999992));
#25812=CARTESIAN_POINT('Ctrl Pts',(-16.4123522628062,17.0802404735808,5.19533333333325));
#25813=CARTESIAN_POINT('Ctrl Pts',(-16.8685283942094,16.2901202367904,5.15366666666658));
#25814=CARTESIAN_POINT('Ctrl Pts',(-17.3247045256125,15.5,5.11199999999992));
#25815=CARTESIAN_POINT('Ctrl Pts',(-16.8685283942094,14.7098797632096,5.07033333333325));
#25816=CARTESIAN_POINT('Ctrl Pts',(-16.4123522628062,13.9197595264192,5.02866666666658));
#25817=CARTESIAN_POINT('Ctrl Pts',(-15.5,13.9197595264192,4.98699999999992));
#25818=CARTESIAN_POINT('Ctrl Pts',(-14.5876477371938,13.9197595264192,4.94533333333325));
#25819=CARTESIAN_POINT('Ctrl Pts',(-14.1314716057906,14.7098797632096,4.90366666666658));
#25820=CARTESIAN_POINT('Ctrl Pts',(-13.6752954743875,15.5,4.86199999999991));
#25821=CARTESIAN_POINT('Ctrl Pts',(-14.1314716057906,16.2901202367904,4.82033333333325));
#25822=CARTESIAN_POINT('Ctrl Pts',(-14.5876477371938,17.0802404735808,4.77866666666658));
#25823=CARTESIAN_POINT('Ctrl Pts',(-15.5,17.0802404735808,4.73699999999991));
#25824=CARTESIAN_POINT('Ctrl Pts',(-16.4123522628062,17.0802404735808,4.69533333333325));
#25825=CARTESIAN_POINT('Ctrl Pts',(-16.8685283942094,16.2901202367904,4.65366666666658));
#25826=CARTESIAN_POINT('Ctrl Pts',(-17.3247045256125,15.5,4.61199999999991));
#25827=CARTESIAN_POINT('Ctrl Pts',(-16.8685283942094,14.7098797632096,4.57033333333324));
#25828=CARTESIAN_POINT('Ctrl Pts',(-16.4123522628062,13.9197595264192,4.52866666666658));
#25829=CARTESIAN_POINT('Ctrl Pts',(-15.5,13.9197595264192,4.48699999999991));
#25830=CARTESIAN_POINT('Ctrl Pts',(-14.5876477371938,13.9197595264192,4.44533333333324));
#25831=CARTESIAN_POINT('Ctrl Pts',(-14.1314716057906,14.7098797632096,4.40366666666658));
#25832=CARTESIAN_POINT('Ctrl Pts',(-13.6752954743875,15.5,4.36199999999991));
#25833=CARTESIAN_POINT('Ctrl Pts',(-14.1314716057906,16.2901202367904,4.32033333333324));
#25834=CARTESIAN_POINT('Ctrl Pts',(-14.5876477371938,17.0802404735808,4.27866666666657));
#25835=CARTESIAN_POINT('Ctrl Pts',(-15.5,17.0802404735808,4.23699999999991));
#25836=CARTESIAN_POINT('Ctrl Pts',(-16.4123522628062,17.0802404735808,4.19533333333324));
#25837=CARTESIAN_POINT('Ctrl Pts',(-16.8685283942094,16.2901202367904,4.15366666666657));
#25838=CARTESIAN_POINT('Ctrl Pts',(-17.3247045256125,15.5,4.1119999999999));
#25839=CARTESIAN_POINT('Ctrl Pts',(-16.8685283942094,14.7098797632096,4.07033333333324));
#25840=CARTESIAN_POINT('Ctrl Pts',(-16.4123522628062,13.9197595264192,4.02866666666657));
#25841=CARTESIAN_POINT('Ctrl Pts',(-15.5,13.9197595264192,3.9869999999999));
#25842=CARTESIAN_POINT('Ctrl Pts',(-14.5876477371938,13.9197595264192,3.94533333333323));
#25843=CARTESIAN_POINT('Ctrl Pts',(-14.1314716057906,14.7098797632096,3.90366666666657));
#25844=CARTESIAN_POINT('Ctrl Pts',(-13.6752954743875,15.5,3.8619999999999));
#25845=CARTESIAN_POINT('Ctrl Pts',(-14.1314716057906,16.2901202367904,3.82033333333323));
#25846=CARTESIAN_POINT('Ctrl Pts',(-14.5876477371938,17.0802404735808,3.77866666666657));
#25847=CARTESIAN_POINT('Ctrl Pts',(-15.5,17.0802404735808,3.7369999999999));
#25848=CARTESIAN_POINT('Ctrl Pts',(-16.4123522628062,17.0802404735808,3.69533333333323));
#25849=CARTESIAN_POINT('Ctrl Pts',(-16.8685283942094,16.2901202367904,3.65366666666656));
#25850=CARTESIAN_POINT('Ctrl Pts',(-17.3247045256125,15.5,3.6119999999999));
#25851=CARTESIAN_POINT('Ctrl Pts',(-16.8685283942094,14.7098797632096,3.57033333333323));
#25852=CARTESIAN_POINT('Ctrl Pts',(-16.4123522628062,13.9197595264192,3.52866666666656));
#25853=CARTESIAN_POINT('Ctrl Pts',(-15.5,13.9197595264192,3.4869999999999));
#25854=CARTESIAN_POINT('Ctrl Pts',(-14.5876477371938,13.9197595264192,3.44533333333323));
#25855=CARTESIAN_POINT('Ctrl Pts',(-14.1314716057906,14.7098797632096,3.40366666666656));
#25856=CARTESIAN_POINT('Ctrl Pts',(-13.6752954743875,15.5,3.36199999999989));
#25857=CARTESIAN_POINT('Ctrl Pts',(-14.1314716057906,16.2901202367904,3.32033333333323));
#25858=CARTESIAN_POINT('Ctrl Pts',(-14.5876477371938,17.0802404735808,3.27866666666656));
#25859=CARTESIAN_POINT('Ctrl Pts',(-15.5,17.0802404735808,3.23699999999989));
#25860=CARTESIAN_POINT('Ctrl Pts',(-16.4123522628062,17.0802404735808,3.19533333333323));
#25861=CARTESIAN_POINT('Ctrl Pts',(-16.8685283942094,16.2901202367904,3.15366666666656));
#25862=CARTESIAN_POINT('Ctrl Pts',(-17.3247045256125,15.5,3.11199999999989));
#25863=CARTESIAN_POINT('Ctrl Pts',(-16.8685283942094,14.7098797632096,3.07033333333322));
#25864=CARTESIAN_POINT('Ctrl Pts',(-16.4123522628062,13.9197595264192,3.02866666666656));
#25865=CARTESIAN_POINT('Ctrl Pts',(-15.5,13.9197595264192,2.98699999999989));
#25866=CARTESIAN_POINT('Ctrl Pts',(-14.5876477371938,13.9197595264192,2.94533333333322));
#25867=CARTESIAN_POINT('Ctrl Pts',(-14.1314716057906,14.7098797632096,2.90366666666656));
#25868=CARTESIAN_POINT('Ctrl Pts',(-13.6752954743875,15.5,2.86199999999989));
#25869=CARTESIAN_POINT('Ctrl Pts',(-14.1314716057906,16.2901202367904,2.82033333333322));
#25870=CARTESIAN_POINT('Ctrl Pts',(-14.5876477371938,17.0802404735808,2.77866666666655));
#25871=CARTESIAN_POINT('Ctrl Pts',(-15.5,17.0802404735808,2.73699999999989));
#25872=CARTESIAN_POINT('Ctrl Pts',(-16.4123522628062,17.0802404735808,2.69533333333322));
#25873=CARTESIAN_POINT('Ctrl Pts',(-16.8685283942094,16.2901202367904,2.65366666666655));
#25874=CARTESIAN_POINT('Ctrl Pts',(-17.3247045256125,15.5,2.61199999999988));
#25875=CARTESIAN_POINT('Ctrl Pts',(-16.8685283942094,14.7098797632096,2.57033333333322));
#25876=CARTESIAN_POINT('Ctrl Pts',(-16.4123522628062,13.9197595264192,2.52866666666655));
#25877=CARTESIAN_POINT('Ctrl Pts',(-15.5,13.9197595264192,2.48699999999988));
#25878=CARTESIAN_POINT('Ctrl Pts',(-14.5876477371938,13.9197595264192,2.44533333333321));
#25879=CARTESIAN_POINT('Ctrl Pts',(-14.1314716057906,14.7098797632096,2.40366666666655));
#25880=CARTESIAN_POINT('Ctrl Pts',(-13.6752954743875,15.5,2.36199999999988));
#25881=CARTESIAN_POINT('Ctrl Pts',(-14.1314716057906,16.2901202367904,2.32033333333321));
#25882=CARTESIAN_POINT('Ctrl Pts',(-14.5876477371938,17.0802404735808,2.27866666666655));
#25883=CARTESIAN_POINT('Ctrl Pts',(-15.5,17.0802404735808,2.23699999999988));
#25884=CARTESIAN_POINT('Ctrl Pts',(-16.4123522628062,17.0802404735808,2.19533333333321));
#25885=CARTESIAN_POINT('Ctrl Pts',(-16.8685283942094,16.2901202367904,2.15366666666655));
#25886=CARTESIAN_POINT('Ctrl Pts',(-17.3247045256125,15.5,2.11199999999988));
#25887=CARTESIAN_POINT('Ctrl Pts',(-16.8685283942094,14.7098797632096,2.07033333333321));
#25888=CARTESIAN_POINT('Ctrl Pts',(-16.4123522628062,13.9197595264192,2.02866666666654));
#25889=CARTESIAN_POINT('Ctrl Pts',(-15.5,13.9197595264192,1.98699999999988));
#25890=CARTESIAN_POINT('Ctrl Pts',(-14.5876477371938,13.9197595264192,1.94533333333321));
#25891=CARTESIAN_POINT('Ctrl Pts',(-14.1314716057906,14.7098797632096,1.90366666666654));
#25892=CARTESIAN_POINT('Ctrl Pts',(-13.6752954743875,15.5,1.86199999999987));
#25893=CARTESIAN_POINT('Ctrl Pts',(-14.1314716057906,16.2901202367904,1.82033333333321));
#25894=CARTESIAN_POINT('Ctrl Pts',(-14.5876477371938,17.0802404735808,1.77866666666654));
#25895=CARTESIAN_POINT('Ctrl Pts',(-15.5,17.0802404735808,1.73699999999987));
#25896=CARTESIAN_POINT('Ctrl Pts',(-16.4123522628062,17.0802404735808,1.6953333333332));
#25897=CARTESIAN_POINT('Ctrl Pts',(-16.8685283942094,16.2901202367904,1.65366666666654));
#25898=CARTESIAN_POINT('Ctrl Pts',(-17.3247045256125,15.5,1.61199999999987));
#25899=CARTESIAN_POINT('Ctrl Pts',(-16.8685283942094,14.7098797632096,1.5703333333332));
#25900=CARTESIAN_POINT('Ctrl Pts',(-16.4123522628062,13.9197595264192,1.52866666666654));
#25901=CARTESIAN_POINT('Ctrl Pts',(-15.5,13.9197595264192,1.48699999999987));
#25902=CARTESIAN_POINT('Ctrl Pts',(-14.5876477371938,13.9197595264192,1.4453333333332));
#25903=CARTESIAN_POINT('Ctrl Pts',(-14.1314716057906,14.7098797632096,1.40366666666653));
#25904=CARTESIAN_POINT('Ctrl Pts',(-13.6752954743875,15.5,1.36199999999987));
#25905=CARTESIAN_POINT('Ctrl Pts',(-14.1314716057906,16.2901202367904,1.3203333333332));
#25906=CARTESIAN_POINT('Ctrl Pts',(-14.5876477371938,17.0802404735808,1.27866666666653));
#25907=CARTESIAN_POINT('Ctrl Pts',(-15.5,17.0802404735808,1.23699999999987));
#25908=CARTESIAN_POINT('Ctrl Pts',(-16.4123522628062,17.0802404735808,1.1953333333332));
#25909=CARTESIAN_POINT('Ctrl Pts',(-16.8685283942094,16.2901202367904,1.15366666666653));
#25910=CARTESIAN_POINT('Ctrl Pts',(-17.3247045256125,15.5,1.11199999999986));
#25911=CARTESIAN_POINT('Ctrl Pts',(-16.8685283942094,14.7098797632096,1.0703333333332));
#25912=CARTESIAN_POINT('Ctrl Pts',(-16.4123522628062,13.9197595264192,1.02866666666653));
#25913=CARTESIAN_POINT('Ctrl Pts',(-15.5,13.9197595264192,0.986999999999863));
#25914=CARTESIAN_POINT('Ctrl Pts',(-14.5876477371938,13.9197595264192,0.945333333333196));
#25915=CARTESIAN_POINT('Ctrl Pts',(-14.1314716057906,14.7098797632096,0.903666666666529));
#25916=CARTESIAN_POINT('Ctrl Pts',(-13.6752954743875,15.5,0.861999999999861));
#25917=CARTESIAN_POINT('Ctrl Pts',(-14.1314716057906,16.2901202367904,0.820333333333194));
#25918=CARTESIAN_POINT('Ctrl Pts',(-14.5876477371938,17.0802404735808,0.778666666666527));
#25919=CARTESIAN_POINT('Ctrl Pts',(-15.5,17.0802404735808,0.736999999999859));
#25920=CARTESIAN_POINT('Ctrl Pts',(-16.4123522628062,17.0802404735808,0.695333333333192));
#25921=CARTESIAN_POINT('Ctrl Pts',(-16.8685283942094,16.2901202367904,0.653666666666525));
#25922=CARTESIAN_POINT('Ctrl Pts',(-17.3247045256125,15.5,0.611999999999858));
#25923=CARTESIAN_POINT('Ctrl Pts',(-16.8685283942094,14.7098797632096,0.57033333333319));
#25924=CARTESIAN_POINT('Ctrl Pts',(-16.4123522628062,13.9197595264192,0.528666666666523));
#25925=CARTESIAN_POINT('Ctrl Pts',(-15.5,13.9197595264192,0.486999999999856));
#25926=CARTESIAN_POINT('Ctrl Pts',(-14.5876477371938,13.9197595264192,0.445333333333188));
#25927=CARTESIAN_POINT('Ctrl Pts',(-14.1314716057906,14.7098797632096,0.403666666666521));
#25928=CARTESIAN_POINT('Ctrl Pts',(-13.6752954743875,15.5,0.361999999999854));
#25929=CARTESIAN_POINT('Ctrl Pts',(-14.1314716057906,16.2901202367904,0.320333333333186));
#25930=CARTESIAN_POINT('Ctrl Pts',(-14.5876477371938,17.0802404735808,0.278666666666519));
#25931=CARTESIAN_POINT('Ctrl Pts',(-15.5,17.0802404735808,0.236999999999852));
#25932=CARTESIAN_POINT('Ctrl Pts',(-16.4123522628062,17.0802404735808,0.195333333333185));
#25933=CARTESIAN_POINT('Ctrl Pts',(-16.8685283942094,16.2901202367904,0.153666666666517));
#25934=CARTESIAN_POINT('Ctrl Pts',(-17.3247045256125,15.5,0.11199999999985));
#25935=CARTESIAN_POINT('Ctrl Pts',(-16.8685283942094,14.7098797632096,0.0703333333331828));
#25936=CARTESIAN_POINT('Ctrl Pts',(-16.4123522628062,13.9197595264192,0.0286666666665155));
#25937=CARTESIAN_POINT('Ctrl Pts',(-15.5,13.9197595264192,-0.0130000000001518));
#25938=CARTESIAN_POINT('Ctrl Pts',(-14.5876477371938,13.9197595264192,-0.0546666666668173));
#25939=CARTESIAN_POINT('Ctrl Pts',(-14.1314716057906,14.7098797632096,-0.0963333333334846));
#25940=CARTESIAN_POINT('Ctrl Pts',(-13.6752954743875,15.5,-0.138000000000152));
#25941=CARTESIAN_POINT('Ctrl Pts',(-14.1314716057906,16.2901202367904,-0.179666666666819));
#25942=CARTESIAN_POINT('Ctrl Pts',(-14.5876477371938,17.0802404735808,-0.221333333333486));
#25943=CARTESIAN_POINT('Ctrl Pts',(-15.5,17.0802404735808,-0.263000000000154));
#25944=CARTESIAN_POINT('Ctrl Pts',(-16.4123522628062,17.0802404735808,-0.304666666666821));
#25945=CARTESIAN_POINT('Ctrl Pts',(-16.8685283942094,16.2901202367904,-0.346333333333488));
#25946=CARTESIAN_POINT('Ctrl Pts',(-17.3247045256125,15.5,-0.388000000000156));
#25947=CARTESIAN_POINT('Ctrl Pts',(-16.8685283942094,14.7098797632096,-0.429666666666823));
#25948=CARTESIAN_POINT('Ctrl Pts',(-16.4123522628062,13.9197595264192,-0.47133333333349));
#25949=CARTESIAN_POINT('Ctrl Pts',(-15.5,13.9197595264192,-0.513000000000157));
#25950=CARTESIAN_POINT('Ctrl Pts',(-14.5876477371938,13.9197595264192,-0.554666666666825));
#25951=CARTESIAN_POINT('Ctrl Pts',(-14.1314716057906,14.7098797632096,-0.596333333333492));
#25952=CARTESIAN_POINT('Ctrl Pts',(-13.6752954743875,15.5,-0.638000000000159));
#25953=CARTESIAN_POINT('Ctrl Pts',(-14.1314716057906,16.2901202367904,-0.679666666666827));
#25954=CARTESIAN_POINT('Ctrl Pts',(-14.5876477371938,17.0802404735808,-0.721333333333494));
#25955=CARTESIAN_POINT('Ctrl Pts',(-15.5,17.0802404735808,-0.763000000000161));
#25956=CARTESIAN_POINT('Ctrl Pts',(-16.4123522628062,17.0802404735808,-0.804666666666829));
#25957=CARTESIAN_POINT('Ctrl Pts',(-16.8685283942094,16.2901202367904,-0.846333333333496));
#25958=CARTESIAN_POINT('Ctrl Pts',(-17.3247045256125,15.5,-0.888000000000163));
#25959=CARTESIAN_POINT('Ctrl Pts',(-16.8685283942094,14.7098797632096,-0.92966666666683));
#25960=CARTESIAN_POINT('Ctrl Pts',(-16.4123522628062,13.9197595264192,-0.971333333333498));
#25961=CARTESIAN_POINT('Ctrl Pts',(-15.5,13.9197595264192,-1.01300000000016));
#25962=CARTESIAN_POINT('Ctrl Pts',(-14.5876477371938,13.9197595264192,-1.05466666666683));
#25963=CARTESIAN_POINT('Ctrl Pts',(-14.1314716057906,14.7098797632096,-1.0963333333335));
#25964=CARTESIAN_POINT('Ctrl Pts',(-13.6752954743875,15.5,-1.13800000000017));
#25965=CARTESIAN_POINT('Ctrl Pts',(-14.1314716057906,16.2901202367904,-1.17966666666683));
#25966=CARTESIAN_POINT('Ctrl Pts',(-14.5876477371938,17.0802404735808,-1.2213333333335));
#25967=CARTESIAN_POINT('Ctrl Pts',(-15.5,17.0802404735808,-1.26300000000017));
#25968=CARTESIAN_POINT('Ctrl Pts',(-16.4123522628062,17.0802404735808,-1.30466666666683));
#25969=CARTESIAN_POINT('Ctrl Pts',(-16.8685283942094,16.2901202367904,-1.3463333333335));
#25970=CARTESIAN_POINT('Ctrl Pts',(-17.3247045256125,15.5,-1.38800000000017));
#25971=CARTESIAN_POINT('Ctrl Pts',(-16.8685283942094,14.7098797632096,-1.42966666666684));
#25972=CARTESIAN_POINT('Ctrl Pts',(-16.4123522628062,13.9197595264192,-1.4713333333335));
#25973=CARTESIAN_POINT('Ctrl Pts',(-15.5,13.9197595264192,-1.51300000000017));
#25974=CARTESIAN_POINT('Ctrl Pts',(-14.5876477371938,13.9197595264192,-1.55466666666684));
#25975=CARTESIAN_POINT('Ctrl Pts',(-14.1314716057906,14.7098797632096,-1.59633333333351));
#25976=CARTESIAN_POINT('Ctrl Pts',(-13.6752954743875,15.5,-1.63800000000017));
#25977=CARTESIAN_POINT('Ctrl Pts',(-14.1314716057906,16.2901202367904,-1.67966666666684));
#25978=CARTESIAN_POINT('Ctrl Pts',(-14.5876477371938,17.0802404735808,-1.72133333333351));
#25979=CARTESIAN_POINT('Ctrl Pts',(-15.5,17.0802404735808,-1.76300000000017));
#25980=CARTESIAN_POINT('Ctrl Pts',(-16.4123522628062,17.0802404735808,-1.80466666666684));
#25981=CARTESIAN_POINT('Ctrl Pts',(-16.8685283942094,16.2901202367904,-1.84633333333351));
#25982=CARTESIAN_POINT('Ctrl Pts',(-17.3247045256125,15.5,-1.88800000000018));
#25983=CARTESIAN_POINT('Ctrl Pts',(-16.8685283942094,14.7098797632096,-1.92966666666684));
#25984=CARTESIAN_POINT('Ctrl Pts',(-16.700583153372,14.4189900731899,-1.94500661517905));
#25985=CARTESIAN_POINT('Ctrl Pts',(-16.4288340223699,14.2215527726061,-1.96262314816781));
#25986=CARTESIAN_POINT('Origin',(-16.5839252605846,14.0080754615186,-2.17746715486548));
#25987=CARTESIAN_POINT('',(-16.4288300625788,14.2215498957104,-2.02512301642216));
#25988=CARTESIAN_POINT('Ctrl Pts',(-15.5,17.0802404735808,11.2370201234482));
#25989=CARTESIAN_POINT('Ctrl Pts',(-16.4123522628062,17.0802404735808,11.1953534567815));
#25990=CARTESIAN_POINT('Ctrl Pts',(-16.8685283942094,16.2901202367904,11.1536867901149));
#25991=CARTESIAN_POINT('Ctrl Pts',(-17.3247045256125,15.5,11.1120201234482));
#25992=CARTESIAN_POINT('Ctrl Pts',(-16.8685283942094,14.7098797632096,11.0703534567815));
#25993=CARTESIAN_POINT('Ctrl Pts',(-16.4123522628062,13.9197595264192,11.0286867901149));
#25994=CARTESIAN_POINT('Ctrl Pts',(-15.5,13.9197595264192,10.9870201234482));
#25995=CARTESIAN_POINT('Ctrl Pts',(-14.5876477371938,13.9197595264192,10.9453534567815));
#25996=CARTESIAN_POINT('Ctrl Pts',(-14.1314716057906,14.7098797632096,10.9036867901149));
#25997=CARTESIAN_POINT('Ctrl Pts',(-13.6752954743875,15.5,10.8620201234482));
#25998=CARTESIAN_POINT('Ctrl Pts',(-14.1314716057906,16.2901202367904,10.8203534567815));
#25999=CARTESIAN_POINT('Ctrl Pts',(-14.5876477371938,17.0802404735808,10.7786867901149));
#26000=CARTESIAN_POINT('Ctrl Pts',(-15.5,17.0802404735808,10.7370201234482));
#26001=CARTESIAN_POINT('Ctrl Pts',(-16.4123522628062,17.0802404735808,10.6953534567815));
#26002=CARTESIAN_POINT('Ctrl Pts',(-16.8685283942094,16.2901202367904,10.6536867901149));
#26003=CARTESIAN_POINT('Ctrl Pts',(-17.3247045256125,15.5,10.6120201234482));
#26004=CARTESIAN_POINT('Ctrl Pts',(-16.8685283942094,14.7098797632096,10.5703534567815));
#26005=CARTESIAN_POINT('Ctrl Pts',(-16.4123522628062,13.9197595264192,10.5286867901149));
#26006=CARTESIAN_POINT('Ctrl Pts',(-15.5,13.9197595264192,10.4870201234482));
#26007=CARTESIAN_POINT('Ctrl Pts',(-14.5876477371938,13.9197595264192,10.4453534567815));
#26008=CARTESIAN_POINT('Ctrl Pts',(-14.1314716057906,14.7098797632096,10.4036867901149));
#26009=CARTESIAN_POINT('Ctrl Pts',(-13.6752954743875,15.5,10.3620201234482));
#26010=CARTESIAN_POINT('Ctrl Pts',(-14.1314716057906,16.2901202367904,10.3203534567815));
#26011=CARTESIAN_POINT('Ctrl Pts',(-14.5876477371938,17.0802404735808,10.2786867901149));
#26012=CARTESIAN_POINT('Ctrl Pts',(-15.5,17.0802404735808,10.2370201234482));
#26013=CARTESIAN_POINT('Ctrl Pts',(-16.4123522628062,17.0802404735808,10.1953534567815));
#26014=CARTESIAN_POINT('Ctrl Pts',(-16.8685283942094,16.2901202367904,10.1536867901149));
#26015=CARTESIAN_POINT('Ctrl Pts',(-17.3247045256125,15.5,10.1120201234482));
#26016=CARTESIAN_POINT('Ctrl Pts',(-16.8685283942094,14.7098797632096,10.0703534567815));
#26017=CARTESIAN_POINT('Ctrl Pts',(-16.4123522628062,13.9197595264192,10.0286867901149));
#26018=CARTESIAN_POINT('Ctrl Pts',(-15.5,13.9197595264192,9.98702012344818));
#26019=CARTESIAN_POINT('Ctrl Pts',(-14.5876477371938,13.9197595264192,9.94535345678152));
#26020=CARTESIAN_POINT('Ctrl Pts',(-14.1314716057906,14.7098797632096,9.90368679011485));
#26021=CARTESIAN_POINT('Ctrl Pts',(-13.6752954743875,15.5,9.86202012344818));
#26022=CARTESIAN_POINT('Ctrl Pts',(-14.1314716057906,16.2901202367904,9.82035345678152));
#26023=CARTESIAN_POINT('Ctrl Pts',(-14.5876477371938,17.0802404735808,9.77868679011485));
#26024=CARTESIAN_POINT('Ctrl Pts',(-15.5,17.0802404735808,9.73702012344818));
#26025=CARTESIAN_POINT('Ctrl Pts',(-16.4123522628062,17.0802404735808,9.69535345678152));
#26026=CARTESIAN_POINT('Ctrl Pts',(-16.8685283942094,16.2901202367904,9.65368679011485));
#26027=CARTESIAN_POINT('Ctrl Pts',(-17.3247045256125,15.5,9.61202012344818));
#26028=CARTESIAN_POINT('Ctrl Pts',(-16.8685283942094,14.7098797632096,9.57035345678151));
#26029=CARTESIAN_POINT('Ctrl Pts',(-16.4123522628062,13.9197595264192,9.52868679011484));
#26030=CARTESIAN_POINT('Ctrl Pts',(-15.5,13.9197595264192,9.48702012344818));
#26031=CARTESIAN_POINT('Ctrl Pts',(-14.5876477371938,13.9197595264192,9.44535345678151));
#26032=CARTESIAN_POINT('Ctrl Pts',(-14.1314716057906,14.7098797632096,9.40368679011484));
#26033=CARTESIAN_POINT('Ctrl Pts',(-13.6752954743875,15.5,9.36202012344818));
#26034=CARTESIAN_POINT('Ctrl Pts',(-14.1314716057906,16.2901202367904,9.32035345678151));
#26035=CARTESIAN_POINT('Ctrl Pts',(-14.5876477371938,17.0802404735808,9.27868679011484));
#26036=CARTESIAN_POINT('Ctrl Pts',(-15.5,17.0802404735808,9.23702012344818));
#26037=CARTESIAN_POINT('Ctrl Pts',(-16.4123522628062,17.0802404735808,9.19535345678151));
#26038=CARTESIAN_POINT('Ctrl Pts',(-16.8685283942094,16.2901202367904,9.15368679011484));
#26039=CARTESIAN_POINT('Ctrl Pts',(-17.3247045256125,15.5,9.11202012344818));
#26040=CARTESIAN_POINT('Ctrl Pts',(-16.8685283942094,14.7098797632096,9.07035345678151));
#26041=CARTESIAN_POINT('Ctrl Pts',(-16.4123522628062,13.9197595264192,9.02868679011484));
#26042=CARTESIAN_POINT('Ctrl Pts',(-15.5,13.9197595264192,8.98702012344817));
#26043=CARTESIAN_POINT('Ctrl Pts',(-14.5876477371938,13.9197595264192,8.9453534567815));
#26044=CARTESIAN_POINT('Ctrl Pts',(-14.1314716057906,14.7098797632096,8.90368679011484));
#26045=CARTESIAN_POINT('Ctrl Pts',(-13.6752954743875,15.5,8.86202012344817));
#26046=CARTESIAN_POINT('Ctrl Pts',(-14.1314716057906,16.2901202367904,8.8203534567815));
#26047=CARTESIAN_POINT('Ctrl Pts',(-14.5876477371938,17.0802404735808,8.77868679011483));
#26048=CARTESIAN_POINT('Ctrl Pts',(-15.5,17.0802404735808,8.73702012344817));
#26049=CARTESIAN_POINT('Ctrl Pts',(-16.4123522628062,17.0802404735808,8.6953534567815));
#26050=CARTESIAN_POINT('Ctrl Pts',(-16.8685283942094,16.2901202367904,8.65368679011483));
#26051=CARTESIAN_POINT('Ctrl Pts',(-17.3247045256125,15.5,8.61202012344817));
#26052=CARTESIAN_POINT('Ctrl Pts',(-16.8685283942094,14.7098797632096,8.5703534567815));
#26053=CARTESIAN_POINT('Ctrl Pts',(-16.4123522628062,13.9197595264192,8.52868679011483));
#26054=CARTESIAN_POINT('Ctrl Pts',(-15.5,13.9197595264192,8.48702012344816));
#26055=CARTESIAN_POINT('Ctrl Pts',(-14.5876477371938,13.9197595264192,8.4453534567815));
#26056=CARTESIAN_POINT('Ctrl Pts',(-14.1314716057906,14.7098797632096,8.40368679011483));
#26057=CARTESIAN_POINT('Ctrl Pts',(-13.6752954743875,15.5,8.36202012344816));
#26058=CARTESIAN_POINT('Ctrl Pts',(-14.1314716057906,16.2901202367904,8.3203534567815));
#26059=CARTESIAN_POINT('Ctrl Pts',(-14.5876477371938,17.0802404735808,8.27868679011483));
#26060=CARTESIAN_POINT('Ctrl Pts',(-15.5,17.0802404735808,8.23702012344816));
#26061=CARTESIAN_POINT('Ctrl Pts',(-16.4123522628062,17.0802404735808,8.19535345678149));
#26062=CARTESIAN_POINT('Ctrl Pts',(-16.8685283942094,16.2901202367904,8.15368679011483));
#26063=CARTESIAN_POINT('Ctrl Pts',(-17.3247045256125,15.5,8.11202012344816));
#26064=CARTESIAN_POINT('Ctrl Pts',(-16.8685283942094,14.7098797632096,8.0703534567815));
#26065=CARTESIAN_POINT('Ctrl Pts',(-16.4123522628062,13.9197595264192,8.02868679011483));
#26066=CARTESIAN_POINT('Ctrl Pts',(-15.5,13.9197595264192,7.98702012344816));
#26067=CARTESIAN_POINT('Ctrl Pts',(-14.5876477371938,13.9197595264192,7.94535345678149));
#26068=CARTESIAN_POINT('Ctrl Pts',(-14.1314716057906,14.7098797632096,7.90368679011482));
#26069=CARTESIAN_POINT('Ctrl Pts',(-13.6752954743875,15.5,7.86202012344816));
#26070=CARTESIAN_POINT('Ctrl Pts',(-14.1314716057906,16.2901202367904,7.82035345678149));
#26071=CARTESIAN_POINT('Ctrl Pts',(-14.5876477371938,17.0802404735808,7.77868679011482));
#26072=CARTESIAN_POINT('Ctrl Pts',(-15.5,17.0802404735808,7.73702012344816));
#26073=CARTESIAN_POINT('Ctrl Pts',(-16.4123522628062,17.0802404735808,7.69535345678149));
#26074=CARTESIAN_POINT('Ctrl Pts',(-16.8685283942094,16.2901202367904,7.65368679011482));
#26075=CARTESIAN_POINT('Ctrl Pts',(-17.3247045256125,15.5,7.61202012344815));
#26076=CARTESIAN_POINT('Ctrl Pts',(-16.8685283942094,14.7098797632096,7.57035345678149));
#26077=CARTESIAN_POINT('Ctrl Pts',(-16.4123522628062,13.9197595264192,7.52868679011482));
#26078=CARTESIAN_POINT('Ctrl Pts',(-15.5,13.9197595264192,7.48702012344815));
#26079=CARTESIAN_POINT('Ctrl Pts',(-14.5876477371938,13.9197595264192,7.44535345678149));
#26080=CARTESIAN_POINT('Ctrl Pts',(-14.1314716057906,14.7098797632096,7.40368679011482));
#26081=CARTESIAN_POINT('Ctrl Pts',(-13.6752954743875,15.5,7.36202012344815));
#26082=CARTESIAN_POINT('Ctrl Pts',(-14.1314716057906,16.2901202367904,7.32035345678148));
#26083=CARTESIAN_POINT('Ctrl Pts',(-14.5876477371938,17.0802404735808,7.27868679011482));
#26084=CARTESIAN_POINT('Ctrl Pts',(-15.5,17.0802404735808,7.23702012344815));
#26085=CARTESIAN_POINT('Ctrl Pts',(-16.4123522628062,17.0802404735808,7.19535345678148));
#26086=CARTESIAN_POINT('Ctrl Pts',(-16.8685283942094,16.2901202367904,7.15368679011481));
#26087=CARTESIAN_POINT('Ctrl Pts',(-17.3247045256125,15.5,7.11202012344815));
#26088=CARTESIAN_POINT('Ctrl Pts',(-16.8685283942094,14.7098797632096,7.07035345678148));
#26089=CARTESIAN_POINT('Ctrl Pts',(-16.4123522628062,13.9197595264192,7.02868679011481));
#26090=CARTESIAN_POINT('Ctrl Pts',(-15.5,13.9197595264192,6.98702012344814));
#26091=CARTESIAN_POINT('Ctrl Pts',(-14.5876477371938,13.9197595264192,6.94535345678148));
#26092=CARTESIAN_POINT('Ctrl Pts',(-14.1314716057906,14.7098797632096,6.90368679011481));
#26093=CARTESIAN_POINT('Ctrl Pts',(-13.6752954743875,15.5,6.86202012344814));
#26094=CARTESIAN_POINT('Ctrl Pts',(-14.1314716057906,16.2901202367904,6.82035345678148));
#26095=CARTESIAN_POINT('Ctrl Pts',(-14.5876477371938,17.0802404735808,6.77868679011481));
#26096=CARTESIAN_POINT('Ctrl Pts',(-15.5,17.0802404735808,6.73702012344814));
#26097=CARTESIAN_POINT('Ctrl Pts',(-16.4123522628062,17.0802404735808,6.69535345678147));
#26098=CARTESIAN_POINT('Ctrl Pts',(-16.8685283942094,16.2901202367904,6.65368679011481));
#26099=CARTESIAN_POINT('Ctrl Pts',(-17.3247045256125,15.5,6.61202012344814));
#26100=CARTESIAN_POINT('Ctrl Pts',(-16.8685283942094,14.7098797632096,6.57035345678147));
#26101=CARTESIAN_POINT('Ctrl Pts',(-16.4123522628062,13.9197595264192,6.52868679011481));
#26102=CARTESIAN_POINT('Ctrl Pts',(-15.5,13.9197595264192,6.48702012344814));
#26103=CARTESIAN_POINT('Ctrl Pts',(-14.5876477371938,13.9197595264192,6.44535345678147));
#26104=CARTESIAN_POINT('Ctrl Pts',(-14.1314716057906,14.7098797632096,6.40368679011481));
#26105=CARTESIAN_POINT('Ctrl Pts',(-13.6752954743875,15.5,6.36202012344814));
#26106=CARTESIAN_POINT('Ctrl Pts',(-14.1314716057906,16.2901202367904,6.32035345678147));
#26107=CARTESIAN_POINT('Ctrl Pts',(-14.5876477371938,17.0802404735808,6.2786867901148));
#26108=CARTESIAN_POINT('Ctrl Pts',(-15.5,17.0802404735808,6.23702012344813));
#26109=CARTESIAN_POINT('Ctrl Pts',(-16.4123522628062,17.0802404735808,6.19535345678147));
#26110=CARTESIAN_POINT('Ctrl Pts',(-16.8685283942094,16.2901202367904,6.1536867901148));
#26111=CARTESIAN_POINT('Ctrl Pts',(-17.3247045256125,15.5,6.11202012344813));
#26112=CARTESIAN_POINT('Ctrl Pts',(-16.8685283942094,14.7098797632096,6.07035345678146));
#26113=CARTESIAN_POINT('Ctrl Pts',(-16.4123522628062,13.9197595264192,6.0286867901148));
#26114=CARTESIAN_POINT('Ctrl Pts',(-15.5,13.9197595264192,5.98702012344813));
#26115=CARTESIAN_POINT('Ctrl Pts',(-14.5876477371938,13.9197595264192,5.94535345678146));
#26116=CARTESIAN_POINT('Ctrl Pts',(-14.1314716057906,14.7098797632096,5.9036867901148));
#26117=CARTESIAN_POINT('Ctrl Pts',(-13.6752954743875,15.5,5.86202012344813));
#26118=CARTESIAN_POINT('Ctrl Pts',(-14.1314716057906,16.2901202367904,5.82035345678146));
#26119=CARTESIAN_POINT('Ctrl Pts',(-14.5876477371938,17.0802404735808,5.77868679011479));
#26120=CARTESIAN_POINT('Ctrl Pts',(-15.5,17.0802404735808,5.73702012344813));
#26121=CARTESIAN_POINT('Ctrl Pts',(-16.4123522628062,17.0802404735808,5.69535345678146));
#26122=CARTESIAN_POINT('Ctrl Pts',(-16.8685283942094,16.2901202367904,5.65368679011479));
#26123=CARTESIAN_POINT('Ctrl Pts',(-17.3247045256125,15.5,5.61202012344813));
#26124=CARTESIAN_POINT('Ctrl Pts',(-16.8685283942094,14.7098797632096,5.57035345678146));
#26125=CARTESIAN_POINT('Ctrl Pts',(-16.4123522628062,13.9197595264192,5.52868679011479));
#26126=CARTESIAN_POINT('Ctrl Pts',(-15.5,13.9197595264192,5.48702012344813));
#26127=CARTESIAN_POINT('Ctrl Pts',(-14.5876477371938,13.9197595264192,5.44535345678146));
#26128=CARTESIAN_POINT('Ctrl Pts',(-14.1314716057906,14.7098797632096,5.40368679011479));
#26129=CARTESIAN_POINT('Ctrl Pts',(-13.6752954743875,15.5,5.36202012344812));
#26130=CARTESIAN_POINT('Ctrl Pts',(-14.1314716057906,16.2901202367904,5.32035345678146));
#26131=CARTESIAN_POINT('Ctrl Pts',(-14.5876477371938,17.0802404735808,5.27868679011479));
#26132=CARTESIAN_POINT('Ctrl Pts',(-15.5,17.0802404735808,5.23702012344812));
#26133=CARTESIAN_POINT('Ctrl Pts',(-16.4123522628062,17.0802404735808,5.19535345678145));
#26134=CARTESIAN_POINT('Ctrl Pts',(-16.8685283942094,16.2901202367904,5.15368679011479));
#26135=CARTESIAN_POINT('Ctrl Pts',(-17.3247045256125,15.5,5.11202012344812));
#26136=CARTESIAN_POINT('Ctrl Pts',(-16.8685283942094,14.7098797632096,5.07035345678145));
#26137=CARTESIAN_POINT('Ctrl Pts',(-16.4123522628062,13.9197595264192,5.02868679011478));
#26138=CARTESIAN_POINT('Ctrl Pts',(-15.5,13.9197595264192,4.98702012344812));
#26139=CARTESIAN_POINT('Ctrl Pts',(-14.5876477371938,13.9197595264192,4.94535345678145));
#26140=CARTESIAN_POINT('Ctrl Pts',(-14.1314716057906,14.7098797632096,4.90368679011478));
#26141=CARTESIAN_POINT('Ctrl Pts',(-13.6752954743875,15.5,4.86202012344812));
#26142=CARTESIAN_POINT('Ctrl Pts',(-14.1314716057906,16.2901202367904,4.82035345678145));
#26143=CARTESIAN_POINT('Ctrl Pts',(-14.5876477371938,17.0802404735808,4.77868679011478));
#26144=CARTESIAN_POINT('Ctrl Pts',(-15.5,17.0802404735808,4.73702012344812));
#26145=CARTESIAN_POINT('Ctrl Pts',(-16.4123522628062,17.0802404735808,4.69535345678145));
#26146=CARTESIAN_POINT('Ctrl Pts',(-16.8685283942094,16.2901202367904,4.65368679011478));
#26147=CARTESIAN_POINT('Ctrl Pts',(-17.3247045256125,15.5,4.61202012344811));
#26148=CARTESIAN_POINT('Ctrl Pts',(-16.8685283942094,14.7098797632096,4.57035345678145));
#26149=CARTESIAN_POINT('Ctrl Pts',(-16.4123522628062,13.9197595264192,4.52868679011478));
#26150=CARTESIAN_POINT('Ctrl Pts',(-15.5,13.9197595264192,4.48702012344811));
#26151=CARTESIAN_POINT('Ctrl Pts',(-14.5876477371938,13.9197595264192,4.44535345678144));
#26152=CARTESIAN_POINT('Ctrl Pts',(-14.1314716057906,14.7098797632096,4.40368679011478));
#26153=CARTESIAN_POINT('Ctrl Pts',(-13.6752954743875,15.5,4.36202012344811));
#26154=CARTESIAN_POINT('Ctrl Pts',(-14.1314716057906,16.2901202367904,4.32035345678144));
#26155=CARTESIAN_POINT('Ctrl Pts',(-14.5876477371938,17.0802404735808,4.27868679011477));
#26156=CARTESIAN_POINT('Ctrl Pts',(-15.5,17.0802404735808,4.23702012344811));
#26157=CARTESIAN_POINT('Ctrl Pts',(-16.4123522628062,17.0802404735808,4.19535345678144));
#26158=CARTESIAN_POINT('Ctrl Pts',(-16.8685283942094,16.2901202367904,4.15368679011477));
#26159=CARTESIAN_POINT('Ctrl Pts',(-17.3247045256125,15.5,4.11202012344811));
#26160=CARTESIAN_POINT('Ctrl Pts',(-16.8685283942094,14.7098797632096,4.07035345678144));
#26161=CARTESIAN_POINT('Ctrl Pts',(-16.4123522628062,13.9197595264192,4.02868679011477));
#26162=CARTESIAN_POINT('Ctrl Pts',(-15.5,13.9197595264192,3.9870201234481));
#26163=CARTESIAN_POINT('Ctrl Pts',(-14.5876477371938,13.9197595264192,3.94535345678144));
#26164=CARTESIAN_POINT('Ctrl Pts',(-14.1314716057906,14.7098797632096,3.90368679011477));
#26165=CARTESIAN_POINT('Ctrl Pts',(-13.6752954743875,15.5,3.8620201234481));
#26166=CARTESIAN_POINT('Ctrl Pts',(-14.1314716057906,16.2901202367904,3.82035345678144));
#26167=CARTESIAN_POINT('Ctrl Pts',(-14.5876477371938,17.0802404735808,3.77868679011477));
#26168=CARTESIAN_POINT('Ctrl Pts',(-15.5,17.0802404735808,3.7370201234481));
#26169=CARTESIAN_POINT('Ctrl Pts',(-16.4123522628062,17.0802404735808,3.69535345678143));
#26170=CARTESIAN_POINT('Ctrl Pts',(-16.8685283942094,16.2901202367904,3.65368679011477));
#26171=CARTESIAN_POINT('Ctrl Pts',(-17.3247045256125,15.5,3.6120201234481));
#26172=CARTESIAN_POINT('Ctrl Pts',(-16.8685283942094,14.7098797632096,3.57035345678143));
#26173=CARTESIAN_POINT('Ctrl Pts',(-16.4123522628062,13.9197595264192,3.52868679011477));
#26174=CARTESIAN_POINT('Ctrl Pts',(-15.5,13.9197595264192,3.4870201234481));
#26175=CARTESIAN_POINT('Ctrl Pts',(-14.5876477371938,13.9197595264192,3.44535345678143));
#26176=CARTESIAN_POINT('Ctrl Pts',(-14.1314716057906,14.7098797632096,3.40368679011476));
#26177=CARTESIAN_POINT('Ctrl Pts',(-13.6752954743875,15.5,3.3620201234481));
#26178=CARTESIAN_POINT('Ctrl Pts',(-14.1314716057906,16.2901202367904,3.32035345678143));
#26179=CARTESIAN_POINT('Ctrl Pts',(-14.5876477371938,17.0802404735808,3.27868679011476));
#26180=CARTESIAN_POINT('Ctrl Pts',(-15.5,17.0802404735808,3.2370201234481));
#26181=CARTESIAN_POINT('Ctrl Pts',(-16.4123522628062,17.0802404735808,3.19535345678143));
#26182=CARTESIAN_POINT('Ctrl Pts',(-16.8685283942094,16.2901202367904,3.15368679011476));
#26183=CARTESIAN_POINT('Ctrl Pts',(-17.3247045256125,15.5,3.11202012344809));
#26184=CARTESIAN_POINT('Ctrl Pts',(-16.8685283942094,14.7098797632096,3.07035345678143));
#26185=CARTESIAN_POINT('Ctrl Pts',(-16.4123522628062,13.9197595264192,3.02868679011476));
#26186=CARTESIAN_POINT('Ctrl Pts',(-15.5,13.9197595264192,2.98702012344809));
#26187=CARTESIAN_POINT('Ctrl Pts',(-14.5876477371938,13.9197595264192,2.94535345678142));
#26188=CARTESIAN_POINT('Ctrl Pts',(-14.1314716057906,14.7098797632096,2.90368679011476));
#26189=CARTESIAN_POINT('Ctrl Pts',(-13.6752954743875,15.5,2.86202012344809));
#26190=CARTESIAN_POINT('Ctrl Pts',(-14.1314716057906,16.2901202367904,2.82035345678142));
#26191=CARTESIAN_POINT('Ctrl Pts',(-14.5876477371938,17.0802404735808,2.77868679011475));
#26192=CARTESIAN_POINT('Ctrl Pts',(-15.5,17.0802404735808,2.73702012344809));
#26193=CARTESIAN_POINT('Ctrl Pts',(-16.4123522628062,17.0802404735808,2.69535345678142));
#26194=CARTESIAN_POINT('Ctrl Pts',(-16.8685283942094,16.2901202367904,2.65368679011475));
#26195=CARTESIAN_POINT('Ctrl Pts',(-17.3247045256125,15.5,2.61202012344809));
#26196=CARTESIAN_POINT('Ctrl Pts',(-16.8685283942094,14.7098797632096,2.57035345678142));
#26197=CARTESIAN_POINT('Ctrl Pts',(-16.4123522628062,13.9197595264192,2.52868679011475));
#26198=CARTESIAN_POINT('Ctrl Pts',(-15.5,13.9197595264192,2.48702012344808));
#26199=CARTESIAN_POINT('Ctrl Pts',(-14.5876477371938,13.9197595264192,2.44535345678142));
#26200=CARTESIAN_POINT('Ctrl Pts',(-14.1314716057906,14.7098797632096,2.40368679011475));
#26201=CARTESIAN_POINT('Ctrl Pts',(-13.6752954743875,15.5,2.36202012344808));
#26202=CARTESIAN_POINT('Ctrl Pts',(-14.1314716057906,16.2901202367904,2.32035345678142));
#26203=CARTESIAN_POINT('Ctrl Pts',(-14.5876477371938,17.0802404735808,2.27868679011475));
#26204=CARTESIAN_POINT('Ctrl Pts',(-15.5,17.0802404735808,2.23702012344808));
#26205=CARTESIAN_POINT('Ctrl Pts',(-16.4123522628062,17.0802404735808,2.19535345678141));
#26206=CARTESIAN_POINT('Ctrl Pts',(-16.8685283942094,16.2901202367904,2.15368679011475));
#26207=CARTESIAN_POINT('Ctrl Pts',(-17.3247045256125,15.5,2.11202012344808));
#26208=CARTESIAN_POINT('Ctrl Pts',(-16.8685283942094,14.7098797632096,2.07035345678141));
#26209=CARTESIAN_POINT('Ctrl Pts',(-16.4123522628062,13.9197595264192,2.02868679011475));
#26210=CARTESIAN_POINT('Ctrl Pts',(-15.5,13.9197595264192,1.98702012344808));
#26211=CARTESIAN_POINT('Ctrl Pts',(-14.5876477371938,13.9197595264192,1.94535345678141));
#26212=CARTESIAN_POINT('Ctrl Pts',(-14.1314716057906,14.7098797632096,1.90368679011474));
#26213=CARTESIAN_POINT('Ctrl Pts',(-13.6752954743875,15.5,1.86202012344808));
#26214=CARTESIAN_POINT('Ctrl Pts',(-14.1314716057906,16.2901202367904,1.82035345678141));
#26215=CARTESIAN_POINT('Ctrl Pts',(-14.5876477371938,17.0802404735808,1.77868679011474));
#26216=CARTESIAN_POINT('Ctrl Pts',(-15.5,17.0802404735808,1.73702012344807));
#26217=CARTESIAN_POINT('Ctrl Pts',(-16.4123522628062,17.0802404735808,1.69535345678141));
#26218=CARTESIAN_POINT('Ctrl Pts',(-16.8685283942094,16.2901202367904,1.65368679011474));
#26219=CARTESIAN_POINT('Ctrl Pts',(-17.3247045256125,15.5,1.61202012344807));
#26220=CARTESIAN_POINT('Ctrl Pts',(-16.8685283942094,14.7098797632096,1.57035345678141));
#26221=CARTESIAN_POINT('Ctrl Pts',(-16.4123522628062,13.9197595264192,1.52868679011474));
#26222=CARTESIAN_POINT('Ctrl Pts',(-15.5,13.9197595264192,1.48702012344807));
#26223=CARTESIAN_POINT('Ctrl Pts',(-14.5876477371938,13.9197595264192,1.4453534567814));
#26224=CARTESIAN_POINT('Ctrl Pts',(-14.1314716057906,14.7098797632096,1.40368679011474));
#26225=CARTESIAN_POINT('Ctrl Pts',(-13.6752954743875,15.5,1.36202012344807));
#26226=CARTESIAN_POINT('Ctrl Pts',(-14.1314716057906,16.2901202367904,1.3203534567814));
#26227=CARTESIAN_POINT('Ctrl Pts',(-14.5876477371938,17.0802404735808,1.27868679011473));
#26228=CARTESIAN_POINT('Ctrl Pts',(-15.5,17.0802404735808,1.23702012344807));
#26229=CARTESIAN_POINT('Ctrl Pts',(-16.4123522628062,17.0802404735808,1.1953534567814));
#26230=CARTESIAN_POINT('Ctrl Pts',(-16.8685283942094,16.2901202367904,1.15368679011473));
#26231=CARTESIAN_POINT('Ctrl Pts',(-17.3247045256125,15.5,1.11202012344807));
#26232=CARTESIAN_POINT('Ctrl Pts',(-16.8685283942094,14.7098797632096,1.0703534567814));
#26233=CARTESIAN_POINT('Ctrl Pts',(-16.4123522628062,13.9197595264192,1.02868679011473));
#26234=CARTESIAN_POINT('Ctrl Pts',(-15.5,13.9197595264192,0.987020123448065));
#26235=CARTESIAN_POINT('Ctrl Pts',(-14.5876477371938,13.9197595264192,0.945353456781398));
#26236=CARTESIAN_POINT('Ctrl Pts',(-14.1314716057906,14.7098797632096,0.903686790114731));
#26237=CARTESIAN_POINT('Ctrl Pts',(-13.6752954743875,15.5,0.862020123448063));
#26238=CARTESIAN_POINT('Ctrl Pts',(-14.1314716057906,16.2901202367904,0.820353456781396));
#26239=CARTESIAN_POINT('Ctrl Pts',(-14.5876477371938,17.0802404735808,0.778686790114729));
#26240=CARTESIAN_POINT('Ctrl Pts',(-15.5,17.0802404735808,0.737020123448061));
#26241=CARTESIAN_POINT('Ctrl Pts',(-16.4123522628062,17.0802404735808,0.695353456781394));
#26242=CARTESIAN_POINT('Ctrl Pts',(-16.8685283942094,16.2901202367904,0.653686790114727));
#26243=CARTESIAN_POINT('Ctrl Pts',(-17.3247045256125,15.5,0.61202012344806));
#26244=CARTESIAN_POINT('Ctrl Pts',(-16.8685283942094,14.7098797632096,0.570353456781392));
#26245=CARTESIAN_POINT('Ctrl Pts',(-16.4123522628062,13.9197595264192,0.528686790114725));
#26246=CARTESIAN_POINT('Ctrl Pts',(-15.5,13.9197595264192,0.487020123448058));
#26247=CARTESIAN_POINT('Ctrl Pts',(-14.5876477371938,13.9197595264192,0.44535345678139));
#26248=CARTESIAN_POINT('Ctrl Pts',(-14.1314716057906,14.7098797632096,0.403686790114723));
#26249=CARTESIAN_POINT('Ctrl Pts',(-13.6752954743875,15.5,0.362020123448056));
#26250=CARTESIAN_POINT('Ctrl Pts',(-14.1314716057906,16.2901202367904,0.320353456781388));
#26251=CARTESIAN_POINT('Ctrl Pts',(-14.5876477371938,17.0802404735808,0.278686790114721));
#26252=CARTESIAN_POINT('Ctrl Pts',(-15.5,17.0802404735808,0.237020123448054));
#26253=CARTESIAN_POINT('Ctrl Pts',(-16.4123522628062,17.0802404735808,0.195353456781387));
#26254=CARTESIAN_POINT('Ctrl Pts',(-16.8685283942094,16.2901202367904,0.153686790114719));
#26255=CARTESIAN_POINT('Ctrl Pts',(-17.3247045256125,15.5,0.112020123448052));
#26256=CARTESIAN_POINT('Ctrl Pts',(-16.8685283942094,14.7098797632096,0.0703534567813848));
#26257=CARTESIAN_POINT('Ctrl Pts',(-16.4123522628062,13.9197595264192,0.0286867901147175));
#26258=CARTESIAN_POINT('Ctrl Pts',(-15.5,13.9197595264192,-0.0129798765519497));
#26259=CARTESIAN_POINT('Ctrl Pts',(-14.5876477371938,13.9197595264192,-0.0546465432186153));
#26260=CARTESIAN_POINT('Ctrl Pts',(-14.1314716057906,14.7098797632096,-0.0963132098852826));
#26261=CARTESIAN_POINT('Ctrl Pts',(-13.6752954743875,15.5,-0.13797987655195));
#26262=CARTESIAN_POINT('Ctrl Pts',(-14.1314716057906,16.2901202367904,-0.179646543218617));
#26263=CARTESIAN_POINT('Ctrl Pts',(-14.5876477371938,17.0802404735808,-0.221313209885284));
#26264=CARTESIAN_POINT('Ctrl Pts',(-15.5,17.0802404735808,-0.262979876551952));
#26265=CARTESIAN_POINT('Ctrl Pts',(-16.4123522628062,17.0802404735808,-0.304646543218619));
#26266=CARTESIAN_POINT('Ctrl Pts',(-16.8685283942094,16.2901202367904,-0.346313209885286));
#26267=CARTESIAN_POINT('Ctrl Pts',(-17.3247045256125,15.5,-0.387979876551954));
#26268=CARTESIAN_POINT('Ctrl Pts',(-16.8685283942094,14.7098797632096,-0.429646543218621));
#26269=CARTESIAN_POINT('Ctrl Pts',(-16.4123522628062,13.9197595264192,-0.471313209885288));
#26270=CARTESIAN_POINT('Ctrl Pts',(-15.5,13.9197595264192,-0.512979876551955));
#26271=CARTESIAN_POINT('Ctrl Pts',(-14.5876477371938,13.9197595264192,-0.554646543218623));
#26272=CARTESIAN_POINT('Ctrl Pts',(-14.1314716057906,14.7098797632096,-0.59631320988529));
#26273=CARTESIAN_POINT('Ctrl Pts',(-13.6752954743875,15.5,-0.637979876551957));
#26274=CARTESIAN_POINT('Ctrl Pts',(-14.1314716057906,16.2901202367904,-0.679646543218624));
#26275=CARTESIAN_POINT('Ctrl Pts',(-14.5876477371938,17.0802404735808,-0.721313209885292));
#26276=CARTESIAN_POINT('Ctrl Pts',(-15.5,17.0802404735808,-0.762979876551959));
#26277=CARTESIAN_POINT('Ctrl Pts',(-16.4123522628062,17.0802404735808,-0.804646543218627));
#26278=CARTESIAN_POINT('Ctrl Pts',(-16.8685283942094,16.2901202367904,-0.846313209885294));
#26279=CARTESIAN_POINT('Ctrl Pts',(-17.3247045256125,15.5,-0.887979876551961));
#26280=CARTESIAN_POINT('Ctrl Pts',(-16.8685283942094,14.7098797632096,-0.929646543218628));
#26281=CARTESIAN_POINT('Ctrl Pts',(-16.4123522628062,13.9197595264192,-0.971313209885295));
#26282=CARTESIAN_POINT('Ctrl Pts',(-15.5,13.9197595264192,-1.01297987655196));
#26283=CARTESIAN_POINT('Ctrl Pts',(-14.5876477371938,13.9197595264192,-1.05464654321863));
#26284=CARTESIAN_POINT('Ctrl Pts',(-14.1314716057906,14.7098797632096,-1.0963132098853));
#26285=CARTESIAN_POINT('Ctrl Pts',(-13.6752954743875,15.5,-1.13797987655196));
#26286=CARTESIAN_POINT('Ctrl Pts',(-14.1314716057906,16.2901202367904,-1.17964654321863));
#26287=CARTESIAN_POINT('Ctrl Pts',(-14.5876477371938,17.0802404735808,-1.2213132098853));
#26288=CARTESIAN_POINT('Ctrl Pts',(-15.5,17.0802404735808,-1.26297987655196));
#26289=CARTESIAN_POINT('Ctrl Pts',(-16.4123522628062,17.0802404735808,-1.30464654321863));
#26290=CARTESIAN_POINT('Ctrl Pts',(-16.8685283942094,16.2901202367904,-1.3463132098853));
#26291=CARTESIAN_POINT('Ctrl Pts',(-17.3247045256125,15.5,-1.38797987655197));
#26292=CARTESIAN_POINT('Ctrl Pts',(-16.8685283942094,14.7098797632096,-1.42964654321863));
#26293=CARTESIAN_POINT('Ctrl Pts',(-16.4123522628062,13.9197595264192,-1.4713132098853));
#26294=CARTESIAN_POINT('Ctrl Pts',(-15.5,13.9197595264192,-1.51297987655197));
#26295=CARTESIAN_POINT('Ctrl Pts',(-14.5876477371938,13.9197595264192,-1.55464654321864));
#26296=CARTESIAN_POINT('Ctrl Pts',(-14.1314716057906,14.7098797632096,-1.5963132098853));
#26297=CARTESIAN_POINT('Ctrl Pts',(-13.6752954743875,15.5,-1.63797987655197));
#26298=CARTESIAN_POINT('Ctrl Pts',(-14.1314716057906,16.2901202367904,-1.67964654321864));
#26299=CARTESIAN_POINT('Ctrl Pts',(-14.5876477371938,17.0802404735808,-1.7213132098853));
#26300=CARTESIAN_POINT('Ctrl Pts',(-15.5,17.0802404735808,-1.76297987655197));
#26301=CARTESIAN_POINT('Ctrl Pts',(-16.4123522628062,17.0802404735808,-1.80464654321864));
#26302=CARTESIAN_POINT('Ctrl Pts',(-16.8685283942094,16.2901202367904,-1.84631320988531));
#26303=CARTESIAN_POINT('Ctrl Pts',(-17.3247045256125,15.5,-1.88797987655197));
#26304=CARTESIAN_POINT('Ctrl Pts',(-16.8685283942094,14.7098797632096,-1.92964654321864));
#26305=CARTESIAN_POINT('Ctrl Pts',(-16.700583153372,14.4189900731899,-1.94498649173085));
#26306=CARTESIAN_POINT('Ctrl Pts',(-16.4288420454487,14.2215586016756,-1.96260250461286));
#26307=CARTESIAN_POINT('Ctrl Pts',(-15.3465777998745,13.4352476007234,-2.03276185973389));
#26308=CARTESIAN_POINT('Ctrl Pts',(-14.2643135543003,12.6489365997713,-2.10292121485492));
#26309=CARTESIAN_POINT('Ctrl Pts',(-15.5,17.0802404735808,11.1745));
#26310=CARTESIAN_POINT('Ctrl Pts',(-16.4123522628062,17.0802404735808,11.1328333333333));
#26311=CARTESIAN_POINT('Ctrl Pts',(-16.8685283942094,16.2901202367904,11.0911666666667));
#26312=CARTESIAN_POINT('Ctrl Pts',(-17.3247045256125,15.5,11.0495));
#26313=CARTESIAN_POINT('Ctrl Pts',(-16.8685283942094,14.7098797632096,11.0078333333333));
#26314=CARTESIAN_POINT('Ctrl Pts',(-16.4123522628062,13.9197595264192,10.9661666666667));
#26315=CARTESIAN_POINT('Ctrl Pts',(-15.5,13.9197595264192,10.9245));
#26316=CARTESIAN_POINT('Ctrl Pts',(-14.5876477371938,13.9197595264192,10.8828333333333));
#26317=CARTESIAN_POINT('Ctrl Pts',(-14.1314716057906,14.7098797632096,10.8411666666667));
#26318=CARTESIAN_POINT('Ctrl Pts',(-13.6752954743875,15.5,10.7995));
#26319=CARTESIAN_POINT('Ctrl Pts',(-14.1314716057906,16.2901202367904,10.7578333333333));
#26320=CARTESIAN_POINT('Ctrl Pts',(-14.5876477371938,17.0802404735808,10.7161666666667));
#26321=CARTESIAN_POINT('Ctrl Pts',(-15.5,17.0802404735808,10.6745));
#26322=CARTESIAN_POINT('Ctrl Pts',(-16.4123522628062,17.0802404735808,10.6328333333333));
#26323=CARTESIAN_POINT('Ctrl Pts',(-16.8685283942094,16.2901202367904,10.5911666666667));
#26324=CARTESIAN_POINT('Ctrl Pts',(-17.3247045256125,15.5,10.5495));
#26325=CARTESIAN_POINT('Ctrl Pts',(-16.8685283942094,14.7098797632096,10.5078333333333));
#26326=CARTESIAN_POINT('Ctrl Pts',(-16.4123522628062,13.9197595264192,10.4661666666667));
#26327=CARTESIAN_POINT('Ctrl Pts',(-15.5,13.9197595264192,10.4245));
#26328=CARTESIAN_POINT('Ctrl Pts',(-14.5876477371938,13.9197595264192,10.3828333333333));
#26329=CARTESIAN_POINT('Ctrl Pts',(-14.1314716057906,14.7098797632096,10.3411666666667));
#26330=CARTESIAN_POINT('Ctrl Pts',(-13.6752954743875,15.5,10.2995));
#26331=CARTESIAN_POINT('Ctrl Pts',(-14.1314716057906,16.2901202367904,10.2578333333333));
#26332=CARTESIAN_POINT('Ctrl Pts',(-14.5876477371938,17.0802404735808,10.2161666666667));
#26333=CARTESIAN_POINT('Ctrl Pts',(-15.5,17.0802404735808,10.1745));
#26334=CARTESIAN_POINT('Ctrl Pts',(-16.4123522628062,17.0802404735808,10.1328333333333));
#26335=CARTESIAN_POINT('Ctrl Pts',(-16.8685283942094,16.2901202367904,10.0911666666667));
#26336=CARTESIAN_POINT('Ctrl Pts',(-17.3247045256125,15.5,10.0495));
#26337=CARTESIAN_POINT('Ctrl Pts',(-16.8685283942094,14.7098797632096,10.0078333333333));
#26338=CARTESIAN_POINT('Ctrl Pts',(-16.4123522628062,13.9197595264192,9.96616666666665));
#26339=CARTESIAN_POINT('Ctrl Pts',(-15.5,13.9197595264192,9.92449999999998));
#26340=CARTESIAN_POINT('Ctrl Pts',(-14.5876477371938,13.9197595264192,9.88283333333331));
#26341=CARTESIAN_POINT('Ctrl Pts',(-14.1314716057906,14.7098797632096,9.84116666666665));
#26342=CARTESIAN_POINT('Ctrl Pts',(-13.6752954743875,15.5,9.79949999999998));
#26343=CARTESIAN_POINT('Ctrl Pts',(-14.1314716057906,16.2901202367904,9.75783333333331));
#26344=CARTESIAN_POINT('Ctrl Pts',(-14.5876477371938,17.0802404735808,9.71616666666665));
#26345=CARTESIAN_POINT('Ctrl Pts',(-15.5,17.0802404735808,9.67449999999998));
#26346=CARTESIAN_POINT('Ctrl Pts',(-16.4123522628062,17.0802404735808,9.63283333333331));
#26347=CARTESIAN_POINT('Ctrl Pts',(-16.8685283942094,16.2901202367904,9.59116666666664));
#26348=CARTESIAN_POINT('Ctrl Pts',(-17.3247045256125,15.5,9.54949999999998));
#26349=CARTESIAN_POINT('Ctrl Pts',(-16.8685283942094,14.7098797632096,9.50783333333331));
#26350=CARTESIAN_POINT('Ctrl Pts',(-16.4123522628062,13.9197595264192,9.46616666666664));
#26351=CARTESIAN_POINT('Ctrl Pts',(-15.5,13.9197595264192,9.42449999999998));
#26352=CARTESIAN_POINT('Ctrl Pts',(-14.5876477371938,13.9197595264192,9.38283333333331));
#26353=CARTESIAN_POINT('Ctrl Pts',(-14.1314716057906,14.7098797632096,9.34116666666664));
#26354=CARTESIAN_POINT('Ctrl Pts',(-13.6752954743875,15.5,9.29949999999998));
#26355=CARTESIAN_POINT('Ctrl Pts',(-14.1314716057906,16.2901202367904,9.25783333333331));
#26356=CARTESIAN_POINT('Ctrl Pts',(-14.5876477371938,17.0802404735808,9.21616666666664));
#26357=CARTESIAN_POINT('Ctrl Pts',(-15.5,17.0802404735808,9.17449999999997));
#26358=CARTESIAN_POINT('Ctrl Pts',(-16.4123522628062,17.0802404735808,9.13283333333331));
#26359=CARTESIAN_POINT('Ctrl Pts',(-16.8685283942094,16.2901202367904,9.09116666666664));
#26360=CARTESIAN_POINT('Ctrl Pts',(-17.3247045256125,15.5,9.04949999999997));
#26361=CARTESIAN_POINT('Ctrl Pts',(-16.8685283942094,14.7098797632096,9.0078333333333));
#26362=CARTESIAN_POINT('Ctrl Pts',(-16.4123522628062,13.9197595264192,8.96616666666664));
#26363=CARTESIAN_POINT('Ctrl Pts',(-15.5,13.9197595264192,8.92449999999997));
#26364=CARTESIAN_POINT('Ctrl Pts',(-14.5876477371938,13.9197595264192,8.8828333333333));
#26365=CARTESIAN_POINT('Ctrl Pts',(-14.1314716057906,14.7098797632096,8.84116666666664));
#26366=CARTESIAN_POINT('Ctrl Pts',(-13.6752954743875,15.5,8.79949999999997));
#26367=CARTESIAN_POINT('Ctrl Pts',(-14.1314716057906,16.2901202367904,8.7578333333333));
#26368=CARTESIAN_POINT('Ctrl Pts',(-14.5876477371938,17.0802404735808,8.71616666666663));
#26369=CARTESIAN_POINT('Ctrl Pts',(-15.5,17.0802404735808,8.67449999999997));
#26370=CARTESIAN_POINT('Ctrl Pts',(-16.4123522628062,17.0802404735808,8.6328333333333));
#26371=CARTESIAN_POINT('Ctrl Pts',(-16.8685283942094,16.2901202367904,8.59116666666663));
#26372=CARTESIAN_POINT('Ctrl Pts',(-17.3247045256125,15.5,8.54949999999996));
#26373=CARTESIAN_POINT('Ctrl Pts',(-16.8685283942094,14.7098797632096,8.50783333333329));
#26374=CARTESIAN_POINT('Ctrl Pts',(-16.4123522628062,13.9197595264192,8.46616666666663));
#26375=CARTESIAN_POINT('Ctrl Pts',(-15.5,13.9197595264192,8.42449999999996));
#26376=CARTESIAN_POINT('Ctrl Pts',(-14.5876477371938,13.9197595264192,8.3828333333333));
#26377=CARTESIAN_POINT('Ctrl Pts',(-14.1314716057906,14.7098797632096,8.34116666666663));
#26378=CARTESIAN_POINT('Ctrl Pts',(-13.6752954743875,15.5,8.29949999999996));
#26379=CARTESIAN_POINT('Ctrl Pts',(-14.1314716057906,16.2901202367904,8.25783333333329));
#26380=CARTESIAN_POINT('Ctrl Pts',(-14.5876477371938,17.0802404735808,8.21616666666663));
#26381=CARTESIAN_POINT('Ctrl Pts',(-15.5,17.0802404735808,8.17449999999996));
#26382=CARTESIAN_POINT('Ctrl Pts',(-16.4123522628062,17.0802404735808,8.13283333333329));
#26383=CARTESIAN_POINT('Ctrl Pts',(-16.8685283942094,16.2901202367904,8.09116666666663));
#26384=CARTESIAN_POINT('Ctrl Pts',(-17.3247045256125,15.5,8.04949999999996));
#26385=CARTESIAN_POINT('Ctrl Pts',(-16.8685283942094,14.7098797632096,8.00783333333329));
#26386=CARTESIAN_POINT('Ctrl Pts',(-16.4123522628062,13.9197595264192,7.96616666666662));
#26387=CARTESIAN_POINT('Ctrl Pts',(-15.5,13.9197595264192,7.92449999999996));
#26388=CARTESIAN_POINT('Ctrl Pts',(-14.5876477371938,13.9197595264192,7.88283333333329));
#26389=CARTESIAN_POINT('Ctrl Pts',(-14.1314716057906,14.7098797632096,7.84116666666662));
#26390=CARTESIAN_POINT('Ctrl Pts',(-13.6752954743875,15.5,7.79949999999995));
#26391=CARTESIAN_POINT('Ctrl Pts',(-14.1314716057906,16.2901202367904,7.75783333333329));
#26392=CARTESIAN_POINT('Ctrl Pts',(-14.5876477371938,17.0802404735808,7.71616666666662));
#26393=CARTESIAN_POINT('Ctrl Pts',(-15.5,17.0802404735808,7.67449999999995));
#26394=CARTESIAN_POINT('Ctrl Pts',(-16.4123522628062,17.0802404735808,7.63283333333328));
#26395=CARTESIAN_POINT('Ctrl Pts',(-16.8685283942094,16.2901202367904,7.59116666666662));
#26396=CARTESIAN_POINT('Ctrl Pts',(-17.3247045256125,15.5,7.54949999999995));
#26397=CARTESIAN_POINT('Ctrl Pts',(-16.8685283942094,14.7098797632096,7.50783333333328));
#26398=CARTESIAN_POINT('Ctrl Pts',(-16.4123522628062,13.9197595264192,7.46616666666662));
#26399=CARTESIAN_POINT('Ctrl Pts',(-15.5,13.9197595264192,7.42449999999995));
#26400=CARTESIAN_POINT('Ctrl Pts',(-14.5876477371938,13.9197595264192,7.38283333333328));
#26401=CARTESIAN_POINT('Ctrl Pts',(-14.1314716057906,14.7098797632096,7.34116666666661));
#26402=CARTESIAN_POINT('Ctrl Pts',(-13.6752954743875,15.5,7.29949999999995));
#26403=CARTESIAN_POINT('Ctrl Pts',(-14.1314716057906,16.2901202367904,7.25783333333328));
#26404=CARTESIAN_POINT('Ctrl Pts',(-14.5876477371938,17.0802404735808,7.21616666666661));
#26405=CARTESIAN_POINT('Ctrl Pts',(-15.5,17.0802404735808,7.17449999999995));
#26406=CARTESIAN_POINT('Ctrl Pts',(-16.4123522628062,17.0802404735808,7.13283333333328));
#26407=CARTESIAN_POINT('Ctrl Pts',(-16.8685283942094,16.2901202367904,7.09116666666661));
#26408=CARTESIAN_POINT('Ctrl Pts',(-17.3247045256125,15.5,7.04949999999994));
#26409=CARTESIAN_POINT('Ctrl Pts',(-16.8685283942094,14.7098797632096,7.00783333333328));
#26410=CARTESIAN_POINT('Ctrl Pts',(-16.4123522628062,13.9197595264192,6.96616666666661));
#26411=CARTESIAN_POINT('Ctrl Pts',(-15.5,13.9197595264192,6.92449999999994));
#26412=CARTESIAN_POINT('Ctrl Pts',(-14.5876477371938,13.9197595264192,6.88283333333327));
#26413=CARTESIAN_POINT('Ctrl Pts',(-14.1314716057906,14.7098797632096,6.84116666666661));
#26414=CARTESIAN_POINT('Ctrl Pts',(-13.6752954743875,15.5,6.79949999999994));
#26415=CARTESIAN_POINT('Ctrl Pts',(-14.1314716057906,16.2901202367904,6.75783333333327));
#26416=CARTESIAN_POINT('Ctrl Pts',(-14.5876477371938,17.0802404735808,6.71616666666661));
#26417=CARTESIAN_POINT('Ctrl Pts',(-15.5,17.0802404735808,6.67449999999994));
#26418=CARTESIAN_POINT('Ctrl Pts',(-16.4123522628062,17.0802404735808,6.63283333333327));
#26419=CARTESIAN_POINT('Ctrl Pts',(-16.8685283942094,16.2901202367904,6.59116666666661));
#26420=CARTESIAN_POINT('Ctrl Pts',(-17.3247045256125,15.5,6.54949999999994));
#26421=CARTESIAN_POINT('Ctrl Pts',(-16.8685283942094,14.7098797632096,6.50783333333327));
#26422=CARTESIAN_POINT('Ctrl Pts',(-16.4123522628062,13.9197595264192,6.4661666666666));
#26423=CARTESIAN_POINT('Ctrl Pts',(-15.5,13.9197595264192,6.42449999999994));
#26424=CARTESIAN_POINT('Ctrl Pts',(-14.5876477371938,13.9197595264192,6.38283333333327));
#26425=CARTESIAN_POINT('Ctrl Pts',(-14.1314716057906,14.7098797632096,6.3411666666666));
#26426=CARTESIAN_POINT('Ctrl Pts',(-13.6752954743875,15.5,6.29949999999993));
#26427=CARTESIAN_POINT('Ctrl Pts',(-14.1314716057906,16.2901202367904,6.25783333333327));
#26428=CARTESIAN_POINT('Ctrl Pts',(-14.5876477371938,17.0802404735808,6.2161666666666));
#26429=CARTESIAN_POINT('Ctrl Pts',(-15.5,17.0802404735808,6.17449999999993));
#26430=CARTESIAN_POINT('Ctrl Pts',(-16.4123522628062,17.0802404735808,6.13283333333326));
#26431=CARTESIAN_POINT('Ctrl Pts',(-16.8685283942094,16.2901202367904,6.0911666666666));
#26432=CARTESIAN_POINT('Ctrl Pts',(-17.3247045256125,15.5,6.04949999999993));
#26433=CARTESIAN_POINT('Ctrl Pts',(-16.8685283942094,14.7098797632096,6.00783333333326));
#26434=CARTESIAN_POINT('Ctrl Pts',(-16.4123522628062,13.9197595264192,5.9661666666666));
#26435=CARTESIAN_POINT('Ctrl Pts',(-15.5,13.9197595264192,5.92449999999993));
#26436=CARTESIAN_POINT('Ctrl Pts',(-14.5876477371938,13.9197595264192,5.88283333333326));
#26437=CARTESIAN_POINT('Ctrl Pts',(-14.1314716057906,14.7098797632096,5.8411666666666));
#26438=CARTESIAN_POINT('Ctrl Pts',(-13.6752954743875,15.5,5.79949999999993));
#26439=CARTESIAN_POINT('Ctrl Pts',(-14.1314716057906,16.2901202367904,5.75783333333326));
#26440=CARTESIAN_POINT('Ctrl Pts',(-14.5876477371938,17.0802404735808,5.71616666666659));
#26441=CARTESIAN_POINT('Ctrl Pts',(-15.5,17.0802404735808,5.67449999999993));
#26442=CARTESIAN_POINT('Ctrl Pts',(-16.4123522628062,17.0802404735808,5.63283333333326));
#26443=CARTESIAN_POINT('Ctrl Pts',(-16.8685283942094,16.2901202367904,5.59116666666659));
#26444=CARTESIAN_POINT('Ctrl Pts',(-17.3247045256125,15.5,5.54949999999992));
#26445=CARTESIAN_POINT('Ctrl Pts',(-16.8685283942094,14.7098797632096,5.50783333333326));
#26446=CARTESIAN_POINT('Ctrl Pts',(-16.4123522628062,13.9197595264192,5.46616666666659));
#26447=CARTESIAN_POINT('Ctrl Pts',(-15.5,13.9197595264192,5.42449999999992));
#26448=CARTESIAN_POINT('Ctrl Pts',(-14.5876477371938,13.9197595264192,5.38283333333326));
#26449=CARTESIAN_POINT('Ctrl Pts',(-14.1314716057906,14.7098797632096,5.34116666666659));
#26450=CARTESIAN_POINT('Ctrl Pts',(-13.6752954743875,15.5,5.29949999999992));
#26451=CARTESIAN_POINT('Ctrl Pts',(-14.1314716057906,16.2901202367904,5.25783333333325));
#26452=CARTESIAN_POINT('Ctrl Pts',(-14.5876477371938,17.0802404735808,5.21616666666659));
#26453=CARTESIAN_POINT('Ctrl Pts',(-15.5,17.0802404735808,5.17449999999992));
#26454=CARTESIAN_POINT('Ctrl Pts',(-16.4123522628062,17.0802404735808,5.13283333333325));
#26455=CARTESIAN_POINT('Ctrl Pts',(-16.8685283942094,16.2901202367904,5.09116666666658));
#26456=CARTESIAN_POINT('Ctrl Pts',(-17.3247045256125,15.5,5.04949999999992));
#26457=CARTESIAN_POINT('Ctrl Pts',(-16.8685283942094,14.7098797632096,5.00783333333325));
#26458=CARTESIAN_POINT('Ctrl Pts',(-16.4123522628062,13.9197595264192,4.96616666666658));
#26459=CARTESIAN_POINT('Ctrl Pts',(-15.5,13.9197595264192,4.92449999999992));
#26460=CARTESIAN_POINT('Ctrl Pts',(-14.5876477371938,13.9197595264192,4.88283333333325));
#26461=CARTESIAN_POINT('Ctrl Pts',(-14.1314716057906,14.7098797632096,4.84116666666658));
#26462=CARTESIAN_POINT('Ctrl Pts',(-13.6752954743875,15.5,4.79949999999991));
#26463=CARTESIAN_POINT('Ctrl Pts',(-14.1314716057906,16.2901202367904,4.75783333333325));
#26464=CARTESIAN_POINT('Ctrl Pts',(-14.5876477371938,17.0802404735808,4.71616666666658));
#26465=CARTESIAN_POINT('Ctrl Pts',(-15.5,17.0802404735808,4.67449999999991));
#26466=CARTESIAN_POINT('Ctrl Pts',(-16.4123522628062,17.0802404735808,4.63283333333324));
#26467=CARTESIAN_POINT('Ctrl Pts',(-16.8685283942094,16.2901202367904,4.59116666666658));
#26468=CARTESIAN_POINT('Ctrl Pts',(-17.3247045256125,15.5,4.54949999999991));
#26469=CARTESIAN_POINT('Ctrl Pts',(-16.8685283942094,14.7098797632096,4.50783333333324));
#26470=CARTESIAN_POINT('Ctrl Pts',(-16.4123522628062,13.9197595264192,4.46616666666658));
#26471=CARTESIAN_POINT('Ctrl Pts',(-15.5,13.9197595264192,4.42449999999991));
#26472=CARTESIAN_POINT('Ctrl Pts',(-14.5876477371938,13.9197595264192,4.38283333333324));
#26473=CARTESIAN_POINT('Ctrl Pts',(-14.1314716057906,14.7098797632096,4.34116666666657));
#26474=CARTESIAN_POINT('Ctrl Pts',(-13.6752954743875,15.5,4.29949999999991));
#26475=CARTESIAN_POINT('Ctrl Pts',(-14.1314716057906,16.2901202367904,4.25783333333324));
#26476=CARTESIAN_POINT('Ctrl Pts',(-14.5876477371938,17.0802404735808,4.21616666666657));
#26477=CARTESIAN_POINT('Ctrl Pts',(-15.5,17.0802404735808,4.17449999999991));
#26478=CARTESIAN_POINT('Ctrl Pts',(-16.4123522628062,17.0802404735808,4.13283333333324));
#26479=CARTESIAN_POINT('Ctrl Pts',(-16.8685283942094,16.2901202367904,4.09116666666657));
#26480=CARTESIAN_POINT('Ctrl Pts',(-17.3247045256125,15.5,4.0494999999999));
#26481=CARTESIAN_POINT('Ctrl Pts',(-16.8685283942094,14.7098797632096,4.00783333333324));
#26482=CARTESIAN_POINT('Ctrl Pts',(-16.4123522628062,13.9197595264192,3.96616666666657));
#26483=CARTESIAN_POINT('Ctrl Pts',(-15.5,13.9197595264192,3.9244999999999));
#26484=CARTESIAN_POINT('Ctrl Pts',(-14.5876477371938,13.9197595264192,3.88283333333323));
#26485=CARTESIAN_POINT('Ctrl Pts',(-14.1314716057906,14.7098797632096,3.84116666666657));
#26486=CARTESIAN_POINT('Ctrl Pts',(-13.6752954743875,15.5,3.7994999999999));
#26487=CARTESIAN_POINT('Ctrl Pts',(-14.1314716057906,16.2901202367904,3.75783333333323));
#26488=CARTESIAN_POINT('Ctrl Pts',(-14.5876477371938,17.0802404735808,3.71616666666657));
#26489=CARTESIAN_POINT('Ctrl Pts',(-15.5,17.0802404735808,3.6744999999999));
#26490=CARTESIAN_POINT('Ctrl Pts',(-16.4123522628062,17.0802404735808,3.63283333333323));
#26491=CARTESIAN_POINT('Ctrl Pts',(-16.8685283942094,16.2901202367904,3.59116666666656));
#26492=CARTESIAN_POINT('Ctrl Pts',(-17.3247045256125,15.5,3.5494999999999));
#26493=CARTESIAN_POINT('Ctrl Pts',(-16.8685283942094,14.7098797632096,3.50783333333323));
#26494=CARTESIAN_POINT('Ctrl Pts',(-16.4123522628062,13.9197595264192,3.46616666666656));
#26495=CARTESIAN_POINT('Ctrl Pts',(-15.5,13.9197595264192,3.4244999999999));
#26496=CARTESIAN_POINT('Ctrl Pts',(-14.5876477371938,13.9197595264192,3.38283333333323));
#26497=CARTESIAN_POINT('Ctrl Pts',(-14.1314716057906,14.7098797632096,3.34116666666656));
#26498=CARTESIAN_POINT('Ctrl Pts',(-13.6752954743875,15.5,3.29949999999989));
#26499=CARTESIAN_POINT('Ctrl Pts',(-14.1314716057906,16.2901202367904,3.25783333333323));
#26500=CARTESIAN_POINT('Ctrl Pts',(-14.5876477371938,17.0802404735808,3.21616666666656));
#26501=CARTESIAN_POINT('Ctrl Pts',(-15.5,17.0802404735808,3.17449999999989));
#26502=CARTESIAN_POINT('Ctrl Pts',(-16.4123522628062,17.0802404735808,3.13283333333323));
#26503=CARTESIAN_POINT('Ctrl Pts',(-16.8685283942094,16.2901202367904,3.09116666666656));
#26504=CARTESIAN_POINT('Ctrl Pts',(-17.3247045256125,15.5,3.04949999999989));
#26505=CARTESIAN_POINT('Ctrl Pts',(-16.8685283942094,14.7098797632096,3.00783333333322));
#26506=CARTESIAN_POINT('Ctrl Pts',(-16.4123522628062,13.9197595264192,2.96616666666656));
#26507=CARTESIAN_POINT('Ctrl Pts',(-15.5,13.9197595264192,2.92449999999989));
#26508=CARTESIAN_POINT('Ctrl Pts',(-14.5876477371938,13.9197595264192,2.88283333333322));
#26509=CARTESIAN_POINT('Ctrl Pts',(-14.1314716057906,14.7098797632096,2.84116666666655));
#26510=CARTESIAN_POINT('Ctrl Pts',(-13.6752954743875,15.5,2.79949999999989));
#26511=CARTESIAN_POINT('Ctrl Pts',(-14.1314716057906,16.2901202367904,2.75783333333322));
#26512=CARTESIAN_POINT('Ctrl Pts',(-14.5876477371938,17.0802404735808,2.71616666666655));
#26513=CARTESIAN_POINT('Ctrl Pts',(-15.5,17.0802404735808,2.67449999999989));
#26514=CARTESIAN_POINT('Ctrl Pts',(-16.4123522628062,17.0802404735808,2.63283333333322));
#26515=CARTESIAN_POINT('Ctrl Pts',(-16.8685283942094,16.2901202367904,2.59116666666655));
#26516=CARTESIAN_POINT('Ctrl Pts',(-17.3247045256125,15.5,2.54949999999988));
#26517=CARTESIAN_POINT('Ctrl Pts',(-16.8685283942094,14.7098797632096,2.50783333333322));
#26518=CARTESIAN_POINT('Ctrl Pts',(-16.4123522628062,13.9197595264192,2.46616666666655));
#26519=CARTESIAN_POINT('Ctrl Pts',(-15.5,13.9197595264192,2.42449999999988));
#26520=CARTESIAN_POINT('Ctrl Pts',(-14.5876477371938,13.9197595264192,2.38283333333321));
#26521=CARTESIAN_POINT('Ctrl Pts',(-14.1314716057906,14.7098797632096,2.34116666666655));
#26522=CARTESIAN_POINT('Ctrl Pts',(-13.6752954743875,15.5,2.29949999999988));
#26523=CARTESIAN_POINT('Ctrl Pts',(-14.1314716057906,16.2901202367904,2.25783333333321));
#26524=CARTESIAN_POINT('Ctrl Pts',(-14.5876477371938,17.0802404735808,2.21616666666655));
#26525=CARTESIAN_POINT('Ctrl Pts',(-15.5,17.0802404735808,2.17449999999988));
#26526=CARTESIAN_POINT('Ctrl Pts',(-16.4123522628062,17.0802404735808,2.13283333333321));
#26527=CARTESIAN_POINT('Ctrl Pts',(-16.8685283942094,16.2901202367904,2.09116666666655));
#26528=CARTESIAN_POINT('Ctrl Pts',(-17.3247045256125,15.5,2.04949999999988));
#26529=CARTESIAN_POINT('Ctrl Pts',(-16.8685283942094,14.7098797632096,2.00783333333321));
#26530=CARTESIAN_POINT('Ctrl Pts',(-16.4123522628062,13.9197595264192,1.96616666666654));
#26531=CARTESIAN_POINT('Ctrl Pts',(-15.5,13.9197595264192,1.92449999999988));
#26532=CARTESIAN_POINT('Ctrl Pts',(-14.5876477371938,13.9197595264192,1.88283333333321));
#26533=CARTESIAN_POINT('Ctrl Pts',(-14.1314716057906,14.7098797632096,1.84116666666654));
#26534=CARTESIAN_POINT('Ctrl Pts',(-13.6752954743875,15.5,1.79949999999987));
#26535=CARTESIAN_POINT('Ctrl Pts',(-14.1314716057906,16.2901202367904,1.75783333333321));
#26536=CARTESIAN_POINT('Ctrl Pts',(-14.5876477371938,17.0802404735808,1.71616666666654));
#26537=CARTESIAN_POINT('Ctrl Pts',(-15.5,17.0802404735808,1.67449999999987));
#26538=CARTESIAN_POINT('Ctrl Pts',(-16.4123522628062,17.0802404735808,1.63283333333321));
#26539=CARTESIAN_POINT('Ctrl Pts',(-16.8685283942094,16.2901202367904,1.59116666666654));
#26540=CARTESIAN_POINT('Ctrl Pts',(-17.3247045256125,15.5,1.54949999999987));
#26541=CARTESIAN_POINT('Ctrl Pts',(-16.8685283942094,14.7098797632096,1.5078333333332));
#26542=CARTESIAN_POINT('Ctrl Pts',(-16.4123522628062,13.9197595264192,1.46616666666654));
#26543=CARTESIAN_POINT('Ctrl Pts',(-15.5,13.9197595264192,1.42449999999987));
#26544=CARTESIAN_POINT('Ctrl Pts',(-14.5876477371938,13.9197595264192,1.3828333333332));
#26545=CARTESIAN_POINT('Ctrl Pts',(-14.1314716057906,14.7098797632096,1.34116666666653));
#26546=CARTESIAN_POINT('Ctrl Pts',(-13.6752954743875,15.5,1.29949999999987));
#26547=CARTESIAN_POINT('Ctrl Pts',(-14.1314716057906,16.2901202367904,1.2578333333332));
#26548=CARTESIAN_POINT('Ctrl Pts',(-14.5876477371938,17.0802404735808,1.21616666666653));
#26549=CARTESIAN_POINT('Ctrl Pts',(-15.5,17.0802404735808,1.17449999999986));
#26550=CARTESIAN_POINT('Ctrl Pts',(-16.4123522628062,17.0802404735808,1.1328333333332));
#26551=CARTESIAN_POINT('Ctrl Pts',(-16.8685283942094,16.2901202367904,1.09116666666653));
#26552=CARTESIAN_POINT('Ctrl Pts',(-17.3247045256125,15.5,1.04949999999986));
#26553=CARTESIAN_POINT('Ctrl Pts',(-16.8685283942094,14.7098797632096,1.0078333333332));
#26554=CARTESIAN_POINT('Ctrl Pts',(-16.4123522628062,13.9197595264192,0.96616666666653));
#26555=CARTESIAN_POINT('Ctrl Pts',(-15.5,13.9197595264192,0.924499999999863));
#26556=CARTESIAN_POINT('Ctrl Pts',(-14.5876477371938,13.9197595264192,0.882833333333196));
#26557=CARTESIAN_POINT('Ctrl Pts',(-14.1314716057906,14.7098797632096,0.841166666666529));
#26558=CARTESIAN_POINT('Ctrl Pts',(-13.6752954743875,15.5,0.799499999999861));
#26559=CARTESIAN_POINT('Ctrl Pts',(-14.1314716057906,16.2901202367904,0.757833333333194));
#26560=CARTESIAN_POINT('Ctrl Pts',(-14.5876477371938,17.0802404735808,0.716166666666527));
#26561=CARTESIAN_POINT('Ctrl Pts',(-15.5,17.0802404735808,0.674499999999859));
#26562=CARTESIAN_POINT('Ctrl Pts',(-16.4123522628062,17.0802404735808,0.632833333333192));
#26563=CARTESIAN_POINT('Ctrl Pts',(-16.8685283942094,16.2901202367904,0.591166666666525));
#26564=CARTESIAN_POINT('Ctrl Pts',(-17.3247045256125,15.5,0.549499999999857));
#26565=CARTESIAN_POINT('Ctrl Pts',(-16.8685283942094,14.7098797632096,0.50783333333319));
#26566=CARTESIAN_POINT('Ctrl Pts',(-16.4123522628062,13.9197595264192,0.466166666666523));
#26567=CARTESIAN_POINT('Ctrl Pts',(-15.5,13.9197595264192,0.424499999999856));
#26568=CARTESIAN_POINT('Ctrl Pts',(-14.5876477371938,13.9197595264192,0.382833333333188));
#26569=CARTESIAN_POINT('Ctrl Pts',(-14.1314716057906,14.7098797632096,0.341166666666521));
#26570=CARTESIAN_POINT('Ctrl Pts',(-13.6752954743875,15.5,0.299499999999854));
#26571=CARTESIAN_POINT('Ctrl Pts',(-14.1314716057906,16.2901202367904,0.257833333333186));
#26572=CARTESIAN_POINT('Ctrl Pts',(-14.5876477371938,17.0802404735808,0.216166666666519));
#26573=CARTESIAN_POINT('Ctrl Pts',(-15.5,17.0802404735808,0.174499999999852));
#26574=CARTESIAN_POINT('Ctrl Pts',(-16.4123522628062,17.0802404735808,0.132833333333185));
#26575=CARTESIAN_POINT('Ctrl Pts',(-16.8685283942094,16.2901202367904,0.0911666666665173));
#26576=CARTESIAN_POINT('Ctrl Pts',(-17.3247045256125,15.5,0.04949999999985));
#26577=CARTESIAN_POINT('Ctrl Pts',(-16.8685283942094,14.7098797632096,0.00783333333318273));
#26578=CARTESIAN_POINT('Ctrl Pts',(-16.4123522628062,13.9197595264192,-0.0338333333334846));
#26579=CARTESIAN_POINT('Ctrl Pts',(-15.5,13.9197595264192,-0.0755000000001518));
#26580=CARTESIAN_POINT('Ctrl Pts',(-14.5876477371938,13.9197595264192,-0.117166666666817));
#26581=CARTESIAN_POINT('Ctrl Pts',(-14.1314716057906,14.7098797632096,-0.158833333333485));
#26582=CARTESIAN_POINT('Ctrl Pts',(-13.6752954743875,15.5,-0.200500000000152));
#26583=CARTESIAN_POINT('Ctrl Pts',(-14.1314716057906,16.2901202367904,-0.242166666666819));
#26584=CARTESIAN_POINT('Ctrl Pts',(-14.5876477371938,17.0802404735808,-0.283833333333486));
#26585=CARTESIAN_POINT('Ctrl Pts',(-15.5,17.0802404735808,-0.325500000000154));
#26586=CARTESIAN_POINT('Ctrl Pts',(-16.4123522628062,17.0802404735808,-0.367166666666821));
#26587=CARTESIAN_POINT('Ctrl Pts',(-16.8685283942094,16.2901202367904,-0.408833333333488));
#26588=CARTESIAN_POINT('Ctrl Pts',(-17.3247045256125,15.5,-0.450500000000156));
#26589=CARTESIAN_POINT('Ctrl Pts',(-16.8685283942094,14.7098797632096,-0.492166666666823));
#26590=CARTESIAN_POINT('Ctrl Pts',(-16.4123522628062,13.9197595264192,-0.53383333333349));
#26591=CARTESIAN_POINT('Ctrl Pts',(-15.5,13.9197595264192,-0.575500000000157));
#26592=CARTESIAN_POINT('Ctrl Pts',(-14.5876477371938,13.9197595264192,-0.617166666666825));
#26593=CARTESIAN_POINT('Ctrl Pts',(-14.1314716057906,14.7098797632096,-0.658833333333492));
#26594=CARTESIAN_POINT('Ctrl Pts',(-13.6752954743875,15.5,-0.700500000000159));
#26595=CARTESIAN_POINT('Ctrl Pts',(-14.1314716057906,16.2901202367904,-0.742166666666827));
#26596=CARTESIAN_POINT('Ctrl Pts',(-14.5876477371938,17.0802404735808,-0.783833333333494));
#26597=CARTESIAN_POINT('Ctrl Pts',(-15.5,17.0802404735808,-0.825500000000161));
#26598=CARTESIAN_POINT('Ctrl Pts',(-16.4123522628062,17.0802404735808,-0.867166666666829));
#26599=CARTESIAN_POINT('Ctrl Pts',(-16.8685283942094,16.2901202367904,-0.908833333333496));
#26600=CARTESIAN_POINT('Ctrl Pts',(-17.3247045256125,15.5,-0.950500000000163));
#26601=CARTESIAN_POINT('Ctrl Pts',(-16.8685283942094,14.7098797632096,-0.99216666666683));
#26602=CARTESIAN_POINT('Ctrl Pts',(-16.4123522628062,13.9197595264192,-1.0338333333335));
#26603=CARTESIAN_POINT('Ctrl Pts',(-15.5,13.9197595264192,-1.07550000000016));
#26604=CARTESIAN_POINT('Ctrl Pts',(-14.5876477371938,13.9197595264192,-1.11716666666683));
#26605=CARTESIAN_POINT('Ctrl Pts',(-14.1314716057906,14.7098797632096,-1.1588333333335));
#26606=CARTESIAN_POINT('Ctrl Pts',(-13.6752954743875,15.5,-1.20050000000017));
#26607=CARTESIAN_POINT('Ctrl Pts',(-14.1314716057906,16.2901202367904,-1.24216666666683));
#26608=CARTESIAN_POINT('Ctrl Pts',(-14.5876477371938,17.0802404735808,-1.2838333333335));
#26609=CARTESIAN_POINT('Ctrl Pts',(-15.5,17.0802404735808,-1.32550000000017));
#26610=CARTESIAN_POINT('Ctrl Pts',(-16.4123522628062,17.0802404735808,-1.36716666666683));
#26611=CARTESIAN_POINT('Ctrl Pts',(-16.8685283942094,16.2901202367904,-1.4088333333335));
#26612=CARTESIAN_POINT('Ctrl Pts',(-17.3247045256125,15.5,-1.45050000000017));
#26613=CARTESIAN_POINT('Ctrl Pts',(-16.8685283942094,14.7098797632096,-1.49216666666684));
#26614=CARTESIAN_POINT('Ctrl Pts',(-16.4123522628062,13.9197595264192,-1.5338333333335));
#26615=CARTESIAN_POINT('Ctrl Pts',(-15.5,13.9197595264192,-1.57550000000017));
#26616=CARTESIAN_POINT('Ctrl Pts',(-14.5876477371938,13.9197595264192,-1.61716666666684));
#26617=CARTESIAN_POINT('Ctrl Pts',(-14.1314716057906,14.7098797632096,-1.65883333333351));
#26618=CARTESIAN_POINT('Ctrl Pts',(-13.6752954743875,15.5,-1.70050000000017));
#26619=CARTESIAN_POINT('Ctrl Pts',(-14.1314716057906,16.2901202367904,-1.74216666666684));
#26620=CARTESIAN_POINT('Ctrl Pts',(-14.5876477371938,17.0802404735808,-1.78383333333351));
#26621=CARTESIAN_POINT('Ctrl Pts',(-15.5,17.0802404735808,-1.82550000000017));
#26622=CARTESIAN_POINT('Ctrl Pts',(-16.4123522628062,17.0802404735808,-1.86716666666684));
#26623=CARTESIAN_POINT('Ctrl Pts',(-16.8685283942094,16.2901202367904,-1.90883333333351));
#26624=CARTESIAN_POINT('Ctrl Pts',(-17.3247045256125,15.5,-1.95050000000018));
#26625=CARTESIAN_POINT('Ctrl Pts',(-16.8685283942094,14.7098797632096,-1.99216666666684));
#26626=CARTESIAN_POINT('Ctrl Pts',(-16.700583153372,14.4189900731899,-2.00750661517905));
#26627=CARTESIAN_POINT('Ctrl Pts',(-16.4288420454487,14.2215586016756,-2.02512262806106));
#26628=CARTESIAN_POINT('Ctrl Pts',(-15.3465777998745,13.4352476007234,-2.09528198318209));
#26629=CARTESIAN_POINT('Ctrl Pts',(-14.2643135543003,12.6489365997713,-2.16544133830312));
#26630=CARTESIAN_POINT('Origin',(0.,0.,1.3858));
#26631=CARTESIAN_POINT('',(16.96,21.2,1.3858));
#26632=CARTESIAN_POINT('',(-16.96,21.2,1.3858));
#26633=CARTESIAN_POINT('',(-21.2,21.2,1.3858));
#26634=CARTESIAN_POINT('',(21.2,16.96,1.3858));
#26635=CARTESIAN_POINT('',(16.96,21.2,1.3858));
#26636=CARTESIAN_POINT('',(21.2,-16.96,1.3858));
#26637=CARTESIAN_POINT('',(21.2,21.2,1.3858));
#26638=CARTESIAN_POINT('',(16.96,-21.2,1.3858));
#26639=CARTESIAN_POINT('',(16.96,-21.2,1.3858));
#26640=CARTESIAN_POINT('',(-16.96,-21.2,1.3858));
#26641=CARTESIAN_POINT('',(-21.2,-21.2,1.3858));
#26642=CARTESIAN_POINT('',(-21.2,-16.96,1.3858));
#26643=CARTESIAN_POINT('',(-16.96,-21.2,1.3858));
#26644=CARTESIAN_POINT('',(-21.2,16.96,1.3858));
#26645=CARTESIAN_POINT('',(-21.2,21.2,1.3858));
#26646=CARTESIAN_POINT('',(-16.96,21.2,1.3858));
#26647=CARTESIAN_POINT('Origin',(-15.6430062215132,-15.5080107655887,1.38580563032454));
#26648=CARTESIAN_POINT('Origin',(-15.4374167911874,-15.6296099418937,1.38577762513339));
#26649=CARTESIAN_POINT('Origin',(15.508010765588,-15.643006221513,1.38580563032419));
#26650=CARTESIAN_POINT('Origin',(15.6296099418937,-15.4374167911875,1.38577762513336));
#26651=CARTESIAN_POINT('Origin',(15.6430062215131,15.5080107655888,1.38580563032457));
#26652=CARTESIAN_POINT('Origin',(15.4374167911878,15.6296099418941,1.38577762513333));
#26653=CARTESIAN_POINT('Ctrl Pts',(17.0802317716411,15.5000000000002,11.1745050240672));
#26654=CARTESIAN_POINT('Ctrl Pts',(17.0802317716411,16.4123472387392,11.1328383574005));
#26655=CARTESIAN_POINT('Ctrl Pts',(16.2901158858204,16.8685208581088,11.0911716907338));
#26656=CARTESIAN_POINT('Ctrl Pts',(15.4999999999998,17.3246944774783,11.0495050240672));
#26657=CARTESIAN_POINT('Ctrl Pts',(14.7098841141792,16.8685208581088,11.0078383574005));
#26658=CARTESIAN_POINT('Ctrl Pts',(13.9197682283586,16.4123472387392,10.9661716907338));
#26659=CARTESIAN_POINT('Ctrl Pts',(13.9197682283586,15.5000000000001,10.9245050240672));
#26660=CARTESIAN_POINT('Ctrl Pts',(13.9197682283586,14.5876527612611,10.8828383574005));
#26661=CARTESIAN_POINT('Ctrl Pts',(14.7098841141792,14.1314791418916,10.8411716907338));
#26662=CARTESIAN_POINT('Ctrl Pts',(15.4999999999999,13.675305522522,10.7995050240672));
#26663=CARTESIAN_POINT('Ctrl Pts',(16.2901158858205,14.1314791418916,10.7578383574005));
#26664=CARTESIAN_POINT('Ctrl Pts',(17.0802317716411,14.5876527612611,10.7161716907338));
#26665=CARTESIAN_POINT('Ctrl Pts',(17.0802317716411,15.5000000000002,10.6745050240672));
#26666=CARTESIAN_POINT('Ctrl Pts',(17.0802317716411,16.4123472387392,10.6328383574005));
#26667=CARTESIAN_POINT('Ctrl Pts',(16.2901158858204,16.8685208581088,10.5911716907338));
#26668=CARTESIAN_POINT('Ctrl Pts',(15.4999999999998,17.3246944774783,10.5495050240672));
#26669=CARTESIAN_POINT('Ctrl Pts',(14.7098841141792,16.8685208581088,10.5078383574005));
#26670=CARTESIAN_POINT('Ctrl Pts',(13.9197682283586,16.4123472387392,10.4661716907338));
#26671=CARTESIAN_POINT('Ctrl Pts',(13.9197682283586,15.5000000000001,10.4245050240672));
#26672=CARTESIAN_POINT('Ctrl Pts',(13.9197682283586,14.5876527612611,10.3828383574005));
#26673=CARTESIAN_POINT('Ctrl Pts',(14.7098841141792,14.1314791418916,10.3411716907338));
#26674=CARTESIAN_POINT('Ctrl Pts',(15.4999999999999,13.675305522522,10.2995050240672));
#26675=CARTESIAN_POINT('Ctrl Pts',(16.2901158858205,14.1314791418916,10.2578383574005));
#26676=CARTESIAN_POINT('Ctrl Pts',(17.0802317716411,14.5876527612611,10.2161716907338));
#26677=CARTESIAN_POINT('Ctrl Pts',(17.0802317716411,15.5000000000002,10.1745050240672));
#26678=CARTESIAN_POINT('Ctrl Pts',(17.0802317716411,16.4123472387392,10.1328383574005));
#26679=CARTESIAN_POINT('Ctrl Pts',(16.2901158858204,16.8685208581088,10.0911716907338));
#26680=CARTESIAN_POINT('Ctrl Pts',(15.4999999999998,17.3246944774783,10.0495050240672));
#26681=CARTESIAN_POINT('Ctrl Pts',(14.7098841141792,16.8685208581088,10.0078383574005));
#26682=CARTESIAN_POINT('Ctrl Pts',(13.9197682283586,16.4123472387392,9.96617169073382));
#26683=CARTESIAN_POINT('Ctrl Pts',(13.9197682283586,15.5000000000001,9.92450502406715));
#26684=CARTESIAN_POINT('Ctrl Pts',(13.9197682283586,14.5876527612611,9.88283835740048));
#26685=CARTESIAN_POINT('Ctrl Pts',(14.7098841141792,14.1314791418916,9.84117169073382));
#26686=CARTESIAN_POINT('Ctrl Pts',(15.4999999999999,13.675305522522,9.79950502406715));
#26687=CARTESIAN_POINT('Ctrl Pts',(16.2901158858205,14.1314791418916,9.75783835740048));
#26688=CARTESIAN_POINT('Ctrl Pts',(17.0802317716411,14.5876527612611,9.71617169073381));
#26689=CARTESIAN_POINT('Ctrl Pts',(17.0802317716411,15.5000000000002,9.67450502406715));
#26690=CARTESIAN_POINT('Ctrl Pts',(17.0802317716411,16.4123472387392,9.63283835740048));
#26691=CARTESIAN_POINT('Ctrl Pts',(16.2901158858204,16.8685208581088,9.59117169073381));
#26692=CARTESIAN_POINT('Ctrl Pts',(15.4999999999998,17.3246944774783,9.54950502406714));
#26693=CARTESIAN_POINT('Ctrl Pts',(14.7098841141792,16.8685208581088,9.50783835740048));
#26694=CARTESIAN_POINT('Ctrl Pts',(13.9197682283586,16.4123472387392,9.46617169073381));
#26695=CARTESIAN_POINT('Ctrl Pts',(13.9197682283586,15.5000000000001,9.42450502406714));
#26696=CARTESIAN_POINT('Ctrl Pts',(13.9197682283586,14.5876527612611,9.38283835740048));
#26697=CARTESIAN_POINT('Ctrl Pts',(14.7098841141792,14.1314791418916,9.34117169073381));
#26698=CARTESIAN_POINT('Ctrl Pts',(15.4999999999999,13.675305522522,9.29950502406714));
#26699=CARTESIAN_POINT('Ctrl Pts',(16.2901158858205,14.1314791418916,9.25783835740048));
#26700=CARTESIAN_POINT('Ctrl Pts',(17.0802317716411,14.5876527612611,9.21617169073381));
#26701=CARTESIAN_POINT('Ctrl Pts',(17.0802317716411,15.5000000000002,9.17450502406714));
#26702=CARTESIAN_POINT('Ctrl Pts',(17.0802317716411,16.4123472387392,9.13283835740048));
#26703=CARTESIAN_POINT('Ctrl Pts',(16.2901158858204,16.8685208581088,9.09117169073381));
#26704=CARTESIAN_POINT('Ctrl Pts',(15.4999999999998,17.3246944774783,9.04950502406714));
#26705=CARTESIAN_POINT('Ctrl Pts',(14.7098841141792,16.8685208581088,9.00783835740047));
#26706=CARTESIAN_POINT('Ctrl Pts',(13.9197682283586,16.4123472387392,8.9661716907338));
#26707=CARTESIAN_POINT('Ctrl Pts',(13.9197682283586,15.5000000000001,8.92450502406714));
#26708=CARTESIAN_POINT('Ctrl Pts',(13.9197682283586,14.5876527612611,8.88283835740047));
#26709=CARTESIAN_POINT('Ctrl Pts',(14.7098841141792,14.1314791418916,8.8411716907338));
#26710=CARTESIAN_POINT('Ctrl Pts',(15.4999999999999,13.675305522522,8.79950502406713));
#26711=CARTESIAN_POINT('Ctrl Pts',(16.2901158858205,14.1314791418916,8.75783835740047));
#26712=CARTESIAN_POINT('Ctrl Pts',(17.0802317716411,14.5876527612611,8.7161716907338));
#26713=CARTESIAN_POINT('Ctrl Pts',(17.0802317716411,15.5000000000002,8.67450502406713));
#26714=CARTESIAN_POINT('Ctrl Pts',(17.0802317716411,16.4123472387392,8.63283835740047));
#26715=CARTESIAN_POINT('Ctrl Pts',(16.2901158858204,16.8685208581088,8.5911716907338));
#26716=CARTESIAN_POINT('Ctrl Pts',(15.4999999999998,17.3246944774783,8.54950502406713));
#26717=CARTESIAN_POINT('Ctrl Pts',(14.7098841141792,16.8685208581088,8.50783835740046));
#26718=CARTESIAN_POINT('Ctrl Pts',(13.9197682283586,16.4123472387392,8.4661716907338));
#26719=CARTESIAN_POINT('Ctrl Pts',(13.9197682283586,15.5000000000001,8.42450502406713));
#26720=CARTESIAN_POINT('Ctrl Pts',(13.9197682283586,14.5876527612611,8.38283835740046));
#26721=CARTESIAN_POINT('Ctrl Pts',(14.7098841141792,14.1314791418916,8.3411716907338));
#26722=CARTESIAN_POINT('Ctrl Pts',(15.4999999999999,13.675305522522,8.29950502406713));
#26723=CARTESIAN_POINT('Ctrl Pts',(16.2901158858205,14.1314791418916,8.25783835740046));
#26724=CARTESIAN_POINT('Ctrl Pts',(17.0802317716411,14.5876527612611,8.21617169073379));
#26725=CARTESIAN_POINT('Ctrl Pts',(17.0802317716411,15.5000000000002,8.17450502406713));
#26726=CARTESIAN_POINT('Ctrl Pts',(17.0802317716411,16.4123472387392,8.13283835740046));
#26727=CARTESIAN_POINT('Ctrl Pts',(16.2901158858204,16.8685208581088,8.09117169073379));
#26728=CARTESIAN_POINT('Ctrl Pts',(15.4999999999998,17.3246944774783,8.04950502406713));
#26729=CARTESIAN_POINT('Ctrl Pts',(14.7098841141792,16.8685208581088,8.00783835740046));
#26730=CARTESIAN_POINT('Ctrl Pts',(13.9197682283586,16.4123472387392,7.96617169073379));
#26731=CARTESIAN_POINT('Ctrl Pts',(13.9197682283586,15.5000000000001,7.92450502406712));
#26732=CARTESIAN_POINT('Ctrl Pts',(13.9197682283586,14.5876527612611,7.88283835740046));
#26733=CARTESIAN_POINT('Ctrl Pts',(14.7098841141792,14.1314791418916,7.84117169073379));
#26734=CARTESIAN_POINT('Ctrl Pts',(15.4999999999999,13.675305522522,7.79950502406712));
#26735=CARTESIAN_POINT('Ctrl Pts',(16.2901158858205,14.1314791418916,7.75783835740046));
#26736=CARTESIAN_POINT('Ctrl Pts',(17.0802317716411,14.5876527612611,7.71617169073379));
#26737=CARTESIAN_POINT('Ctrl Pts',(17.0802317716411,15.5000000000002,7.67450502406712));
#26738=CARTESIAN_POINT('Ctrl Pts',(17.0802317716411,16.4123472387392,7.63283835740045));
#26739=CARTESIAN_POINT('Ctrl Pts',(16.2901158858204,16.8685208581088,7.59117169073379));
#26740=CARTESIAN_POINT('Ctrl Pts',(15.4999999999998,17.3246944774783,7.54950502406712));
#26741=CARTESIAN_POINT('Ctrl Pts',(14.7098841141792,16.8685208581088,7.50783835740045));
#26742=CARTESIAN_POINT('Ctrl Pts',(13.9197682283586,16.4123472387392,7.46617169073379));
#26743=CARTESIAN_POINT('Ctrl Pts',(13.9197682283586,15.5000000000001,7.42450502406712));
#26744=CARTESIAN_POINT('Ctrl Pts',(13.9197682283586,14.5876527612611,7.38283835740045));
#26745=CARTESIAN_POINT('Ctrl Pts',(14.7098841141792,14.1314791418916,7.34117169073378));
#26746=CARTESIAN_POINT('Ctrl Pts',(15.4999999999999,13.675305522522,7.29950502406711));
#26747=CARTESIAN_POINT('Ctrl Pts',(16.2901158858205,14.1314791418916,7.25783835740045));
#26748=CARTESIAN_POINT('Ctrl Pts',(17.0802317716411,14.5876527612611,7.21617169073378));
#26749=CARTESIAN_POINT('Ctrl Pts',(17.0802317716411,15.5000000000002,7.17450502406711));
#26750=CARTESIAN_POINT('Ctrl Pts',(17.0802317716411,16.4123472387392,7.13283835740045));
#26751=CARTESIAN_POINT('Ctrl Pts',(16.2901158858204,16.8685208581088,7.09117169073378));
#26752=CARTESIAN_POINT('Ctrl Pts',(15.4999999999998,17.3246944774783,7.04950502406711));
#26753=CARTESIAN_POINT('Ctrl Pts',(14.7098841141792,16.8685208581088,7.00783835740045));
#26754=CARTESIAN_POINT('Ctrl Pts',(13.9197682283586,16.4123472387392,6.96617169073378));
#26755=CARTESIAN_POINT('Ctrl Pts',(13.9197682283586,15.5000000000001,6.92450502406711));
#26756=CARTESIAN_POINT('Ctrl Pts',(13.9197682283586,14.5876527612611,6.88283835740044));
#26757=CARTESIAN_POINT('Ctrl Pts',(14.7098841141792,14.1314791418916,6.84117169073378));
#26758=CARTESIAN_POINT('Ctrl Pts',(15.4999999999999,13.675305522522,6.79950502406711));
#26759=CARTESIAN_POINT('Ctrl Pts',(16.2901158858205,14.1314791418916,6.75783835740044));
#26760=CARTESIAN_POINT('Ctrl Pts',(17.0802317716411,14.5876527612611,6.71617169073377));
#26761=CARTESIAN_POINT('Ctrl Pts',(17.0802317716411,15.5000000000002,6.67450502406711));
#26762=CARTESIAN_POINT('Ctrl Pts',(17.0802317716411,16.4123472387392,6.63283835740044));
#26763=CARTESIAN_POINT('Ctrl Pts',(16.2901158858204,16.8685208581088,6.59117169073377));
#26764=CARTESIAN_POINT('Ctrl Pts',(15.4999999999998,17.3246944774783,6.54950502406711));
#26765=CARTESIAN_POINT('Ctrl Pts',(14.7098841141792,16.8685208581088,6.50783835740044));
#26766=CARTESIAN_POINT('Ctrl Pts',(13.9197682283586,16.4123472387392,6.46617169073377));
#26767=CARTESIAN_POINT('Ctrl Pts',(13.9197682283586,15.5000000000001,6.4245050240671));
#26768=CARTESIAN_POINT('Ctrl Pts',(13.9197682283586,14.5876527612611,6.38283835740044));
#26769=CARTESIAN_POINT('Ctrl Pts',(14.7098841141792,14.1314791418916,6.34117169073377));
#26770=CARTESIAN_POINT('Ctrl Pts',(15.4999999999999,13.675305522522,6.2995050240671));
#26771=CARTESIAN_POINT('Ctrl Pts',(16.2901158858205,14.1314791418916,6.25783835740044));
#26772=CARTESIAN_POINT('Ctrl Pts',(17.0802317716411,14.5876527612611,6.21617169073377));
#26773=CARTESIAN_POINT('Ctrl Pts',(17.0802317716411,15.5000000000002,6.1745050240671));
#26774=CARTESIAN_POINT('Ctrl Pts',(17.0802317716411,16.4123472387392,6.13283835740043));
#26775=CARTESIAN_POINT('Ctrl Pts',(16.2901158858204,16.8685208581088,6.09117169073377));
#26776=CARTESIAN_POINT('Ctrl Pts',(15.4999999999998,17.3246944774783,6.0495050240671));
#26777=CARTESIAN_POINT('Ctrl Pts',(14.7098841141792,16.8685208581088,6.00783835740043));
#26778=CARTESIAN_POINT('Ctrl Pts',(13.9197682283586,16.4123472387392,5.96617169073376));
#26779=CARTESIAN_POINT('Ctrl Pts',(13.9197682283586,15.5000000000001,5.9245050240671));
#26780=CARTESIAN_POINT('Ctrl Pts',(13.9197682283586,14.5876527612611,5.88283835740043));
#26781=CARTESIAN_POINT('Ctrl Pts',(14.7098841141792,14.1314791418916,5.84117169073376));
#26782=CARTESIAN_POINT('Ctrl Pts',(15.4999999999999,13.675305522522,5.79950502406709));
#26783=CARTESIAN_POINT('Ctrl Pts',(16.2901158858205,14.1314791418916,5.75783835740043));
#26784=CARTESIAN_POINT('Ctrl Pts',(17.0802317716411,14.5876527612611,5.71617169073376));
#26785=CARTESIAN_POINT('Ctrl Pts',(17.0802317716411,15.5000000000002,5.67450502406709));
#26786=CARTESIAN_POINT('Ctrl Pts',(17.0802317716411,16.4123472387392,5.63283835740043));
#26787=CARTESIAN_POINT('Ctrl Pts',(16.2901158858204,16.8685208581088,5.59117169073376));
#26788=CARTESIAN_POINT('Ctrl Pts',(15.4999999999998,17.3246944774783,5.54950502406709));
#26789=CARTESIAN_POINT('Ctrl Pts',(14.7098841141792,16.8685208581088,5.50783835740043));
#26790=CARTESIAN_POINT('Ctrl Pts',(13.9197682283586,16.4123472387392,5.46617169073376));
#26791=CARTESIAN_POINT('Ctrl Pts',(13.9197682283586,15.5000000000001,5.42450502406709));
#26792=CARTESIAN_POINT('Ctrl Pts',(13.9197682283586,14.5876527612611,5.38283835740042));
#26793=CARTESIAN_POINT('Ctrl Pts',(14.7098841141792,14.1314791418916,5.34117169073376));
#26794=CARTESIAN_POINT('Ctrl Pts',(15.4999999999999,13.675305522522,5.29950502406709));
#26795=CARTESIAN_POINT('Ctrl Pts',(16.2901158858205,14.1314791418916,5.25783835740042));
#26796=CARTESIAN_POINT('Ctrl Pts',(17.0802317716411,14.5876527612611,5.21617169073375));
#26797=CARTESIAN_POINT('Ctrl Pts',(17.0802317716411,15.5000000000002,5.17450502406709));
#26798=CARTESIAN_POINT('Ctrl Pts',(17.0802317716411,16.4123472387392,5.13283835740042));
#26799=CARTESIAN_POINT('Ctrl Pts',(16.2901158858204,16.8685208581088,5.09117169073375));
#26800=CARTESIAN_POINT('Ctrl Pts',(15.4999999999998,17.3246944774783,5.04950502406708));
#26801=CARTESIAN_POINT('Ctrl Pts',(14.7098841141792,16.8685208581088,5.00783835740042));
#26802=CARTESIAN_POINT('Ctrl Pts',(13.9197682283586,16.4123472387392,4.96617169073375));
#26803=CARTESIAN_POINT('Ctrl Pts',(13.9197682283586,15.5000000000001,4.92450502406708));
#26804=CARTESIAN_POINT('Ctrl Pts',(13.9197682283586,14.5876527612611,4.88283835740042));
#26805=CARTESIAN_POINT('Ctrl Pts',(14.7098841141792,14.1314791418916,4.84117169073375));
#26806=CARTESIAN_POINT('Ctrl Pts',(15.4999999999999,13.675305522522,4.79950502406708));
#26807=CARTESIAN_POINT('Ctrl Pts',(16.2901158858205,14.1314791418916,4.75783835740041));
#26808=CARTESIAN_POINT('Ctrl Pts',(17.0802317716411,14.5876527612611,4.71617169073375));
#26809=CARTESIAN_POINT('Ctrl Pts',(17.0802317716411,15.5000000000002,4.67450502406708));
#26810=CARTESIAN_POINT('Ctrl Pts',(17.0802317716411,16.4123472387392,4.63283835740041));
#26811=CARTESIAN_POINT('Ctrl Pts',(16.2901158858204,16.8685208581088,4.59117169073375));
#26812=CARTESIAN_POINT('Ctrl Pts',(15.4999999999998,17.3246944774783,4.54950502406708));
#26813=CARTESIAN_POINT('Ctrl Pts',(14.7098841141792,16.8685208581088,4.50783835740041));
#26814=CARTESIAN_POINT('Ctrl Pts',(13.9197682283586,16.4123472387392,4.46617169073374));
#26815=CARTESIAN_POINT('Ctrl Pts',(13.9197682283586,15.5000000000001,4.42450502406708));
#26816=CARTESIAN_POINT('Ctrl Pts',(13.9197682283586,14.5876527612611,4.38283835740041));
#26817=CARTESIAN_POINT('Ctrl Pts',(14.7098841141792,14.1314791418916,4.34117169073374));
#26818=CARTESIAN_POINT('Ctrl Pts',(15.4999999999999,13.675305522522,4.29950502406708));
#26819=CARTESIAN_POINT('Ctrl Pts',(16.2901158858205,14.1314791418916,4.25783835740041));
#26820=CARTESIAN_POINT('Ctrl Pts',(17.0802317716411,14.5876527612611,4.21617169073374));
#26821=CARTESIAN_POINT('Ctrl Pts',(17.0802317716411,15.5000000000002,4.17450502406707));
#26822=CARTESIAN_POINT('Ctrl Pts',(17.0802317716411,16.4123472387392,4.13283835740041));
#26823=CARTESIAN_POINT('Ctrl Pts',(16.2901158858204,16.8685208581088,4.09117169073374));
#26824=CARTESIAN_POINT('Ctrl Pts',(15.4999999999998,17.3246944774783,4.04950502406707));
#26825=CARTESIAN_POINT('Ctrl Pts',(14.7098841141792,16.8685208581088,4.0078383574004));
#26826=CARTESIAN_POINT('Ctrl Pts',(13.9197682283586,16.4123472387392,3.96617169073374));
#26827=CARTESIAN_POINT('Ctrl Pts',(13.9197682283586,15.5000000000001,3.92450502406707));
#26828=CARTESIAN_POINT('Ctrl Pts',(13.9197682283586,14.5876527612611,3.8828383574004));
#26829=CARTESIAN_POINT('Ctrl Pts',(14.7098841141792,14.1314791418916,3.84117169073374));
#26830=CARTESIAN_POINT('Ctrl Pts',(15.4999999999999,13.675305522522,3.79950502406707));
#26831=CARTESIAN_POINT('Ctrl Pts',(16.2901158858205,14.1314791418916,3.7578383574004));
#26832=CARTESIAN_POINT('Ctrl Pts',(17.0802317716411,14.5876527612611,3.71617169073373));
#26833=CARTESIAN_POINT('Ctrl Pts',(17.0802317716411,15.5000000000002,3.67450502406707));
#26834=CARTESIAN_POINT('Ctrl Pts',(17.0802317716411,16.4123472387392,3.6328383574004));
#26835=CARTESIAN_POINT('Ctrl Pts',(16.2901158858204,16.8685208581088,3.59117169073373));
#26836=CARTESIAN_POINT('Ctrl Pts',(15.4999999999998,17.3246944774783,3.54950502406707));
#26837=CARTESIAN_POINT('Ctrl Pts',(14.7098841141792,16.8685208581088,3.5078383574004));
#26838=CARTESIAN_POINT('Ctrl Pts',(13.9197682283586,16.4123472387392,3.46617169073373));
#26839=CARTESIAN_POINT('Ctrl Pts',(13.9197682283586,15.5000000000001,3.42450502406706));
#26840=CARTESIAN_POINT('Ctrl Pts',(13.9197682283586,14.5876527612611,3.3828383574004));
#26841=CARTESIAN_POINT('Ctrl Pts',(14.7098841141792,14.1314791418916,3.34117169073373));
#26842=CARTESIAN_POINT('Ctrl Pts',(15.4999999999999,13.675305522522,3.29950502406706));
#26843=CARTESIAN_POINT('Ctrl Pts',(16.2901158858205,14.1314791418916,3.2578383574004));
#26844=CARTESIAN_POINT('Ctrl Pts',(17.0802317716411,14.5876527612611,3.21617169073373));
#26845=CARTESIAN_POINT('Ctrl Pts',(17.0802317716411,15.5000000000002,3.17450502406706));
#26846=CARTESIAN_POINT('Ctrl Pts',(17.0802317716411,16.4123472387392,3.13283835740039));
#26847=CARTESIAN_POINT('Ctrl Pts',(16.2901158858204,16.8685208581088,3.09117169073373));
#26848=CARTESIAN_POINT('Ctrl Pts',(15.4999999999998,17.3246944774783,3.04950502406706));
#26849=CARTESIAN_POINT('Ctrl Pts',(14.7098841141792,16.8685208581088,3.00783835740039));
#26850=CARTESIAN_POINT('Ctrl Pts',(13.9197682283586,16.4123472387392,2.96617169073372));
#26851=CARTESIAN_POINT('Ctrl Pts',(13.9197682283586,15.5000000000001,2.92450502406706));
#26852=CARTESIAN_POINT('Ctrl Pts',(13.9197682283586,14.5876527612611,2.88283835740039));
#26853=CARTESIAN_POINT('Ctrl Pts',(14.7098841141792,14.1314791418916,2.84117169073372));
#26854=CARTESIAN_POINT('Ctrl Pts',(15.4999999999999,13.675305522522,2.79950502406705));
#26855=CARTESIAN_POINT('Ctrl Pts',(16.2901158858205,14.1314791418916,2.75783835740039));
#26856=CARTESIAN_POINT('Ctrl Pts',(17.0802317716411,14.5876527612611,2.71617169073372));
#26857=CARTESIAN_POINT('Ctrl Pts',(17.0802317716411,15.5000000000002,2.67450502406705));
#26858=CARTESIAN_POINT('Ctrl Pts',(17.0802317716411,16.4123472387392,2.63283835740039));
#26859=CARTESIAN_POINT('Ctrl Pts',(16.2901158858204,16.8685208581088,2.59117169073372));
#26860=CARTESIAN_POINT('Ctrl Pts',(15.4999999999998,17.3246944774783,2.54950502406705));
#26861=CARTESIAN_POINT('Ctrl Pts',(14.7098841141792,16.8685208581088,2.50783835740038));
#26862=CARTESIAN_POINT('Ctrl Pts',(13.9197682283586,16.4123472387392,2.46617169073372));
#26863=CARTESIAN_POINT('Ctrl Pts',(13.9197682283586,15.5000000000001,2.42450502406705));
#26864=CARTESIAN_POINT('Ctrl Pts',(13.9197682283586,14.5876527612611,2.38283835740038));
#26865=CARTESIAN_POINT('Ctrl Pts',(14.7098841141792,14.1314791418916,2.34117169073372));
#26866=CARTESIAN_POINT('Ctrl Pts',(15.4999999999999,13.675305522522,2.29950502406705));
#26867=CARTESIAN_POINT('Ctrl Pts',(16.2901158858205,14.1314791418916,2.25783835740038));
#26868=CARTESIAN_POINT('Ctrl Pts',(17.0802317716411,14.5876527612611,2.21617169073371));
#26869=CARTESIAN_POINT('Ctrl Pts',(17.0802317716411,15.5000000000002,2.17450502406705));
#26870=CARTESIAN_POINT('Ctrl Pts',(17.0802317716411,16.4123472387392,2.13283835740038));
#26871=CARTESIAN_POINT('Ctrl Pts',(16.2901158858204,16.8685208581088,2.09117169073371));
#26872=CARTESIAN_POINT('Ctrl Pts',(15.4999999999998,17.3246944774783,2.04950502406705));
#26873=CARTESIAN_POINT('Ctrl Pts',(14.7098841141792,16.8685208581088,2.00783835740038));
#26874=CARTESIAN_POINT('Ctrl Pts',(13.9197682283586,16.4123472387392,1.96617169073371));
#26875=CARTESIAN_POINT('Ctrl Pts',(13.9197682283586,15.5000000000001,1.92450502406704));
#26876=CARTESIAN_POINT('Ctrl Pts',(13.9197682283586,14.5876527612611,1.88283835740038));
#26877=CARTESIAN_POINT('Ctrl Pts',(14.7098841141792,14.1314791418916,1.84117169073371));
#26878=CARTESIAN_POINT('Ctrl Pts',(15.4999999999999,13.675305522522,1.79950502406704));
#26879=CARTESIAN_POINT('Ctrl Pts',(16.2901158858205,14.1314791418916,1.75783835740037));
#26880=CARTESIAN_POINT('Ctrl Pts',(17.0802317716411,14.5876527612611,1.71617169073371));
#26881=CARTESIAN_POINT('Ctrl Pts',(17.0802317716411,15.5000000000002,1.67450502406704));
#26882=CARTESIAN_POINT('Ctrl Pts',(17.0802317716411,16.4123472387392,1.63283835740037));
#26883=CARTESIAN_POINT('Ctrl Pts',(16.2901158858204,16.8685208581088,1.59117169073371));
#26884=CARTESIAN_POINT('Ctrl Pts',(15.4999999999998,17.3246944774783,1.54950502406704));
#26885=CARTESIAN_POINT('Ctrl Pts',(14.7098841141792,16.8685208581088,1.50783835740037));
#26886=CARTESIAN_POINT('Ctrl Pts',(13.9197682283586,16.4123472387392,1.4661716907337));
#26887=CARTESIAN_POINT('Ctrl Pts',(13.9197682283586,15.5000000000001,1.42450502406704));
#26888=CARTESIAN_POINT('Ctrl Pts',(13.9197682283586,14.5876527612611,1.38283835740037));
#26889=CARTESIAN_POINT('Ctrl Pts',(14.7098841141792,14.1314791418916,1.3411716907337));
#26890=CARTESIAN_POINT('Ctrl Pts',(15.4999999999999,13.675305522522,1.29950502406703));
#26891=CARTESIAN_POINT('Ctrl Pts',(16.2901158858205,14.1314791418916,1.25783835740037));
#26892=CARTESIAN_POINT('Ctrl Pts',(17.0802317716411,14.5876527612611,1.2161716907337));
#26893=CARTESIAN_POINT('Ctrl Pts',(17.0802317716411,15.5000000000002,1.17450502406703));
#26894=CARTESIAN_POINT('Ctrl Pts',(17.0802317716411,16.4123472387392,1.13283835740037));
#26895=CARTESIAN_POINT('Ctrl Pts',(16.2901158858204,16.8685208581088,1.0911716907337));
#26896=CARTESIAN_POINT('Ctrl Pts',(15.4999999999998,17.3246944774783,1.04950502406703));
#26897=CARTESIAN_POINT('Ctrl Pts',(14.7098841141792,16.8685208581088,1.00783835740037));
#26898=CARTESIAN_POINT('Ctrl Pts',(13.9197682283586,16.4123472387392,0.966171690733698));
#26899=CARTESIAN_POINT('Ctrl Pts',(13.9197682283586,15.5000000000001,0.924505024067031));
#26900=CARTESIAN_POINT('Ctrl Pts',(13.9197682283586,14.5876527612611,0.882838357400363));
#26901=CARTESIAN_POINT('Ctrl Pts',(14.7098841141792,14.1314791418916,0.841171690733696));
#26902=CARTESIAN_POINT('Ctrl Pts',(15.4999999999999,13.675305522522,0.799505024067029));
#26903=CARTESIAN_POINT('Ctrl Pts',(16.2901158858205,14.1314791418916,0.757838357400362));
#26904=CARTESIAN_POINT('Ctrl Pts',(17.0802317716411,14.5876527612611,0.716171690733694));
#26905=CARTESIAN_POINT('Ctrl Pts',(17.0802317716411,15.5000000000002,0.674505024067027));
#26906=CARTESIAN_POINT('Ctrl Pts',(17.0802317716411,16.4123472387392,0.632838357400359));
#26907=CARTESIAN_POINT('Ctrl Pts',(16.2901158858204,16.8685208581088,0.591171690733692));
#26908=CARTESIAN_POINT('Ctrl Pts',(15.4999999999998,17.3246944774783,0.549505024067025));
#26909=CARTESIAN_POINT('Ctrl Pts',(14.7098841141792,16.8685208581088,0.507838357400358));
#26910=CARTESIAN_POINT('Ctrl Pts',(13.9197682283586,16.4123472387392,0.46617169073369));
#26911=CARTESIAN_POINT('Ctrl Pts',(13.9197682283586,15.5000000000001,0.424505024067023));
#26912=CARTESIAN_POINT('Ctrl Pts',(13.9197682283586,14.5876527612611,0.382838357400356));
#26913=CARTESIAN_POINT('Ctrl Pts',(14.7098841141792,14.1314791418916,0.341171690733689));
#26914=CARTESIAN_POINT('Ctrl Pts',(15.4999999999999,13.675305522522,0.299505024067021));
#26915=CARTESIAN_POINT('Ctrl Pts',(16.2901158858205,14.1314791418916,0.257838357400354));
#26916=CARTESIAN_POINT('Ctrl Pts',(17.0802317716411,14.5876527612611,0.216171690733687));
#26917=CARTESIAN_POINT('Ctrl Pts',(17.0802317716411,15.5000000000002,0.174505024067019));
#26918=CARTESIAN_POINT('Ctrl Pts',(17.0802317716411,16.4123472387392,0.132838357400352));
#26919=CARTESIAN_POINT('Ctrl Pts',(16.2901158858204,16.8685208581088,0.0911716907336848));
#26920=CARTESIAN_POINT('Ctrl Pts',(15.4999999999998,17.3246944774783,0.0495050240670175));
#26921=CARTESIAN_POINT('Ctrl Pts',(14.7098841141792,16.8685208581088,0.00783835740035027));
#26922=CARTESIAN_POINT('Ctrl Pts',(13.9197682283586,16.4123472387392,-0.033828309266317));
#26923=CARTESIAN_POINT('Ctrl Pts',(13.9197682283586,15.5000000000001,-0.0754949759329843));
#26924=CARTESIAN_POINT('Ctrl Pts',(13.9197682283586,14.5876527612611,-0.11716164259965));
#26925=CARTESIAN_POINT('Ctrl Pts',(14.7098841141792,14.1314791418916,-0.158828309266317));
#26926=CARTESIAN_POINT('Ctrl Pts',(15.4999999999999,13.675305522522,-0.200494975932984));
#26927=CARTESIAN_POINT('Ctrl Pts',(16.2901158858205,14.1314791418916,-0.242161642599652));
#26928=CARTESIAN_POINT('Ctrl Pts',(17.0802317716411,14.5876527612611,-0.283828309266319));
#26929=CARTESIAN_POINT('Ctrl Pts',(17.0802317716411,15.5000000000002,-0.325494975932986));
#26930=CARTESIAN_POINT('Ctrl Pts',(17.0802317716411,16.4123472387392,-0.367161642599654));
#26931=CARTESIAN_POINT('Ctrl Pts',(16.2901158858204,16.8685208581088,-0.408828309266321));
#26932=CARTESIAN_POINT('Ctrl Pts',(15.4999999999998,17.3246944774783,-0.450494975932988));
#26933=CARTESIAN_POINT('Ctrl Pts',(14.7098841141792,16.8685208581088,-0.492161642599655));
#26934=CARTESIAN_POINT('Ctrl Pts',(13.9197682283586,16.4123472387392,-0.533828309266323));
#26935=CARTESIAN_POINT('Ctrl Pts',(13.9197682283586,15.5000000000001,-0.57549497593299));
#26936=CARTESIAN_POINT('Ctrl Pts',(13.9197682283586,14.5876527612611,-0.617161642599657));
#26937=CARTESIAN_POINT('Ctrl Pts',(14.7098841141792,14.1314791418916,-0.658828309266325));
#26938=CARTESIAN_POINT('Ctrl Pts',(15.4999999999999,13.675305522522,-0.700494975932992));
#26939=CARTESIAN_POINT('Ctrl Pts',(16.2901158858205,14.1314791418916,-0.742161642599659));
#26940=CARTESIAN_POINT('Ctrl Pts',(17.0802317716411,14.5876527612611,-0.783828309266326));
#26941=CARTESIAN_POINT('Ctrl Pts',(17.0802317716411,15.5000000000002,-0.825494975932994));
#26942=CARTESIAN_POINT('Ctrl Pts',(17.0802317716411,16.4123472387392,-0.867161642599661));
#26943=CARTESIAN_POINT('Ctrl Pts',(16.2901158858204,16.8685208581088,-0.908828309266328));
#26944=CARTESIAN_POINT('Ctrl Pts',(15.4999999999998,17.3246944774783,-0.950494975932996));
#26945=CARTESIAN_POINT('Ctrl Pts',(14.7098841141792,16.8685208581088,-0.992161642599663));
#26946=CARTESIAN_POINT('Ctrl Pts',(13.9197682283586,16.4123472387392,-1.03382830926633));
#26947=CARTESIAN_POINT('Ctrl Pts',(13.9197682283586,15.5000000000001,-1.075494975933));
#26948=CARTESIAN_POINT('Ctrl Pts',(13.9197682283586,14.5876527612611,-1.11716164259966));
#26949=CARTESIAN_POINT('Ctrl Pts',(14.7098841141792,14.1314791418916,-1.15882830926633));
#26950=CARTESIAN_POINT('Ctrl Pts',(15.4999999999999,13.675305522522,-1.200494975933));
#26951=CARTESIAN_POINT('Ctrl Pts',(16.2901158858205,14.1314791418916,-1.24216164259967));
#26952=CARTESIAN_POINT('Ctrl Pts',(17.0802317716411,14.5876527612611,-1.28382830926633));
#26953=CARTESIAN_POINT('Ctrl Pts',(17.0802317716411,15.5000000000002,-1.325494975933));
#26954=CARTESIAN_POINT('Ctrl Pts',(17.0802317716411,16.4123472387392,-1.36716164259967));
#26955=CARTESIAN_POINT('Ctrl Pts',(16.2901158858204,16.8685208581088,-1.40882830926633));
#26956=CARTESIAN_POINT('Ctrl Pts',(15.4999999999998,17.3246944774783,-1.450494975933));
#26957=CARTESIAN_POINT('Ctrl Pts',(14.7098841141792,16.8685208581088,-1.49216164259967));
#26958=CARTESIAN_POINT('Ctrl Pts',(13.9197682283586,16.4123472387392,-1.53382830926634));
#26959=CARTESIAN_POINT('Ctrl Pts',(13.9197682283586,15.5000000000001,-1.575494975933));
#26960=CARTESIAN_POINT('Ctrl Pts',(13.9197682283586,14.5876527612611,-1.61716164259967));
#26961=CARTESIAN_POINT('Ctrl Pts',(14.7098841141792,14.1314791418916,-1.65882830926634));
#26962=CARTESIAN_POINT('Ctrl Pts',(15.4999999999999,13.675305522522,-1.70049497593301));
#26963=CARTESIAN_POINT('Ctrl Pts',(16.2901158858205,14.1314791418916,-1.74216164259967));
#26964=CARTESIAN_POINT('Ctrl Pts',(17.0802317716411,14.5876527612611,-1.78382830926634));
#26965=CARTESIAN_POINT('Ctrl Pts',(17.0802317716411,15.5000000000002,-1.82549497593301));
#26966=CARTESIAN_POINT('Ctrl Pts',(17.0802317716411,16.4123472387392,-1.86716164259967));
#26967=CARTESIAN_POINT('Ctrl Pts',(16.2901158858204,16.8685208581088,-1.90882830926634));
#26968=CARTESIAN_POINT('Ctrl Pts',(15.4999999999998,17.3246944774783,-1.95049497593301));
#26969=CARTESIAN_POINT('Ctrl Pts',(14.7098841141792,16.8685208581088,-1.99216164259968));
#26970=CARTESIAN_POINT('Ctrl Pts',(14.4189893226642,16.7005726719217,-2.00750194461187));
#26971=CARTESIAN_POINT('Ctrl Pts',(14.221556935765,16.4288249477779,-2.02511838079831));
#26972=CARTESIAN_POINT('Ctrl Pts',(17.4320632938681,15.5000000000002,10.971375));
#26973=CARTESIAN_POINT('Ctrl Pts',(17.4320632938681,16.6154772628064,10.9297083333333));
#26974=CARTESIAN_POINT('Ctrl Pts',(16.466031646934,17.1732158942095,10.8880416666667));
#26975=CARTESIAN_POINT('Ctrl Pts',(15.4999999999998,17.7309545256126,10.846375));
#26976=CARTESIAN_POINT('Ctrl Pts',(14.5339683530657,17.1732158942095,10.8047083333333));
#26977=CARTESIAN_POINT('Ctrl Pts',(13.5679367061316,16.6154772628064,10.7630416666667));
#26978=CARTESIAN_POINT('Ctrl Pts',(13.5679367061316,15.5000000000001,10.721375));
#26979=CARTESIAN_POINT('Ctrl Pts',(13.5679367061316,14.3845227371939,10.6797083333333));
#26980=CARTESIAN_POINT('Ctrl Pts',(14.5339683530657,13.8267841057908,10.6380416666667));
#26981=CARTESIAN_POINT('Ctrl Pts',(15.4999999999999,13.2690454743877,10.596375));
#26982=CARTESIAN_POINT('Ctrl Pts',(16.466031646934,13.8267841057908,10.5547083333333));
#26983=CARTESIAN_POINT('Ctrl Pts',(17.4320632938681,14.3845227371939,10.5130416666667));
#26984=CARTESIAN_POINT('Ctrl Pts',(17.4320632938681,15.5000000000002,10.471375));
#26985=CARTESIAN_POINT('Ctrl Pts',(17.4320632938681,16.6154772628064,10.4297083333333));
#26986=CARTESIAN_POINT('Ctrl Pts',(16.466031646934,17.1732158942095,10.3880416666667));
#26987=CARTESIAN_POINT('Ctrl Pts',(15.4999999999998,17.7309545256126,10.346375));
#26988=CARTESIAN_POINT('Ctrl Pts',(14.5339683530657,17.1732158942095,10.3047083333333));
#26989=CARTESIAN_POINT('Ctrl Pts',(13.5679367061316,16.6154772628064,10.2630416666667));
#26990=CARTESIAN_POINT('Ctrl Pts',(13.5679367061316,15.5000000000001,10.221375));
#26991=CARTESIAN_POINT('Ctrl Pts',(13.5679367061316,14.3845227371939,10.1797083333333));
#26992=CARTESIAN_POINT('Ctrl Pts',(14.5339683530657,13.8267841057908,10.1380416666667));
#26993=CARTESIAN_POINT('Ctrl Pts',(15.4999999999999,13.2690454743877,10.096375));
#26994=CARTESIAN_POINT('Ctrl Pts',(16.466031646934,13.8267841057908,10.0547083333333));
#26995=CARTESIAN_POINT('Ctrl Pts',(17.4320632938681,14.3845227371939,10.0130416666666));
#26996=CARTESIAN_POINT('Ctrl Pts',(17.4320632938681,15.5000000000002,9.97137499999998));
#26997=CARTESIAN_POINT('Ctrl Pts',(17.4320632938681,16.6154772628064,9.92970833333332));
#26998=CARTESIAN_POINT('Ctrl Pts',(16.466031646934,17.1732158942095,9.88804166666665));
#26999=CARTESIAN_POINT('Ctrl Pts',(15.4999999999998,17.7309545256126,9.84637499999998));
#27000=CARTESIAN_POINT('Ctrl Pts',(14.5339683530657,17.1732158942095,9.80470833333331));
#27001=CARTESIAN_POINT('Ctrl Pts',(13.5679367061316,16.6154772628064,9.76304166666665));
#27002=CARTESIAN_POINT('Ctrl Pts',(13.5679367061316,15.5000000000001,9.72137499999998));
#27003=CARTESIAN_POINT('Ctrl Pts',(13.5679367061316,14.3845227371939,9.67970833333331));
#27004=CARTESIAN_POINT('Ctrl Pts',(14.5339683530657,13.8267841057908,9.63804166666664));
#27005=CARTESIAN_POINT('Ctrl Pts',(15.4999999999999,13.2690454743877,9.59637499999998));
#27006=CARTESIAN_POINT('Ctrl Pts',(16.466031646934,13.8267841057908,9.55470833333331));
#27007=CARTESIAN_POINT('Ctrl Pts',(17.4320632938681,14.3845227371939,9.51304166666664));
#27008=CARTESIAN_POINT('Ctrl Pts',(17.4320632938681,15.5000000000002,9.47137499999998));
#27009=CARTESIAN_POINT('Ctrl Pts',(17.4320632938681,16.6154772628064,9.42970833333331));
#27010=CARTESIAN_POINT('Ctrl Pts',(16.466031646934,17.1732158942095,9.38804166666664));
#27011=CARTESIAN_POINT('Ctrl Pts',(15.4999999999998,17.7309545256126,9.34637499999997));
#27012=CARTESIAN_POINT('Ctrl Pts',(14.5339683530657,17.1732158942095,9.30470833333331));
#27013=CARTESIAN_POINT('Ctrl Pts',(13.5679367061316,16.6154772628064,9.26304166666664));
#27014=CARTESIAN_POINT('Ctrl Pts',(13.5679367061316,15.5000000000001,9.22137499999997));
#27015=CARTESIAN_POINT('Ctrl Pts',(13.5679367061316,14.3845227371939,9.1797083333333));
#27016=CARTESIAN_POINT('Ctrl Pts',(14.5339683530657,13.8267841057908,9.13804166666664));
#27017=CARTESIAN_POINT('Ctrl Pts',(15.4999999999999,13.2690454743877,9.09637499999997));
#27018=CARTESIAN_POINT('Ctrl Pts',(16.466031646934,13.8267841057908,9.0547083333333));
#27019=CARTESIAN_POINT('Ctrl Pts',(17.4320632938681,14.3845227371939,9.01304166666664));
#27020=CARTESIAN_POINT('Ctrl Pts',(17.4320632938681,15.5000000000002,8.97137499999997));
#27021=CARTESIAN_POINT('Ctrl Pts',(17.4320632938681,16.6154772628064,8.9297083333333));
#27022=CARTESIAN_POINT('Ctrl Pts',(16.466031646934,17.1732158942095,8.88804166666663));
#27023=CARTESIAN_POINT('Ctrl Pts',(15.4999999999998,17.7309545256126,8.84637499999997));
#27024=CARTESIAN_POINT('Ctrl Pts',(14.5339683530657,17.1732158942095,8.8047083333333));
#27025=CARTESIAN_POINT('Ctrl Pts',(13.5679367061316,16.6154772628064,8.76304166666663));
#27026=CARTESIAN_POINT('Ctrl Pts',(13.5679367061316,15.5000000000001,8.72137499999997));
#27027=CARTESIAN_POINT('Ctrl Pts',(13.5679367061316,14.3845227371939,8.6797083333333));
#27028=CARTESIAN_POINT('Ctrl Pts',(14.5339683530657,13.8267841057908,8.63804166666663));
#27029=CARTESIAN_POINT('Ctrl Pts',(15.4999999999999,13.2690454743877,8.59637499999996));
#27030=CARTESIAN_POINT('Ctrl Pts',(16.466031646934,13.8267841057908,8.5547083333333));
#27031=CARTESIAN_POINT('Ctrl Pts',(17.4320632938681,14.3845227371939,8.51304166666663));
#27032=CARTESIAN_POINT('Ctrl Pts',(17.4320632938681,15.5000000000002,8.47137499999996));
#27033=CARTESIAN_POINT('Ctrl Pts',(17.4320632938681,16.6154772628064,8.42970833333329));
#27034=CARTESIAN_POINT('Ctrl Pts',(16.466031646934,17.1732158942095,8.38804166666663));
#27035=CARTESIAN_POINT('Ctrl Pts',(15.4999999999998,17.7309545256126,8.34637499999996));
#27036=CARTESIAN_POINT('Ctrl Pts',(14.5339683530657,17.1732158942095,8.30470833333329));
#27037=CARTESIAN_POINT('Ctrl Pts',(13.5679367061316,16.6154772628064,8.26304166666663));
#27038=CARTESIAN_POINT('Ctrl Pts',(13.5679367061316,15.5000000000001,8.22137499999996));
#27039=CARTESIAN_POINT('Ctrl Pts',(13.5679367061316,14.3845227371939,8.17970833333329));
#27040=CARTESIAN_POINT('Ctrl Pts',(14.5339683530657,13.8267841057908,8.13804166666662));
#27041=CARTESIAN_POINT('Ctrl Pts',(15.4999999999999,13.2690454743877,8.09637499999996));
#27042=CARTESIAN_POINT('Ctrl Pts',(16.466031646934,13.8267841057908,8.05470833333329));
#27043=CARTESIAN_POINT('Ctrl Pts',(17.4320632938681,14.3845227371939,8.01304166666662));
#27044=CARTESIAN_POINT('Ctrl Pts',(17.4320632938681,15.5000000000002,7.97137499999995));
#27045=CARTESIAN_POINT('Ctrl Pts',(17.4320632938681,16.6154772628064,7.92970833333329));
#27046=CARTESIAN_POINT('Ctrl Pts',(16.466031646934,17.1732158942095,7.88804166666662));
#27047=CARTESIAN_POINT('Ctrl Pts',(15.4999999999998,17.7309545256126,7.84637499999995));
#27048=CARTESIAN_POINT('Ctrl Pts',(14.5339683530657,17.1732158942095,7.80470833333329));
#27049=CARTESIAN_POINT('Ctrl Pts',(13.5679367061316,16.6154772628064,7.76304166666662));
#27050=CARTESIAN_POINT('Ctrl Pts',(13.5679367061316,15.5000000000001,7.72137499999995));
#27051=CARTESIAN_POINT('Ctrl Pts',(13.5679367061316,14.3845227371939,7.67970833333329));
#27052=CARTESIAN_POINT('Ctrl Pts',(14.5339683530657,13.8267841057908,7.63804166666662));
#27053=CARTESIAN_POINT('Ctrl Pts',(15.4999999999999,13.2690454743877,7.59637499999995));
#27054=CARTESIAN_POINT('Ctrl Pts',(16.466031646934,13.8267841057908,7.55470833333328));
#27055=CARTESIAN_POINT('Ctrl Pts',(17.4320632938681,14.3845227371939,7.51304166666662));
#27056=CARTESIAN_POINT('Ctrl Pts',(17.4320632938681,15.5000000000002,7.47137499999995));
#27057=CARTESIAN_POINT('Ctrl Pts',(17.4320632938681,16.6154772628064,7.42970833333328));
#27058=CARTESIAN_POINT('Ctrl Pts',(16.466031646934,17.1732158942095,7.38804166666661));
#27059=CARTESIAN_POINT('Ctrl Pts',(15.4999999999998,17.7309545256126,7.34637499999995));
#27060=CARTESIAN_POINT('Ctrl Pts',(14.5339683530657,17.1732158942095,7.30470833333328));
#27061=CARTESIAN_POINT('Ctrl Pts',(13.5679367061316,16.6154772628064,7.26304166666661));
#27062=CARTESIAN_POINT('Ctrl Pts',(13.5679367061316,15.5000000000001,7.22137499999994));
#27063=CARTESIAN_POINT('Ctrl Pts',(13.5679367061316,14.3845227371939,7.17970833333328));
#27064=CARTESIAN_POINT('Ctrl Pts',(14.5339683530657,13.8267841057908,7.13804166666661));
#27065=CARTESIAN_POINT('Ctrl Pts',(15.4999999999999,13.2690454743877,7.09637499999995));
#27066=CARTESIAN_POINT('Ctrl Pts',(16.466031646934,13.8267841057908,7.05470833333328));
#27067=CARTESIAN_POINT('Ctrl Pts',(17.4320632938681,14.3845227371939,7.01304166666661));
#27068=CARTESIAN_POINT('Ctrl Pts',(17.4320632938681,15.5000000000002,6.97137499999994));
#27069=CARTESIAN_POINT('Ctrl Pts',(17.4320632938681,16.6154772628064,6.92970833333328));
#27070=CARTESIAN_POINT('Ctrl Pts',(16.466031646934,17.1732158942095,6.88804166666661));
#27071=CARTESIAN_POINT('Ctrl Pts',(15.4999999999998,17.7309545256126,6.84637499999994));
#27072=CARTESIAN_POINT('Ctrl Pts',(14.5339683530657,17.1732158942095,6.80470833333327));
#27073=CARTESIAN_POINT('Ctrl Pts',(13.5679367061316,16.6154772628064,6.76304166666661));
#27074=CARTESIAN_POINT('Ctrl Pts',(13.5679367061316,15.5000000000001,6.72137499999994));
#27075=CARTESIAN_POINT('Ctrl Pts',(13.5679367061316,14.3845227371939,6.67970833333327));
#27076=CARTESIAN_POINT('Ctrl Pts',(14.5339683530657,13.8267841057908,6.6380416666666));
#27077=CARTESIAN_POINT('Ctrl Pts',(15.4999999999999,13.2690454743877,6.59637499999994));
#27078=CARTESIAN_POINT('Ctrl Pts',(16.466031646934,13.8267841057908,6.55470833333327));
#27079=CARTESIAN_POINT('Ctrl Pts',(17.4320632938681,14.3845227371939,6.5130416666666));
#27080=CARTESIAN_POINT('Ctrl Pts',(17.4320632938681,15.5000000000002,6.47137499999994));
#27081=CARTESIAN_POINT('Ctrl Pts',(17.4320632938681,16.6154772628064,6.42970833333327));
#27082=CARTESIAN_POINT('Ctrl Pts',(16.466031646934,17.1732158942095,6.3880416666666));
#27083=CARTESIAN_POINT('Ctrl Pts',(15.4999999999998,17.7309545256126,6.34637499999993));
#27084=CARTESIAN_POINT('Ctrl Pts',(14.5339683530657,17.1732158942095,6.30470833333327));
#27085=CARTESIAN_POINT('Ctrl Pts',(13.5679367061316,16.6154772628064,6.2630416666666));
#27086=CARTESIAN_POINT('Ctrl Pts',(13.5679367061316,15.5000000000001,6.22137499999993));
#27087=CARTESIAN_POINT('Ctrl Pts',(13.5679367061316,14.3845227371939,6.17970833333327));
#27088=CARTESIAN_POINT('Ctrl Pts',(14.5339683530657,13.8267841057908,6.1380416666666));
#27089=CARTESIAN_POINT('Ctrl Pts',(15.4999999999999,13.2690454743877,6.09637499999993));
#27090=CARTESIAN_POINT('Ctrl Pts',(16.466031646934,13.8267841057908,6.05470833333326));
#27091=CARTESIAN_POINT('Ctrl Pts',(17.4320632938681,14.3845227371939,6.0130416666666));
#27092=CARTESIAN_POINT('Ctrl Pts',(17.4320632938681,15.5000000000002,5.97137499999993));
#27093=CARTESIAN_POINT('Ctrl Pts',(17.4320632938681,16.6154772628064,5.92970833333326));
#27094=CARTESIAN_POINT('Ctrl Pts',(16.466031646934,17.1732158942095,5.8880416666666));
#27095=CARTESIAN_POINT('Ctrl Pts',(15.4999999999998,17.7309545256126,5.84637499999993));
#27096=CARTESIAN_POINT('Ctrl Pts',(14.5339683530657,17.1732158942095,5.80470833333326));
#27097=CARTESIAN_POINT('Ctrl Pts',(13.5679367061316,16.6154772628064,5.76304166666659));
#27098=CARTESIAN_POINT('Ctrl Pts',(13.5679367061316,15.5000000000001,5.72137499999993));
#27099=CARTESIAN_POINT('Ctrl Pts',(13.5679367061316,14.3845227371939,5.67970833333326));
#27100=CARTESIAN_POINT('Ctrl Pts',(14.5339683530657,13.8267841057908,5.63804166666659));
#27101=CARTESIAN_POINT('Ctrl Pts',(15.4999999999999,13.2690454743877,5.59637499999992));
#27102=CARTESIAN_POINT('Ctrl Pts',(16.466031646934,13.8267841057908,5.55470833333326));
#27103=CARTESIAN_POINT('Ctrl Pts',(17.4320632938681,14.3845227371939,5.51304166666659));
#27104=CARTESIAN_POINT('Ctrl Pts',(17.4320632938681,15.5000000000002,5.47137499999992));
#27105=CARTESIAN_POINT('Ctrl Pts',(17.4320632938681,16.6154772628064,5.42970833333325));
#27106=CARTESIAN_POINT('Ctrl Pts',(16.466031646934,17.1732158942095,5.38804166666659));
#27107=CARTESIAN_POINT('Ctrl Pts',(15.4999999999998,17.7309545256126,5.34637499999992));
#27108=CARTESIAN_POINT('Ctrl Pts',(14.5339683530657,17.1732158942095,5.30470833333325));
#27109=CARTESIAN_POINT('Ctrl Pts',(13.5679367061316,16.6154772628064,5.26304166666659));
#27110=CARTESIAN_POINT('Ctrl Pts',(13.5679367061316,15.5000000000001,5.22137499999992));
#27111=CARTESIAN_POINT('Ctrl Pts',(13.5679367061316,14.3845227371939,5.17970833333325));
#27112=CARTESIAN_POINT('Ctrl Pts',(14.5339683530657,13.8267841057908,5.13804166666659));
#27113=CARTESIAN_POINT('Ctrl Pts',(15.4999999999999,13.2690454743877,5.09637499999992));
#27114=CARTESIAN_POINT('Ctrl Pts',(16.466031646934,13.8267841057908,5.05470833333325));
#27115=CARTESIAN_POINT('Ctrl Pts',(17.4320632938681,14.3845227371939,5.01304166666658));
#27116=CARTESIAN_POINT('Ctrl Pts',(17.4320632938681,15.5000000000002,4.97137499999991));
#27117=CARTESIAN_POINT('Ctrl Pts',(17.4320632938681,16.6154772628064,4.92970833333325));
#27118=CARTESIAN_POINT('Ctrl Pts',(16.466031646934,17.1732158942095,4.88804166666658));
#27119=CARTESIAN_POINT('Ctrl Pts',(15.4999999999998,17.7309545256126,4.84637499999991));
#27120=CARTESIAN_POINT('Ctrl Pts',(14.5339683530657,17.1732158942095,4.80470833333325));
#27121=CARTESIAN_POINT('Ctrl Pts',(13.5679367061316,16.6154772628064,4.76304166666658));
#27122=CARTESIAN_POINT('Ctrl Pts',(13.5679367061316,15.5000000000001,4.72137499999991));
#27123=CARTESIAN_POINT('Ctrl Pts',(13.5679367061316,14.3845227371939,4.67970833333325));
#27124=CARTESIAN_POINT('Ctrl Pts',(14.5339683530657,13.8267841057908,4.63804166666658));
#27125=CARTESIAN_POINT('Ctrl Pts',(15.4999999999999,13.2690454743877,4.59637499999991));
#27126=CARTESIAN_POINT('Ctrl Pts',(16.466031646934,13.8267841057908,4.55470833333324));
#27127=CARTESIAN_POINT('Ctrl Pts',(17.4320632938681,14.3845227371939,4.51304166666658));
#27128=CARTESIAN_POINT('Ctrl Pts',(17.4320632938681,15.5000000000002,4.47137499999991));
#27129=CARTESIAN_POINT('Ctrl Pts',(17.4320632938681,16.6154772628064,4.42970833333324));
#27130=CARTESIAN_POINT('Ctrl Pts',(16.466031646934,17.1732158942095,4.38804166666657));
#27131=CARTESIAN_POINT('Ctrl Pts',(15.4999999999998,17.7309545256126,4.34637499999991));
#27132=CARTESIAN_POINT('Ctrl Pts',(14.5339683530657,17.1732158942095,4.30470833333324));
#27133=CARTESIAN_POINT('Ctrl Pts',(13.5679367061316,16.6154772628064,4.26304166666657));
#27134=CARTESIAN_POINT('Ctrl Pts',(13.5679367061316,15.5000000000001,4.22137499999991));
#27135=CARTESIAN_POINT('Ctrl Pts',(13.5679367061316,14.3845227371939,4.17970833333324));
#27136=CARTESIAN_POINT('Ctrl Pts',(14.5339683530657,13.8267841057908,4.13804166666657));
#27137=CARTESIAN_POINT('Ctrl Pts',(15.4999999999999,13.2690454743877,4.0963749999999));
#27138=CARTESIAN_POINT('Ctrl Pts',(16.466031646934,13.8267841057908,4.05470833333324));
#27139=CARTESIAN_POINT('Ctrl Pts',(17.4320632938681,14.3845227371939,4.01304166666657));
#27140=CARTESIAN_POINT('Ctrl Pts',(17.4320632938681,15.5000000000002,3.9713749999999));
#27141=CARTESIAN_POINT('Ctrl Pts',(17.4320632938681,16.6154772628064,3.92970833333323));
#27142=CARTESIAN_POINT('Ctrl Pts',(16.466031646934,17.1732158942095,3.88804166666657));
#27143=CARTESIAN_POINT('Ctrl Pts',(15.4999999999998,17.7309545256126,3.8463749999999));
#27144=CARTESIAN_POINT('Ctrl Pts',(14.5339683530657,17.1732158942095,3.80470833333323));
#27145=CARTESIAN_POINT('Ctrl Pts',(13.5679367061316,16.6154772628064,3.76304166666656));
#27146=CARTESIAN_POINT('Ctrl Pts',(13.5679367061316,15.5000000000001,3.7213749999999));
#27147=CARTESIAN_POINT('Ctrl Pts',(13.5679367061316,14.3845227371939,3.67970833333323));
#27148=CARTESIAN_POINT('Ctrl Pts',(14.5339683530657,13.8267841057908,3.63804166666656));
#27149=CARTESIAN_POINT('Ctrl Pts',(15.4999999999999,13.2690454743877,3.5963749999999));
#27150=CARTESIAN_POINT('Ctrl Pts',(16.466031646934,13.8267841057908,3.55470833333323));
#27151=CARTESIAN_POINT('Ctrl Pts',(17.4320632938681,14.3845227371939,3.51304166666656));
#27152=CARTESIAN_POINT('Ctrl Pts',(17.4320632938681,15.5000000000002,3.4713749999999));
#27153=CARTESIAN_POINT('Ctrl Pts',(17.4320632938681,16.6154772628064,3.42970833333323));
#27154=CARTESIAN_POINT('Ctrl Pts',(16.466031646934,17.1732158942095,3.38804166666656));
#27155=CARTESIAN_POINT('Ctrl Pts',(15.4999999999998,17.7309545256126,3.34637499999989));
#27156=CARTESIAN_POINT('Ctrl Pts',(14.5339683530657,17.1732158942095,3.30470833333323));
#27157=CARTESIAN_POINT('Ctrl Pts',(13.5679367061316,16.6154772628064,3.26304166666656));
#27158=CARTESIAN_POINT('Ctrl Pts',(13.5679367061316,15.5000000000001,3.22137499999989));
#27159=CARTESIAN_POINT('Ctrl Pts',(13.5679367061316,14.3845227371939,3.17970833333322));
#27160=CARTESIAN_POINT('Ctrl Pts',(14.5339683530657,13.8267841057908,3.13804166666656));
#27161=CARTESIAN_POINT('Ctrl Pts',(15.4999999999999,13.2690454743877,3.09637499999989));
#27162=CARTESIAN_POINT('Ctrl Pts',(16.466031646934,13.8267841057908,3.05470833333322));
#27163=CARTESIAN_POINT('Ctrl Pts',(17.4320632938681,14.3845227371939,3.01304166666656));
#27164=CARTESIAN_POINT('Ctrl Pts',(17.4320632938681,15.5000000000002,2.97137499999989));
#27165=CARTESIAN_POINT('Ctrl Pts',(17.4320632938681,16.6154772628064,2.92970833333322));
#27166=CARTESIAN_POINT('Ctrl Pts',(16.466031646934,17.1732158942095,2.88804166666655));
#27167=CARTESIAN_POINT('Ctrl Pts',(15.4999999999998,17.7309545256126,2.84637499999989));
#27168=CARTESIAN_POINT('Ctrl Pts',(14.5339683530657,17.1732158942095,2.80470833333322));
#27169=CARTESIAN_POINT('Ctrl Pts',(13.5679367061316,16.6154772628064,2.76304166666655));
#27170=CARTESIAN_POINT('Ctrl Pts',(13.5679367061316,15.5000000000001,2.72137499999989));
#27171=CARTESIAN_POINT('Ctrl Pts',(13.5679367061316,14.3845227371939,2.67970833333322));
#27172=CARTESIAN_POINT('Ctrl Pts',(14.5339683530657,13.8267841057908,2.63804166666655));
#27173=CARTESIAN_POINT('Ctrl Pts',(15.4999999999999,13.2690454743877,2.59637499999988));
#27174=CARTESIAN_POINT('Ctrl Pts',(16.466031646934,13.8267841057908,2.55470833333322));
#27175=CARTESIAN_POINT('Ctrl Pts',(17.4320632938681,14.3845227371939,2.51304166666655));
#27176=CARTESIAN_POINT('Ctrl Pts',(17.4320632938681,15.5000000000002,2.47137499999988));
#27177=CARTESIAN_POINT('Ctrl Pts',(17.4320632938681,16.6154772628064,2.42970833333321));
#27178=CARTESIAN_POINT('Ctrl Pts',(16.466031646934,17.1732158942095,2.38804166666655));
#27179=CARTESIAN_POINT('Ctrl Pts',(15.4999999999998,17.7309545256126,2.34637499999988));
#27180=CARTESIAN_POINT('Ctrl Pts',(14.5339683530657,17.1732158942095,2.30470833333321));
#27181=CARTESIAN_POINT('Ctrl Pts',(13.5679367061316,16.6154772628064,2.26304166666655));
#27182=CARTESIAN_POINT('Ctrl Pts',(13.5679367061316,15.5000000000001,2.22137499999988));
#27183=CARTESIAN_POINT('Ctrl Pts',(13.5679367061316,14.3845227371939,2.17970833333321));
#27184=CARTESIAN_POINT('Ctrl Pts',(14.5339683530657,13.8267841057908,2.13804166666654));
#27185=CARTESIAN_POINT('Ctrl Pts',(15.4999999999999,13.2690454743877,2.09637499999988));
#27186=CARTESIAN_POINT('Ctrl Pts',(16.466031646934,13.8267841057908,2.05470833333321));
#27187=CARTESIAN_POINT('Ctrl Pts',(17.4320632938681,14.3845227371939,2.01304166666654));
#27188=CARTESIAN_POINT('Ctrl Pts',(17.4320632938681,15.5000000000002,1.97137499999988));
#27189=CARTESIAN_POINT('Ctrl Pts',(17.4320632938681,16.6154772628064,1.92970833333321));
#27190=CARTESIAN_POINT('Ctrl Pts',(16.466031646934,17.1732158942095,1.88804166666654));
#27191=CARTESIAN_POINT('Ctrl Pts',(15.4999999999998,17.7309545256126,1.84637499999987));
#27192=CARTESIAN_POINT('Ctrl Pts',(14.5339683530657,17.1732158942095,1.80470833333321));
#27193=CARTESIAN_POINT('Ctrl Pts',(13.5679367061316,16.6154772628064,1.76304166666654));
#27194=CARTESIAN_POINT('Ctrl Pts',(13.5679367061316,15.5000000000001,1.72137499999987));
#27195=CARTESIAN_POINT('Ctrl Pts',(13.5679367061316,14.3845227371939,1.67970833333321));
#27196=CARTESIAN_POINT('Ctrl Pts',(14.5339683530657,13.8267841057908,1.63804166666654));
#27197=CARTESIAN_POINT('Ctrl Pts',(15.4999999999999,13.2690454743877,1.59637499999987));
#27198=CARTESIAN_POINT('Ctrl Pts',(16.466031646934,13.8267841057908,1.5547083333332));
#27199=CARTESIAN_POINT('Ctrl Pts',(17.4320632938681,14.3845227371939,1.51304166666654));
#27200=CARTESIAN_POINT('Ctrl Pts',(17.4320632938681,15.5000000000002,1.47137499999987));
#27201=CARTESIAN_POINT('Ctrl Pts',(17.4320632938681,16.6154772628064,1.4297083333332));
#27202=CARTESIAN_POINT('Ctrl Pts',(16.466031646934,17.1732158942095,1.38804166666653));
#27203=CARTESIAN_POINT('Ctrl Pts',(15.4999999999998,17.7309545256126,1.34637499999987));
#27204=CARTESIAN_POINT('Ctrl Pts',(14.5339683530657,17.1732158942095,1.3047083333332));
#27205=CARTESIAN_POINT('Ctrl Pts',(13.5679367061316,16.6154772628064,1.26304166666653));
#27206=CARTESIAN_POINT('Ctrl Pts',(13.5679367061316,15.5000000000001,1.22137499999987));
#27207=CARTESIAN_POINT('Ctrl Pts',(13.5679367061316,14.3845227371939,1.1797083333332));
#27208=CARTESIAN_POINT('Ctrl Pts',(14.5339683530657,13.8267841057908,1.13804166666653));
#27209=CARTESIAN_POINT('Ctrl Pts',(15.4999999999999,13.2690454743877,1.09637499999986));
#27210=CARTESIAN_POINT('Ctrl Pts',(16.466031646934,13.8267841057908,1.0547083333332));
#27211=CARTESIAN_POINT('Ctrl Pts',(17.4320632938681,14.3845227371939,1.01304166666653));
#27212=CARTESIAN_POINT('Ctrl Pts',(17.4320632938681,15.5000000000002,0.971374999999861));
#27213=CARTESIAN_POINT('Ctrl Pts',(17.4320632938681,16.6154772628064,0.929708333333194));
#27214=CARTESIAN_POINT('Ctrl Pts',(16.466031646934,17.1732158942095,0.888041666666528));
#27215=CARTESIAN_POINT('Ctrl Pts',(15.4999999999998,17.7309545256126,0.846374999999861));
#27216=CARTESIAN_POINT('Ctrl Pts',(14.5339683530657,17.1732158942095,0.804708333333194));
#27217=CARTESIAN_POINT('Ctrl Pts',(13.5679367061316,16.6154772628064,0.763041666666526));
#27218=CARTESIAN_POINT('Ctrl Pts',(13.5679367061316,15.5000000000001,0.721374999999859));
#27219=CARTESIAN_POINT('Ctrl Pts',(13.5679367061316,14.3845227371939,0.679708333333192));
#27220=CARTESIAN_POINT('Ctrl Pts',(14.5339683530657,13.8267841057908,0.638041666666525));
#27221=CARTESIAN_POINT('Ctrl Pts',(15.4999999999999,13.2690454743877,0.596374999999858));
#27222=CARTESIAN_POINT('Ctrl Pts',(16.466031646934,13.8267841057908,0.55470833333319));
#27223=CARTESIAN_POINT('Ctrl Pts',(17.4320632938681,14.3845227371939,0.513041666666523));
#27224=CARTESIAN_POINT('Ctrl Pts',(17.4320632938681,15.5000000000002,0.471374999999856));
#27225=CARTESIAN_POINT('Ctrl Pts',(17.4320632938681,16.6154772628064,0.429708333333188));
#27226=CARTESIAN_POINT('Ctrl Pts',(16.466031646934,17.1732158942095,0.388041666666521));
#27227=CARTESIAN_POINT('Ctrl Pts',(15.4999999999998,17.7309545256126,0.346374999999854));
#27228=CARTESIAN_POINT('Ctrl Pts',(14.5339683530657,17.1732158942095,0.304708333333186));
#27229=CARTESIAN_POINT('Ctrl Pts',(13.5679367061316,16.6154772628064,0.263041666666519));
#27230=CARTESIAN_POINT('Ctrl Pts',(13.5679367061316,15.5000000000001,0.221374999999852));
#27231=CARTESIAN_POINT('Ctrl Pts',(13.5679367061316,14.3845227371939,0.179708333333185));
#27232=CARTESIAN_POINT('Ctrl Pts',(14.5339683530657,13.8267841057908,0.138041666666517));
#27233=CARTESIAN_POINT('Ctrl Pts',(15.4999999999999,13.2690454743877,0.0963749999998501));
#27234=CARTESIAN_POINT('Ctrl Pts',(16.466031646934,13.8267841057908,0.0547083333331828));
#27235=CARTESIAN_POINT('Ctrl Pts',(17.4320632938681,14.3845227371939,0.0130416666665155));
#27236=CARTESIAN_POINT('Ctrl Pts',(17.4320632938681,15.5000000000002,-0.0286250000001518));
#27237=CARTESIAN_POINT('Ctrl Pts',(17.4320632938681,16.6154772628064,-0.0702916666668191));
#27238=CARTESIAN_POINT('Ctrl Pts',(16.466031646934,17.1732158942095,-0.111958333333486));
#27239=CARTESIAN_POINT('Ctrl Pts',(15.4999999999998,17.7309545256126,-0.153625000000154));
#27240=CARTESIAN_POINT('Ctrl Pts',(14.5339683530657,17.1732158942095,-0.195291666666821));
#27241=CARTESIAN_POINT('Ctrl Pts',(13.5679367061316,16.6154772628064,-0.236958333333488));
#27242=CARTESIAN_POINT('Ctrl Pts',(13.5679367061316,15.5000000000001,-0.278625000000155));
#27243=CARTESIAN_POINT('Ctrl Pts',(13.5679367061316,14.3845227371939,-0.320291666666821));
#27244=CARTESIAN_POINT('Ctrl Pts',(14.5339683530657,13.8267841057908,-0.361958333333488));
#27245=CARTESIAN_POINT('Ctrl Pts',(15.4999999999999,13.2690454743877,-0.403625000000156));
#27246=CARTESIAN_POINT('Ctrl Pts',(16.466031646934,13.8267841057908,-0.445291666666823));
#27247=CARTESIAN_POINT('Ctrl Pts',(17.4320632938681,14.3845227371939,-0.48695833333349));
#27248=CARTESIAN_POINT('Ctrl Pts',(17.4320632938681,15.5000000000002,-0.528625000000157));
#27249=CARTESIAN_POINT('Ctrl Pts',(17.4320632938681,16.6154772628064,-0.570291666666825));
#27250=CARTESIAN_POINT('Ctrl Pts',(16.466031646934,17.1732158942095,-0.611958333333492));
#27251=CARTESIAN_POINT('Ctrl Pts',(15.4999999999998,17.7309545256126,-0.653625000000159));
#27252=CARTESIAN_POINT('Ctrl Pts',(14.5339683530657,17.1732158942095,-0.695291666666827));
#27253=CARTESIAN_POINT('Ctrl Pts',(13.5679367061316,16.6154772628064,-0.736958333333494));
#27254=CARTESIAN_POINT('Ctrl Pts',(13.5679367061316,15.5000000000001,-0.778625000000161));
#27255=CARTESIAN_POINT('Ctrl Pts',(13.5679367061316,14.3845227371939,-0.820291666666829));
#27256=CARTESIAN_POINT('Ctrl Pts',(14.5339683530657,13.8267841057908,-0.861958333333496));
#27257=CARTESIAN_POINT('Ctrl Pts',(15.4999999999999,13.2690454743877,-0.903625000000163));
#27258=CARTESIAN_POINT('Ctrl Pts',(16.466031646934,13.8267841057908,-0.94529166666683));
#27259=CARTESIAN_POINT('Ctrl Pts',(17.4320632938681,14.3845227371939,-0.986958333333498));
#27260=CARTESIAN_POINT('Ctrl Pts',(17.4320632938681,15.5000000000002,-1.02862500000016));
#27261=CARTESIAN_POINT('Ctrl Pts',(17.4320632938681,16.6154772628064,-1.07029166666683));
#27262=CARTESIAN_POINT('Ctrl Pts',(16.466031646934,17.1732158942095,-1.1119583333335));
#27263=CARTESIAN_POINT('Ctrl Pts',(15.4999999999998,17.7309545256126,-1.15362500000017));
#27264=CARTESIAN_POINT('Ctrl Pts',(14.5339683530657,17.1732158942095,-1.19529166666683));
#27265=CARTESIAN_POINT('Ctrl Pts',(13.5679367061316,16.6154772628064,-1.2369583333335));
#27266=CARTESIAN_POINT('Ctrl Pts',(13.5679367061316,15.5000000000001,-1.27862500000017));
#27267=CARTESIAN_POINT('Ctrl Pts',(13.5679367061316,14.3845227371939,-1.32029166666684));
#27268=CARTESIAN_POINT('Ctrl Pts',(14.5339683530657,13.8267841057908,-1.3619583333335));
#27269=CARTESIAN_POINT('Ctrl Pts',(15.4999999999999,13.2690454743877,-1.40362500000017));
#27270=CARTESIAN_POINT('Ctrl Pts',(16.466031646934,13.8267841057908,-1.44529166666684));
#27271=CARTESIAN_POINT('Ctrl Pts',(17.4320632938681,14.3845227371939,-1.4869583333335));
#27272=CARTESIAN_POINT('Ctrl Pts',(17.4320632938681,15.5000000000002,-1.52862500000017));
#27273=CARTESIAN_POINT('Ctrl Pts',(17.4320632938681,16.6154772628064,-1.57029166666684));
#27274=CARTESIAN_POINT('Ctrl Pts',(16.466031646934,17.1732158942095,-1.61195833333351));
#27275=CARTESIAN_POINT('Ctrl Pts',(15.4999999999998,17.7309545256126,-1.65362500000017));
#27276=CARTESIAN_POINT('Ctrl Pts',(14.5339683530657,17.1732158942095,-1.69529166666684));
#27277=CARTESIAN_POINT('Ctrl Pts',(13.5679367061316,16.6154772628064,-1.73695833333351));
#27278=CARTESIAN_POINT('Ctrl Pts',(13.5679367061316,15.5000000000001,-1.77862500000017));
#27279=CARTESIAN_POINT('Ctrl Pts',(13.5679367061316,14.3845227371939,-1.82029166666684));
#27280=CARTESIAN_POINT('Ctrl Pts',(14.5339683530657,13.8267841057908,-1.86195833333351));
#27281=CARTESIAN_POINT('Ctrl Pts',(15.4999999999999,13.2690454743877,-1.90362500000018));
#27282=CARTESIAN_POINT('Ctrl Pts',(16.466031646934,13.8267841057908,-1.94529166666684));
#27283=CARTESIAN_POINT('Ctrl Pts',(17.4320632938681,14.3845227371939,-1.98695833333351));
#27284=CARTESIAN_POINT('Ctrl Pts',(17.4320632938681,15.5000000000002,-2.02862500000018));
#27285=CARTESIAN_POINT('Ctrl Pts',(17.4320632938681,16.6154772628064,-2.07029166666685));
#27286=CARTESIAN_POINT('Ctrl Pts',(16.466031646934,17.1732158942095,-2.11195833333351));
#27287=CARTESIAN_POINT('Ctrl Pts',(15.4999999999998,17.7309545256126,-2.15362500000018));
#27288=CARTESIAN_POINT('Ctrl Pts',(14.5339683530657,17.1732158942095,-2.19529166666685));
#27289=CARTESIAN_POINT('Ctrl Pts',(14.1783071398502,16.9678747970192,-2.21063196867905));
#27290=CARTESIAN_POINT('Ctrl Pts',(13.9369173167912,16.6356236599185,-2.22824840486548));
#27291=CARTESIAN_POINT('',(14.2215513317124,16.4288320706155,-2.02512305032131));
#27292=CARTESIAN_POINT('Ctrl Pts',(13.9406917842495,15.2436450846259,10.4122404735808));
#27293=CARTESIAN_POINT('Ctrl Pts',(14.0620451873461,14.5054990725559,10.3753299573543));
#27294=CARTESIAN_POINT('Ctrl Pts',(14.7098797632094,14.1314716057908,10.3411666666667));
#27295=CARTESIAN_POINT('Ctrl Pts',(15.4999999999999,13.6752954743877,10.2995));
#27296=CARTESIAN_POINT('Ctrl Pts',(16.2901202367903,14.1314716057908,10.2578333333333));
#27297=CARTESIAN_POINT('Ctrl Pts',(17.0802404735807,14.5876477371939,10.2161666666667));
#27298=CARTESIAN_POINT('Ctrl Pts',(17.0802404735807,15.5000000000002,10.1745));
#27299=CARTESIAN_POINT('Ctrl Pts',(17.0802404735807,16.4123522628064,10.1328333333333));
#27300=CARTESIAN_POINT('Ctrl Pts',(16.2901202367902,16.8685283942095,10.0911666666667));
#27301=CARTESIAN_POINT('Ctrl Pts',(15.4999999999998,17.3247045256126,10.0495));
#27302=CARTESIAN_POINT('Ctrl Pts',(14.7098797632094,16.8685283942095,10.0078333333333));
#27303=CARTESIAN_POINT('Ctrl Pts',(13.919759526419,16.4123522628064,9.96616666666665));
#27304=CARTESIAN_POINT('Ctrl Pts',(13.919759526419,15.5000000000001,9.92449999999998));
#27305=CARTESIAN_POINT('Ctrl Pts',(13.919759526419,14.5876477371939,9.88283333333331));
#27306=CARTESIAN_POINT('Ctrl Pts',(14.7098797632094,14.1314716057908,9.84116666666665));
#27307=CARTESIAN_POINT('Ctrl Pts',(15.4999999999999,13.6752954743877,9.79949999999998));
#27308=CARTESIAN_POINT('Ctrl Pts',(16.2901202367903,14.1314716057908,9.75783333333331));
#27309=CARTESIAN_POINT('Ctrl Pts',(17.0802404735807,14.5876477371939,9.71616666666665));
#27310=CARTESIAN_POINT('Ctrl Pts',(17.0802404735807,15.5000000000002,9.67449999999998));
#27311=CARTESIAN_POINT('Ctrl Pts',(17.0802404735807,16.4123522628064,9.63283333333331));
#27312=CARTESIAN_POINT('Ctrl Pts',(16.2901202367902,16.8685283942095,9.59116666666664));
#27313=CARTESIAN_POINT('Ctrl Pts',(15.4999999999998,17.3247045256126,9.54949999999998));
#27314=CARTESIAN_POINT('Ctrl Pts',(14.7098797632094,16.8685283942095,9.50783333333331));
#27315=CARTESIAN_POINT('Ctrl Pts',(13.919759526419,16.4123522628064,9.46616666666664));
#27316=CARTESIAN_POINT('Ctrl Pts',(13.919759526419,15.5000000000001,9.42449999999998));
#27317=CARTESIAN_POINT('Ctrl Pts',(13.919759526419,14.5876477371939,9.38283333333331));
#27318=CARTESIAN_POINT('Ctrl Pts',(14.7098797632094,14.1314716057908,9.34116666666664));
#27319=CARTESIAN_POINT('Ctrl Pts',(15.4999999999999,13.6752954743877,9.29949999999997));
#27320=CARTESIAN_POINT('Ctrl Pts',(16.2901202367903,14.1314716057908,9.25783333333331));
#27321=CARTESIAN_POINT('Ctrl Pts',(17.0802404735807,14.5876477371939,9.21616666666664));
#27322=CARTESIAN_POINT('Ctrl Pts',(17.0802404735807,15.5000000000002,9.17449999999997));
#27323=CARTESIAN_POINT('Ctrl Pts',(17.0802404735807,16.4123522628064,9.13283333333331));
#27324=CARTESIAN_POINT('Ctrl Pts',(16.2901202367902,16.8685283942095,9.09116666666664));
#27325=CARTESIAN_POINT('Ctrl Pts',(15.4999999999998,17.3247045256126,9.04949999999997));
#27326=CARTESIAN_POINT('Ctrl Pts',(14.7098797632094,16.8685283942095,9.0078333333333));
#27327=CARTESIAN_POINT('Ctrl Pts',(13.919759526419,16.4123522628064,8.96616666666664));
#27328=CARTESIAN_POINT('Ctrl Pts',(13.919759526419,15.5000000000001,8.92449999999997));
#27329=CARTESIAN_POINT('Ctrl Pts',(13.919759526419,14.5876477371939,8.8828333333333));
#27330=CARTESIAN_POINT('Ctrl Pts',(14.7098797632094,14.1314716057908,8.84116666666664));
#27331=CARTESIAN_POINT('Ctrl Pts',(15.4999999999999,13.6752954743877,8.79949999999997));
#27332=CARTESIAN_POINT('Ctrl Pts',(16.2901202367903,14.1314716057908,8.7578333333333));
#27333=CARTESIAN_POINT('Ctrl Pts',(17.0802404735807,14.5876477371939,8.71616666666663));
#27334=CARTESIAN_POINT('Ctrl Pts',(17.0802404735807,15.5000000000002,8.67449999999997));
#27335=CARTESIAN_POINT('Ctrl Pts',(17.0802404735807,16.4123522628064,8.6328333333333));
#27336=CARTESIAN_POINT('Ctrl Pts',(16.2901202367902,16.8685283942095,8.59116666666663));
#27337=CARTESIAN_POINT('Ctrl Pts',(15.4999999999998,17.3247045256126,8.54949999999996));
#27338=CARTESIAN_POINT('Ctrl Pts',(14.7098797632094,16.8685283942095,8.50783333333329));
#27339=CARTESIAN_POINT('Ctrl Pts',(13.919759526419,16.4123522628064,8.46616666666663));
#27340=CARTESIAN_POINT('Ctrl Pts',(13.919759526419,15.5000000000001,8.42449999999996));
#27341=CARTESIAN_POINT('Ctrl Pts',(13.919759526419,14.5876477371939,8.38283333333329));
#27342=CARTESIAN_POINT('Ctrl Pts',(14.7098797632094,14.1314716057908,8.34116666666663));
#27343=CARTESIAN_POINT('Ctrl Pts',(15.4999999999999,13.6752954743877,8.29949999999996));
#27344=CARTESIAN_POINT('Ctrl Pts',(16.2901202367903,14.1314716057908,8.25783333333329));
#27345=CARTESIAN_POINT('Ctrl Pts',(17.0802404735807,14.5876477371939,8.21616666666663));
#27346=CARTESIAN_POINT('Ctrl Pts',(17.0802404735807,15.5000000000002,8.17449999999996));
#27347=CARTESIAN_POINT('Ctrl Pts',(17.0802404735807,16.4123522628064,8.13283333333329));
#27348=CARTESIAN_POINT('Ctrl Pts',(16.2901202367902,16.8685283942095,8.09116666666663));
#27349=CARTESIAN_POINT('Ctrl Pts',(15.4999999999998,17.3247045256126,8.04949999999996));
#27350=CARTESIAN_POINT('Ctrl Pts',(14.7098797632094,16.8685283942095,8.00783333333329));
#27351=CARTESIAN_POINT('Ctrl Pts',(13.919759526419,16.4123522628064,7.96616666666662));
#27352=CARTESIAN_POINT('Ctrl Pts',(13.919759526419,15.5000000000001,7.92449999999996));
#27353=CARTESIAN_POINT('Ctrl Pts',(13.919759526419,14.5876477371939,7.88283333333329));
#27354=CARTESIAN_POINT('Ctrl Pts',(14.7098797632094,14.1314716057908,7.84116666666662));
#27355=CARTESIAN_POINT('Ctrl Pts',(15.4999999999999,13.6752954743877,7.79949999999995));
#27356=CARTESIAN_POINT('Ctrl Pts',(16.2901202367903,14.1314716057908,7.75783333333329));
#27357=CARTESIAN_POINT('Ctrl Pts',(17.0802404735807,14.5876477371939,7.71616666666662));
#27358=CARTESIAN_POINT('Ctrl Pts',(17.0802404735807,15.5000000000002,7.67449999999995));
#27359=CARTESIAN_POINT('Ctrl Pts',(17.0802404735807,16.4123522628064,7.63283333333328));
#27360=CARTESIAN_POINT('Ctrl Pts',(16.2901202367902,16.8685283942095,7.59116666666662));
#27361=CARTESIAN_POINT('Ctrl Pts',(15.4999999999998,17.3247045256126,7.54949999999995));
#27362=CARTESIAN_POINT('Ctrl Pts',(14.7098797632094,16.8685283942095,7.50783333333328));
#27363=CARTESIAN_POINT('Ctrl Pts',(13.919759526419,16.4123522628064,7.46616666666662));
#27364=CARTESIAN_POINT('Ctrl Pts',(13.919759526419,15.5000000000001,7.42449999999995));
#27365=CARTESIAN_POINT('Ctrl Pts',(13.919759526419,14.5876477371939,7.38283333333328));
#27366=CARTESIAN_POINT('Ctrl Pts',(14.7098797632094,14.1314716057908,7.34116666666661));
#27367=CARTESIAN_POINT('Ctrl Pts',(15.4999999999999,13.6752954743877,7.29949999999995));
#27368=CARTESIAN_POINT('Ctrl Pts',(16.2901202367903,14.1314716057908,7.25783333333328));
#27369=CARTESIAN_POINT('Ctrl Pts',(17.0802404735807,14.5876477371939,7.21616666666661));
#27370=CARTESIAN_POINT('Ctrl Pts',(17.0802404735807,15.5000000000002,7.17449999999995));
#27371=CARTESIAN_POINT('Ctrl Pts',(17.0802404735807,16.4123522628064,7.13283333333328));
#27372=CARTESIAN_POINT('Ctrl Pts',(16.2901202367902,16.8685283942095,7.09116666666661));
#27373=CARTESIAN_POINT('Ctrl Pts',(15.4999999999998,17.3247045256126,7.04949999999994));
#27374=CARTESIAN_POINT('Ctrl Pts',(14.7098797632094,16.8685283942095,7.00783333333328));
#27375=CARTESIAN_POINT('Ctrl Pts',(13.919759526419,16.4123522628064,6.96616666666661));
#27376=CARTESIAN_POINT('Ctrl Pts',(13.919759526419,15.5000000000001,6.92449999999994));
#27377=CARTESIAN_POINT('Ctrl Pts',(13.919759526419,14.5876477371939,6.88283333333327));
#27378=CARTESIAN_POINT('Ctrl Pts',(14.7098797632094,14.1314716057908,6.84116666666661));
#27379=CARTESIAN_POINT('Ctrl Pts',(15.4999999999999,13.6752954743877,6.79949999999994));
#27380=CARTESIAN_POINT('Ctrl Pts',(16.2901202367903,14.1314716057908,6.75783333333327));
#27381=CARTESIAN_POINT('Ctrl Pts',(17.0802404735807,14.5876477371939,6.71616666666661));
#27382=CARTESIAN_POINT('Ctrl Pts',(17.0802404735807,15.5000000000002,6.67449999999994));
#27383=CARTESIAN_POINT('Ctrl Pts',(17.0802404735807,16.4123522628064,6.63283333333327));
#27384=CARTESIAN_POINT('Ctrl Pts',(16.2901202367902,16.8685283942095,6.59116666666661));
#27385=CARTESIAN_POINT('Ctrl Pts',(15.4999999999998,17.3247045256126,6.54949999999994));
#27386=CARTESIAN_POINT('Ctrl Pts',(14.7098797632094,16.8685283942095,6.50783333333327));
#27387=CARTESIAN_POINT('Ctrl Pts',(13.919759526419,16.4123522628064,6.4661666666666));
#27388=CARTESIAN_POINT('Ctrl Pts',(13.919759526419,15.5000000000001,6.42449999999994));
#27389=CARTESIAN_POINT('Ctrl Pts',(13.919759526419,14.5876477371939,6.38283333333327));
#27390=CARTESIAN_POINT('Ctrl Pts',(14.7098797632094,14.1314716057908,6.3411666666666));
#27391=CARTESIAN_POINT('Ctrl Pts',(15.4999999999999,13.6752954743877,6.29949999999993));
#27392=CARTESIAN_POINT('Ctrl Pts',(16.2901202367903,14.1314716057908,6.25783333333327));
#27393=CARTESIAN_POINT('Ctrl Pts',(17.0802404735807,14.5876477371939,6.2161666666666));
#27394=CARTESIAN_POINT('Ctrl Pts',(17.0802404735807,15.5000000000002,6.17449999999993));
#27395=CARTESIAN_POINT('Ctrl Pts',(17.0802404735807,16.4123522628064,6.13283333333326));
#27396=CARTESIAN_POINT('Ctrl Pts',(16.2901202367902,16.8685283942095,6.0911666666666));
#27397=CARTESIAN_POINT('Ctrl Pts',(15.4999999999998,17.3247045256126,6.04949999999993));
#27398=CARTESIAN_POINT('Ctrl Pts',(14.7098797632094,16.8685283942095,6.00783333333326));
#27399=CARTESIAN_POINT('Ctrl Pts',(13.919759526419,16.4123522628064,5.9661666666666));
#27400=CARTESIAN_POINT('Ctrl Pts',(13.919759526419,15.5000000000001,5.92449999999993));
#27401=CARTESIAN_POINT('Ctrl Pts',(13.919759526419,14.5876477371939,5.88283333333326));
#27402=CARTESIAN_POINT('Ctrl Pts',(14.7098797632094,14.1314716057908,5.8411666666666));
#27403=CARTESIAN_POINT('Ctrl Pts',(15.4999999999999,13.6752954743877,5.79949999999993));
#27404=CARTESIAN_POINT('Ctrl Pts',(16.2901202367903,14.1314716057908,5.75783333333326));
#27405=CARTESIAN_POINT('Ctrl Pts',(17.0802404735807,14.5876477371939,5.71616666666659));
#27406=CARTESIAN_POINT('Ctrl Pts',(17.0802404735807,15.5000000000002,5.67449999999993));
#27407=CARTESIAN_POINT('Ctrl Pts',(17.0802404735807,16.4123522628064,5.63283333333326));
#27408=CARTESIAN_POINT('Ctrl Pts',(16.2901202367902,16.8685283942095,5.59116666666659));
#27409=CARTESIAN_POINT('Ctrl Pts',(15.4999999999998,17.3247045256126,5.54949999999992));
#27410=CARTESIAN_POINT('Ctrl Pts',(14.7098797632094,16.8685283942095,5.50783333333326));
#27411=CARTESIAN_POINT('Ctrl Pts',(13.919759526419,16.4123522628064,5.46616666666659));
#27412=CARTESIAN_POINT('Ctrl Pts',(13.919759526419,15.5000000000001,5.42449999999992));
#27413=CARTESIAN_POINT('Ctrl Pts',(13.919759526419,14.5876477371939,5.38283333333326));
#27414=CARTESIAN_POINT('Ctrl Pts',(14.7098797632094,14.1314716057908,5.34116666666659));
#27415=CARTESIAN_POINT('Ctrl Pts',(15.4999999999999,13.6752954743877,5.29949999999992));
#27416=CARTESIAN_POINT('Ctrl Pts',(16.2901202367903,14.1314716057908,5.25783333333325));
#27417=CARTESIAN_POINT('Ctrl Pts',(17.0802404735807,14.5876477371939,5.21616666666659));
#27418=CARTESIAN_POINT('Ctrl Pts',(17.0802404735807,15.5000000000002,5.17449999999992));
#27419=CARTESIAN_POINT('Ctrl Pts',(17.0802404735807,16.4123522628064,5.13283333333325));
#27420=CARTESIAN_POINT('Ctrl Pts',(16.2901202367902,16.8685283942095,5.09116666666658));
#27421=CARTESIAN_POINT('Ctrl Pts',(15.4999999999998,17.3247045256126,5.04949999999992));
#27422=CARTESIAN_POINT('Ctrl Pts',(14.7098797632094,16.8685283942095,5.00783333333325));
#27423=CARTESIAN_POINT('Ctrl Pts',(13.919759526419,16.4123522628064,4.96616666666658));
#27424=CARTESIAN_POINT('Ctrl Pts',(13.919759526419,15.5000000000001,4.92449999999992));
#27425=CARTESIAN_POINT('Ctrl Pts',(13.919759526419,14.5876477371939,4.88283333333325));
#27426=CARTESIAN_POINT('Ctrl Pts',(14.7098797632094,14.1314716057908,4.84116666666658));
#27427=CARTESIAN_POINT('Ctrl Pts',(15.4999999999999,13.6752954743877,4.79949999999991));
#27428=CARTESIAN_POINT('Ctrl Pts',(16.2901202367903,14.1314716057908,4.75783333333325));
#27429=CARTESIAN_POINT('Ctrl Pts',(17.0802404735807,14.5876477371939,4.71616666666658));
#27430=CARTESIAN_POINT('Ctrl Pts',(17.0802404735807,15.5000000000002,4.67449999999991));
#27431=CARTESIAN_POINT('Ctrl Pts',(17.0802404735807,16.4123522628064,4.63283333333325));
#27432=CARTESIAN_POINT('Ctrl Pts',(16.2901202367902,16.8685283942095,4.59116666666658));
#27433=CARTESIAN_POINT('Ctrl Pts',(15.4999999999998,17.3247045256126,4.54949999999991));
#27434=CARTESIAN_POINT('Ctrl Pts',(14.7098797632094,16.8685283942095,4.50783333333324));
#27435=CARTESIAN_POINT('Ctrl Pts',(13.919759526419,16.4123522628064,4.46616666666658));
#27436=CARTESIAN_POINT('Ctrl Pts',(13.919759526419,15.5000000000001,4.42449999999991));
#27437=CARTESIAN_POINT('Ctrl Pts',(13.919759526419,14.5876477371939,4.38283333333324));
#27438=CARTESIAN_POINT('Ctrl Pts',(14.7098797632094,14.1314716057908,4.34116666666657));
#27439=CARTESIAN_POINT('Ctrl Pts',(15.4999999999999,13.6752954743877,4.29949999999991));
#27440=CARTESIAN_POINT('Ctrl Pts',(16.2901202367903,14.1314716057908,4.25783333333324));
#27441=CARTESIAN_POINT('Ctrl Pts',(17.0802404735807,14.5876477371939,4.21616666666657));
#27442=CARTESIAN_POINT('Ctrl Pts',(17.0802404735807,15.5000000000002,4.17449999999991));
#27443=CARTESIAN_POINT('Ctrl Pts',(17.0802404735807,16.4123522628064,4.13283333333324));
#27444=CARTESIAN_POINT('Ctrl Pts',(16.2901202367902,16.8685283942095,4.09116666666657));
#27445=CARTESIAN_POINT('Ctrl Pts',(15.4999999999998,17.3247045256126,4.0494999999999));
#27446=CARTESIAN_POINT('Ctrl Pts',(14.7098797632094,16.8685283942095,4.00783333333324));
#27447=CARTESIAN_POINT('Ctrl Pts',(13.919759526419,16.4123522628064,3.96616666666657));
#27448=CARTESIAN_POINT('Ctrl Pts',(13.919759526419,15.5000000000001,3.9244999999999));
#27449=CARTESIAN_POINT('Ctrl Pts',(13.919759526419,14.5876477371939,3.88283333333323));
#27450=CARTESIAN_POINT('Ctrl Pts',(14.7098797632094,14.1314716057908,3.84116666666657));
#27451=CARTESIAN_POINT('Ctrl Pts',(15.4999999999999,13.6752954743877,3.7994999999999));
#27452=CARTESIAN_POINT('Ctrl Pts',(16.2901202367903,14.1314716057908,3.75783333333323));
#27453=CARTESIAN_POINT('Ctrl Pts',(17.0802404735807,14.5876477371939,3.71616666666657));
#27454=CARTESIAN_POINT('Ctrl Pts',(17.0802404735807,15.5000000000002,3.6744999999999));
#27455=CARTESIAN_POINT('Ctrl Pts',(17.0802404735807,16.4123522628064,3.63283333333323));
#27456=CARTESIAN_POINT('Ctrl Pts',(16.2901202367902,16.8685283942095,3.59116666666656));
#27457=CARTESIAN_POINT('Ctrl Pts',(15.4999999999998,17.3247045256126,3.5494999999999));
#27458=CARTESIAN_POINT('Ctrl Pts',(14.7098797632094,16.8685283942095,3.50783333333323));
#27459=CARTESIAN_POINT('Ctrl Pts',(13.919759526419,16.4123522628064,3.46616666666656));
#27460=CARTESIAN_POINT('Ctrl Pts',(13.919759526419,15.5000000000001,3.4244999999999));
#27461=CARTESIAN_POINT('Ctrl Pts',(13.919759526419,14.5876477371939,3.38283333333323));
#27462=CARTESIAN_POINT('Ctrl Pts',(14.7098797632094,14.1314716057908,3.34116666666656));
#27463=CARTESIAN_POINT('Ctrl Pts',(15.4999999999999,13.6752954743877,3.29949999999989));
#27464=CARTESIAN_POINT('Ctrl Pts',(16.2901202367903,14.1314716057908,3.25783333333323));
#27465=CARTESIAN_POINT('Ctrl Pts',(17.0802404735807,14.5876477371939,3.21616666666656));
#27466=CARTESIAN_POINT('Ctrl Pts',(17.0802404735807,15.5000000000002,3.17449999999989));
#27467=CARTESIAN_POINT('Ctrl Pts',(17.0802404735807,16.4123522628064,3.13283333333323));
#27468=CARTESIAN_POINT('Ctrl Pts',(16.2901202367902,16.8685283942095,3.09116666666656));
#27469=CARTESIAN_POINT('Ctrl Pts',(15.4999999999998,17.3247045256126,3.04949999999989));
#27470=CARTESIAN_POINT('Ctrl Pts',(14.7098797632094,16.8685283942095,3.00783333333322));
#27471=CARTESIAN_POINT('Ctrl Pts',(13.919759526419,16.4123522628064,2.96616666666656));
#27472=CARTESIAN_POINT('Ctrl Pts',(13.919759526419,15.5000000000001,2.92449999999989));
#27473=CARTESIAN_POINT('Ctrl Pts',(13.919759526419,14.5876477371939,2.88283333333322));
#27474=CARTESIAN_POINT('Ctrl Pts',(14.7098797632094,14.1314716057908,2.84116666666655));
#27475=CARTESIAN_POINT('Ctrl Pts',(15.4999999999999,13.6752954743877,2.79949999999989));
#27476=CARTESIAN_POINT('Ctrl Pts',(16.2901202367903,14.1314716057908,2.75783333333322));
#27477=CARTESIAN_POINT('Ctrl Pts',(17.0802404735807,14.5876477371939,2.71616666666655));
#27478=CARTESIAN_POINT('Ctrl Pts',(17.0802404735807,15.5000000000002,2.67449999999989));
#27479=CARTESIAN_POINT('Ctrl Pts',(17.0802404735807,16.4123522628064,2.63283333333322));
#27480=CARTESIAN_POINT('Ctrl Pts',(16.2901202367902,16.8685283942095,2.59116666666655));
#27481=CARTESIAN_POINT('Ctrl Pts',(15.4999999999998,17.3247045256126,2.54949999999988));
#27482=CARTESIAN_POINT('Ctrl Pts',(14.7098797632094,16.8685283942095,2.50783333333322));
#27483=CARTESIAN_POINT('Ctrl Pts',(13.919759526419,16.4123522628064,2.46616666666655));
#27484=CARTESIAN_POINT('Ctrl Pts',(13.919759526419,15.5000000000001,2.42449999999988));
#27485=CARTESIAN_POINT('Ctrl Pts',(13.919759526419,14.5876477371939,2.38283333333321));
#27486=CARTESIAN_POINT('Ctrl Pts',(14.7098797632094,14.1314716057908,2.34116666666655));
#27487=CARTESIAN_POINT('Ctrl Pts',(15.4999999999999,13.6752954743877,2.29949999999988));
#27488=CARTESIAN_POINT('Ctrl Pts',(16.2901202367903,14.1314716057908,2.25783333333321));
#27489=CARTESIAN_POINT('Ctrl Pts',(17.0802404735807,14.5876477371939,2.21616666666655));
#27490=CARTESIAN_POINT('Ctrl Pts',(17.0802404735807,15.5000000000002,2.17449999999988));
#27491=CARTESIAN_POINT('Ctrl Pts',(17.0802404735807,16.4123522628064,2.13283333333321));
#27492=CARTESIAN_POINT('Ctrl Pts',(16.2901202367902,16.8685283942095,2.09116666666655));
#27493=CARTESIAN_POINT('Ctrl Pts',(15.4999999999998,17.3247045256126,2.04949999999988));
#27494=CARTESIAN_POINT('Ctrl Pts',(14.7098797632094,16.8685283942095,2.00783333333321));
#27495=CARTESIAN_POINT('Ctrl Pts',(13.919759526419,16.4123522628064,1.96616666666654));
#27496=CARTESIAN_POINT('Ctrl Pts',(13.919759526419,15.5000000000001,1.92449999999988));
#27497=CARTESIAN_POINT('Ctrl Pts',(13.919759526419,14.5876477371939,1.88283333333321));
#27498=CARTESIAN_POINT('Ctrl Pts',(14.7098797632094,14.1314716057908,1.84116666666654));
#27499=CARTESIAN_POINT('Ctrl Pts',(15.4999999999999,13.6752954743877,1.79949999999987));
#27500=CARTESIAN_POINT('Ctrl Pts',(16.2901202367903,14.1314716057908,1.75783333333321));
#27501=CARTESIAN_POINT('Ctrl Pts',(17.0802404735807,14.5876477371939,1.71616666666654));
#27502=CARTESIAN_POINT('Ctrl Pts',(17.0802404735807,15.5000000000002,1.67449999999987));
#27503=CARTESIAN_POINT('Ctrl Pts',(17.0802404735807,16.4123522628064,1.63283333333321));
#27504=CARTESIAN_POINT('Ctrl Pts',(16.2901202367902,16.8685283942095,1.59116666666654));
#27505=CARTESIAN_POINT('Ctrl Pts',(15.4999999999998,17.3247045256126,1.54949999999987));
#27506=CARTESIAN_POINT('Ctrl Pts',(14.7098797632094,16.8685283942095,1.5078333333332));
#27507=CARTESIAN_POINT('Ctrl Pts',(13.919759526419,16.4123522628064,1.46616666666654));
#27508=CARTESIAN_POINT('Ctrl Pts',(13.919759526419,15.5000000000001,1.42449999999987));
#27509=CARTESIAN_POINT('Ctrl Pts',(13.919759526419,14.5876477371939,1.3828333333332));
#27510=CARTESIAN_POINT('Ctrl Pts',(14.7098797632094,14.1314716057908,1.34116666666653));
#27511=CARTESIAN_POINT('Ctrl Pts',(15.4999999999999,13.6752954743877,1.29949999999987));
#27512=CARTESIAN_POINT('Ctrl Pts',(16.2901202367903,14.1314716057908,1.2578333333332));
#27513=CARTESIAN_POINT('Ctrl Pts',(17.0802404735807,14.5876477371939,1.21616666666653));
#27514=CARTESIAN_POINT('Ctrl Pts',(17.0802404735807,15.5000000000002,1.17449999999986));
#27515=CARTESIAN_POINT('Ctrl Pts',(17.0802404735807,16.4123522628064,1.1328333333332));
#27516=CARTESIAN_POINT('Ctrl Pts',(16.2901202367902,16.8685283942095,1.09116666666653));
#27517=CARTESIAN_POINT('Ctrl Pts',(15.4999999999998,17.3247045256126,1.04949999999987));
#27518=CARTESIAN_POINT('Ctrl Pts',(14.7098797632094,16.8685283942095,1.0078333333332));
#27519=CARTESIAN_POINT('Ctrl Pts',(13.919759526419,16.4123522628064,0.96616666666653));
#27520=CARTESIAN_POINT('Ctrl Pts',(13.919759526419,15.5000000000001,0.924499999999863));
#27521=CARTESIAN_POINT('Ctrl Pts',(13.919759526419,14.5876477371939,0.882833333333196));
#27522=CARTESIAN_POINT('Ctrl Pts',(14.7098797632094,14.1314716057908,0.841166666666529));
#27523=CARTESIAN_POINT('Ctrl Pts',(15.4999999999999,13.6752954743877,0.799499999999861));
#27524=CARTESIAN_POINT('Ctrl Pts',(16.2901202367903,14.1314716057908,0.757833333333194));
#27525=CARTESIAN_POINT('Ctrl Pts',(17.0802404735807,14.5876477371939,0.716166666666527));
#27526=CARTESIAN_POINT('Ctrl Pts',(17.0802404735807,15.5000000000002,0.674499999999859));
#27527=CARTESIAN_POINT('Ctrl Pts',(17.0802404735807,16.4123522628064,0.632833333333192));
#27528=CARTESIAN_POINT('Ctrl Pts',(16.2901202367902,16.8685283942095,0.591166666666525));
#27529=CARTESIAN_POINT('Ctrl Pts',(15.4999999999998,17.3247045256126,0.549499999999857));
#27530=CARTESIAN_POINT('Ctrl Pts',(14.7098797632094,16.8685283942095,0.50783333333319));
#27531=CARTESIAN_POINT('Ctrl Pts',(13.919759526419,16.4123522628064,0.466166666666523));
#27532=CARTESIAN_POINT('Ctrl Pts',(13.919759526419,15.5000000000001,0.424499999999856));
#27533=CARTESIAN_POINT('Ctrl Pts',(13.919759526419,14.5876477371939,0.382833333333188));
#27534=CARTESIAN_POINT('Ctrl Pts',(14.7098797632094,14.1314716057908,0.341166666666521));
#27535=CARTESIAN_POINT('Ctrl Pts',(15.4999999999999,13.6752954743877,0.299499999999854));
#27536=CARTESIAN_POINT('Ctrl Pts',(16.2901202367903,14.1314716057908,0.257833333333186));
#27537=CARTESIAN_POINT('Ctrl Pts',(17.0802404735807,14.5876477371939,0.216166666666519));
#27538=CARTESIAN_POINT('Ctrl Pts',(17.0802404735807,15.5000000000002,0.174499999999852));
#27539=CARTESIAN_POINT('Ctrl Pts',(17.0802404735807,16.4123522628064,0.132833333333185));
#27540=CARTESIAN_POINT('Ctrl Pts',(16.2901202367902,16.8685283942095,0.0911666666665173));
#27541=CARTESIAN_POINT('Ctrl Pts',(15.4999999999998,17.3247045256126,0.04949999999985));
#27542=CARTESIAN_POINT('Ctrl Pts',(14.7098797632094,16.8685283942095,0.00783333333318273));
#27543=CARTESIAN_POINT('Ctrl Pts',(13.919759526419,16.4123522628064,-0.0338333333334846));
#27544=CARTESIAN_POINT('Ctrl Pts',(13.919759526419,15.5000000000001,-0.0755000000001518));
#27545=CARTESIAN_POINT('Ctrl Pts',(13.919759526419,14.5876477371939,-0.117166666666817));
#27546=CARTESIAN_POINT('Ctrl Pts',(14.7098797632094,14.1314716057908,-0.158833333333485));
#27547=CARTESIAN_POINT('Ctrl Pts',(15.4999999999999,13.6752954743877,-0.200500000000152));
#27548=CARTESIAN_POINT('Ctrl Pts',(16.2901202367903,14.1314716057908,-0.242166666666819));
#27549=CARTESIAN_POINT('Ctrl Pts',(17.0802404735807,14.5876477371939,-0.283833333333487));
#27550=CARTESIAN_POINT('Ctrl Pts',(17.0802404735807,15.5000000000002,-0.325500000000154));
#27551=CARTESIAN_POINT('Ctrl Pts',(17.0802404735807,16.4123522628064,-0.367166666666821));
#27552=CARTESIAN_POINT('Ctrl Pts',(16.2901202367902,16.8685283942095,-0.408833333333488));
#27553=CARTESIAN_POINT('Ctrl Pts',(15.4999999999998,17.3247045256126,-0.450500000000156));
#27554=CARTESIAN_POINT('Ctrl Pts',(14.7098797632094,16.8685283942095,-0.492166666666823));
#27555=CARTESIAN_POINT('Ctrl Pts',(13.919759526419,16.4123522628064,-0.53383333333349));
#27556=CARTESIAN_POINT('Ctrl Pts',(13.919759526419,15.5000000000001,-0.575500000000157));
#27557=CARTESIAN_POINT('Ctrl Pts',(13.919759526419,14.5876477371939,-0.617166666666825));
#27558=CARTESIAN_POINT('Ctrl Pts',(14.7098797632094,14.1314716057908,-0.658833333333492));
#27559=CARTESIAN_POINT('Ctrl Pts',(15.4999999999999,13.6752954743877,-0.700500000000159));
#27560=CARTESIAN_POINT('Ctrl Pts',(16.2901202367903,14.1314716057908,-0.742166666666827));
#27561=CARTESIAN_POINT('Ctrl Pts',(17.0802404735807,14.5876477371939,-0.783833333333494));
#27562=CARTESIAN_POINT('Ctrl Pts',(17.0802404735807,15.5000000000002,-0.825500000000161));
#27563=CARTESIAN_POINT('Ctrl Pts',(17.0802404735807,16.4123522628064,-0.867166666666829));
#27564=CARTESIAN_POINT('Ctrl Pts',(16.2901202367902,16.8685283942095,-0.908833333333496));
#27565=CARTESIAN_POINT('Ctrl Pts',(15.4999999999998,17.3247045256126,-0.950500000000163));
#27566=CARTESIAN_POINT('Ctrl Pts',(14.7098797632094,16.8685283942095,-0.99216666666683));
#27567=CARTESIAN_POINT('Ctrl Pts',(13.919759526419,16.4123522628064,-1.0338333333335));
#27568=CARTESIAN_POINT('Ctrl Pts',(13.919759526419,15.5000000000001,-1.07550000000016));
#27569=CARTESIAN_POINT('Ctrl Pts',(13.919759526419,14.5876477371939,-1.11716666666683));
#27570=CARTESIAN_POINT('Ctrl Pts',(14.7098797632094,14.1314716057908,-1.1588333333335));
#27571=CARTESIAN_POINT('Ctrl Pts',(15.4999999999999,13.6752954743877,-1.20050000000017));
#27572=CARTESIAN_POINT('Ctrl Pts',(16.2901202367903,14.1314716057908,-1.24216666666683));
#27573=CARTESIAN_POINT('Ctrl Pts',(17.0802404735807,14.5876477371939,-1.2838333333335));
#27574=CARTESIAN_POINT('Ctrl Pts',(17.0802404735807,15.5000000000002,-1.32550000000017));
#27575=CARTESIAN_POINT('Ctrl Pts',(17.0802404735807,16.4123522628064,-1.36716666666683));
#27576=CARTESIAN_POINT('Ctrl Pts',(16.2901202367902,16.8685283942095,-1.4088333333335));
#27577=CARTESIAN_POINT('Ctrl Pts',(15.4999999999998,17.3247045256126,-1.45050000000017));
#27578=CARTESIAN_POINT('Ctrl Pts',(14.7098797632094,16.8685283942095,-1.49216666666684));
#27579=CARTESIAN_POINT('Ctrl Pts',(13.919759526419,16.4123522628064,-1.5338333333335));
#27580=CARTESIAN_POINT('Ctrl Pts',(13.919759526419,15.5000000000001,-1.57550000000017));
#27581=CARTESIAN_POINT('Ctrl Pts',(13.919759526419,14.5876477371939,-1.61716666666684));
#27582=CARTESIAN_POINT('Ctrl Pts',(14.7098797632094,14.1314716057908,-1.65883333333351));
#27583=CARTESIAN_POINT('Ctrl Pts',(15.4999999999999,13.6752954743877,-1.70050000000017));
#27584=CARTESIAN_POINT('Ctrl Pts',(16.2901202367903,14.1314716057908,-1.74216666666684));
#27585=CARTESIAN_POINT('Ctrl Pts',(17.0802404735807,14.5876477371939,-1.78383333333351));
#27586=CARTESIAN_POINT('Ctrl Pts',(17.0802404735807,15.5000000000002,-1.82550000000017));
#27587=CARTESIAN_POINT('Ctrl Pts',(17.0802404735807,16.4123522628064,-1.86716666666684));
#27588=CARTESIAN_POINT('Ctrl Pts',(16.2901202367902,16.8685283942095,-1.90883333333351));
#27589=CARTESIAN_POINT('Ctrl Pts',(15.4999999999998,17.3247045256126,-1.95050000000018));
#27590=CARTESIAN_POINT('Ctrl Pts',(14.7098797632094,16.8685283942095,-1.99216666666684));
#27591=CARTESIAN_POINT('Ctrl Pts',(14.4189900731848,16.7005831533693,-2.00750661517932));
#27592=CARTESIAN_POINT('Ctrl Pts',(14.2215542486878,16.4288360540163,-2.02512301646327));
#27593=CARTESIAN_POINT('',(13.9369173167912,16.6356236599185,-2.22824840486548));
#27594=CARTESIAN_POINT('Ctrl Pts',(17.4320632938681,15.5000000000002,11.440125));
#27595=CARTESIAN_POINT('Ctrl Pts',(17.4320632938681,16.6154772628064,11.3984583333333));
#27596=CARTESIAN_POINT('Ctrl Pts',(16.466031646934,17.1732158942095,11.3567916666667));
#27597=CARTESIAN_POINT('Ctrl Pts',(15.4999999999998,17.7309545256126,11.315125));
#27598=CARTESIAN_POINT('Ctrl Pts',(14.5339683530657,17.1732158942095,11.2734583333333));
#27599=CARTESIAN_POINT('Ctrl Pts',(13.5679367061316,16.6154772628064,11.2317916666667));
#27600=CARTESIAN_POINT('Ctrl Pts',(13.5679367061316,15.5000000000001,11.190125));
#27601=CARTESIAN_POINT('Ctrl Pts',(13.5679367061316,14.3845227371939,11.1484583333333));
#27602=CARTESIAN_POINT('Ctrl Pts',(14.5339683530657,13.8267841057908,11.1067916666667));
#27603=CARTESIAN_POINT('Ctrl Pts',(15.4999999999999,13.2690454743877,11.065125));
#27604=CARTESIAN_POINT('Ctrl Pts',(16.466031646934,13.8267841057908,11.0234583333333));
#27605=CARTESIAN_POINT('Ctrl Pts',(17.4320632938681,14.3845227371939,10.9817916666667));
#27606=CARTESIAN_POINT('Ctrl Pts',(17.4320632938681,15.5000000000002,10.940125));
#27607=CARTESIAN_POINT('Ctrl Pts',(17.4320632938681,16.6154772628064,10.8984583333333));
#27608=CARTESIAN_POINT('Ctrl Pts',(16.466031646934,17.1732158942095,10.8567916666667));
#27609=CARTESIAN_POINT('Ctrl Pts',(15.4999999999998,17.7309545256126,10.815125));
#27610=CARTESIAN_POINT('Ctrl Pts',(14.5339683530657,17.1732158942095,10.7734583333333));
#27611=CARTESIAN_POINT('Ctrl Pts',(13.5679367061316,16.6154772628064,10.7317916666667));
#27612=CARTESIAN_POINT('Ctrl Pts',(13.5679367061316,15.5000000000001,10.690125));
#27613=CARTESIAN_POINT('Ctrl Pts',(13.5679367061316,14.3845227371939,10.6484583333333));
#27614=CARTESIAN_POINT('Ctrl Pts',(14.5339683530657,13.8267841057908,10.6067916666667));
#27615=CARTESIAN_POINT('Ctrl Pts',(15.4999999999999,13.2690454743877,10.565125));
#27616=CARTESIAN_POINT('Ctrl Pts',(16.466031646934,13.8267841057908,10.5234583333333));
#27617=CARTESIAN_POINT('Ctrl Pts',(17.4320632938681,14.3845227371939,10.4817916666667));
#27618=CARTESIAN_POINT('Ctrl Pts',(17.4320632938681,15.5000000000002,10.440125));
#27619=CARTESIAN_POINT('Ctrl Pts',(17.4320632938681,16.6154772628064,10.3984583333333));
#27620=CARTESIAN_POINT('Ctrl Pts',(16.466031646934,17.1732158942095,10.3567916666667));
#27621=CARTESIAN_POINT('Ctrl Pts',(15.4999999999998,17.7309545256126,10.315125));
#27622=CARTESIAN_POINT('Ctrl Pts',(14.5339683530657,17.1732158942095,10.2734583333333));
#27623=CARTESIAN_POINT('Ctrl Pts',(13.5679367061316,16.6154772628064,10.2317916666667));
#27624=CARTESIAN_POINT('Ctrl Pts',(13.5679367061316,15.5000000000001,10.190125));
#27625=CARTESIAN_POINT('Ctrl Pts',(13.5679367061316,14.3845227371939,10.1484583333333));
#27626=CARTESIAN_POINT('Ctrl Pts',(14.5339683530657,13.8267841057908,10.1067916666666));
#27627=CARTESIAN_POINT('Ctrl Pts',(15.4999999999999,13.2690454743877,10.065125));
#27628=CARTESIAN_POINT('Ctrl Pts',(16.466031646934,13.8267841057908,10.0234583333333));
#27629=CARTESIAN_POINT('Ctrl Pts',(17.4320632938681,14.3845227371939,9.98179166666664));
#27630=CARTESIAN_POINT('Ctrl Pts',(17.4320632938681,15.5000000000002,9.94012499999998));
#27631=CARTESIAN_POINT('Ctrl Pts',(17.4320632938681,16.6154772628064,9.89845833333331));
#27632=CARTESIAN_POINT('Ctrl Pts',(16.466031646934,17.1732158942095,9.85679166666664));
#27633=CARTESIAN_POINT('Ctrl Pts',(15.4999999999998,17.7309545256126,9.81512499999998));
#27634=CARTESIAN_POINT('Ctrl Pts',(14.5339683530657,17.1732158942095,9.77345833333331));
#27635=CARTESIAN_POINT('Ctrl Pts',(13.5679367061316,16.6154772628064,9.73179166666664));
#27636=CARTESIAN_POINT('Ctrl Pts',(13.5679367061316,15.5000000000001,9.69012499999998));
#27637=CARTESIAN_POINT('Ctrl Pts',(13.5679367061316,14.3845227371939,9.64845833333331));
#27638=CARTESIAN_POINT('Ctrl Pts',(14.5339683530657,13.8267841057908,9.60679166666664));
#27639=CARTESIAN_POINT('Ctrl Pts',(15.4999999999999,13.2690454743877,9.56512499999998));
#27640=CARTESIAN_POINT('Ctrl Pts',(16.466031646934,13.8267841057908,9.52345833333331));
#27641=CARTESIAN_POINT('Ctrl Pts',(17.4320632938681,14.3845227371939,9.48179166666664));
#27642=CARTESIAN_POINT('Ctrl Pts',(17.4320632938681,15.5000000000002,9.44012499999997));
#27643=CARTESIAN_POINT('Ctrl Pts',(17.4320632938681,16.6154772628064,9.39845833333331));
#27644=CARTESIAN_POINT('Ctrl Pts',(16.466031646934,17.1732158942095,9.35679166666664));
#27645=CARTESIAN_POINT('Ctrl Pts',(15.4999999999998,17.7309545256126,9.31512499999997));
#27646=CARTESIAN_POINT('Ctrl Pts',(14.5339683530657,17.1732158942095,9.2734583333333));
#27647=CARTESIAN_POINT('Ctrl Pts',(13.5679367061316,16.6154772628064,9.23179166666664));
#27648=CARTESIAN_POINT('Ctrl Pts',(13.5679367061316,15.5000000000001,9.19012499999997));
#27649=CARTESIAN_POINT('Ctrl Pts',(13.5679367061316,14.3845227371939,9.1484583333333));
#27650=CARTESIAN_POINT('Ctrl Pts',(14.5339683530657,13.8267841057908,9.10679166666664));
#27651=CARTESIAN_POINT('Ctrl Pts',(15.4999999999999,13.2690454743877,9.06512499999997));
#27652=CARTESIAN_POINT('Ctrl Pts',(16.466031646934,13.8267841057908,9.0234583333333));
#27653=CARTESIAN_POINT('Ctrl Pts',(17.4320632938681,14.3845227371939,8.98179166666663));
#27654=CARTESIAN_POINT('Ctrl Pts',(17.4320632938681,15.5000000000002,8.94012499999997));
#27655=CARTESIAN_POINT('Ctrl Pts',(17.4320632938681,16.6154772628064,8.8984583333333));
#27656=CARTESIAN_POINT('Ctrl Pts',(16.466031646934,17.1732158942095,8.85679166666663));
#27657=CARTESIAN_POINT('Ctrl Pts',(15.4999999999998,17.7309545256126,8.81512499999996));
#27658=CARTESIAN_POINT('Ctrl Pts',(14.5339683530657,17.1732158942095,8.7734583333333));
#27659=CARTESIAN_POINT('Ctrl Pts',(13.5679367061316,16.6154772628064,8.73179166666663));
#27660=CARTESIAN_POINT('Ctrl Pts',(13.5679367061316,15.5000000000001,8.69012499999996));
#27661=CARTESIAN_POINT('Ctrl Pts',(13.5679367061316,14.3845227371939,8.64845833333329));
#27662=CARTESIAN_POINT('Ctrl Pts',(14.5339683530657,13.8267841057908,8.60679166666663));
#27663=CARTESIAN_POINT('Ctrl Pts',(15.4999999999999,13.2690454743877,8.56512499999996));
#27664=CARTESIAN_POINT('Ctrl Pts',(16.466031646934,13.8267841057908,8.52345833333329));
#27665=CARTESIAN_POINT('Ctrl Pts',(17.4320632938681,14.3845227371939,8.48179166666663));
#27666=CARTESIAN_POINT('Ctrl Pts',(17.4320632938681,15.5000000000002,8.44012499999996));
#27667=CARTESIAN_POINT('Ctrl Pts',(17.4320632938681,16.6154772628064,8.39845833333329));
#27668=CARTESIAN_POINT('Ctrl Pts',(16.466031646934,17.1732158942095,8.35679166666662));
#27669=CARTESIAN_POINT('Ctrl Pts',(15.4999999999998,17.7309545256126,8.31512499999996));
#27670=CARTESIAN_POINT('Ctrl Pts',(14.5339683530657,17.1732158942095,8.27345833333329));
#27671=CARTESIAN_POINT('Ctrl Pts',(13.5679367061316,16.6154772628064,8.23179166666662));
#27672=CARTESIAN_POINT('Ctrl Pts',(13.5679367061316,15.5000000000001,8.19012499999996));
#27673=CARTESIAN_POINT('Ctrl Pts',(13.5679367061316,14.3845227371939,8.14845833333329));
#27674=CARTESIAN_POINT('Ctrl Pts',(14.5339683530657,13.8267841057908,8.10679166666662));
#27675=CARTESIAN_POINT('Ctrl Pts',(15.4999999999999,13.2690454743877,8.06512499999995));
#27676=CARTESIAN_POINT('Ctrl Pts',(16.466031646934,13.8267841057908,8.02345833333329));
#27677=CARTESIAN_POINT('Ctrl Pts',(17.4320632938681,14.3845227371939,7.98179166666662));
#27678=CARTESIAN_POINT('Ctrl Pts',(17.4320632938681,15.5000000000002,7.94012499999995));
#27679=CARTESIAN_POINT('Ctrl Pts',(17.4320632938681,16.6154772628064,7.89845833333329));
#27680=CARTESIAN_POINT('Ctrl Pts',(16.466031646934,17.1732158942095,7.85679166666662));
#27681=CARTESIAN_POINT('Ctrl Pts',(15.4999999999998,17.7309545256126,7.81512499999995));
#27682=CARTESIAN_POINT('Ctrl Pts',(14.5339683530657,17.1732158942095,7.77345833333328));
#27683=CARTESIAN_POINT('Ctrl Pts',(13.5679367061316,16.6154772628064,7.73179166666662));
#27684=CARTESIAN_POINT('Ctrl Pts',(13.5679367061316,15.5000000000001,7.69012499999995));
#27685=CARTESIAN_POINT('Ctrl Pts',(13.5679367061316,14.3845227371939,7.64845833333328));
#27686=CARTESIAN_POINT('Ctrl Pts',(14.5339683530657,13.8267841057908,7.60679166666661));
#27687=CARTESIAN_POINT('Ctrl Pts',(15.4999999999999,13.2690454743877,7.56512499999995));
#27688=CARTESIAN_POINT('Ctrl Pts',(16.466031646934,13.8267841057908,7.52345833333328));
#27689=CARTESIAN_POINT('Ctrl Pts',(17.4320632938681,14.3845227371939,7.48179166666661));
#27690=CARTESIAN_POINT('Ctrl Pts',(17.4320632938681,15.5000000000002,7.44012499999995));
#27691=CARTESIAN_POINT('Ctrl Pts',(17.4320632938681,16.6154772628064,7.39845833333328));
#27692=CARTESIAN_POINT('Ctrl Pts',(16.466031646934,17.1732158942095,7.35679166666661));
#27693=CARTESIAN_POINT('Ctrl Pts',(15.4999999999998,17.7309545256126,7.31512499999995));
#27694=CARTESIAN_POINT('Ctrl Pts',(14.5339683530657,17.1732158942095,7.27345833333328));
#27695=CARTESIAN_POINT('Ctrl Pts',(13.5679367061316,16.6154772628064,7.23179166666661));
#27696=CARTESIAN_POINT('Ctrl Pts',(13.5679367061316,15.5000000000001,7.19012499999994));
#27697=CARTESIAN_POINT('Ctrl Pts',(13.5679367061316,14.3845227371939,7.14845833333328));
#27698=CARTESIAN_POINT('Ctrl Pts',(14.5339683530657,13.8267841057908,7.10679166666661));
#27699=CARTESIAN_POINT('Ctrl Pts',(15.4999999999999,13.2690454743877,7.06512499999994));
#27700=CARTESIAN_POINT('Ctrl Pts',(16.466031646934,13.8267841057908,7.02345833333327));
#27701=CARTESIAN_POINT('Ctrl Pts',(17.4320632938681,14.3845227371939,6.98179166666661));
#27702=CARTESIAN_POINT('Ctrl Pts',(17.4320632938681,15.5000000000002,6.94012499999994));
#27703=CARTESIAN_POINT('Ctrl Pts',(17.4320632938681,16.6154772628064,6.89845833333327));
#27704=CARTESIAN_POINT('Ctrl Pts',(16.466031646934,17.1732158942095,6.8567916666666));
#27705=CARTESIAN_POINT('Ctrl Pts',(15.4999999999998,17.7309545256126,6.81512499999994));
#27706=CARTESIAN_POINT('Ctrl Pts',(14.5339683530657,17.1732158942095,6.77345833333327));
#27707=CARTESIAN_POINT('Ctrl Pts',(13.5679367061316,16.6154772628064,6.7317916666666));
#27708=CARTESIAN_POINT('Ctrl Pts',(13.5679367061316,15.5000000000001,6.69012499999994));
#27709=CARTESIAN_POINT('Ctrl Pts',(13.5679367061316,14.3845227371939,6.64845833333327));
#27710=CARTESIAN_POINT('Ctrl Pts',(14.5339683530657,13.8267841057908,6.6067916666666));
#27711=CARTESIAN_POINT('Ctrl Pts',(15.4999999999999,13.2690454743877,6.56512499999993));
#27712=CARTESIAN_POINT('Ctrl Pts',(16.466031646934,13.8267841057908,6.52345833333327));
#27713=CARTESIAN_POINT('Ctrl Pts',(17.4320632938681,14.3845227371939,6.4817916666666));
#27714=CARTESIAN_POINT('Ctrl Pts',(17.4320632938681,15.5000000000002,6.44012499999993));
#27715=CARTESIAN_POINT('Ctrl Pts',(17.4320632938681,16.6154772628064,6.39845833333327));
#27716=CARTESIAN_POINT('Ctrl Pts',(16.466031646934,17.1732158942095,6.3567916666666));
#27717=CARTESIAN_POINT('Ctrl Pts',(15.4999999999998,17.7309545256126,6.31512499999993));
#27718=CARTESIAN_POINT('Ctrl Pts',(14.5339683530657,17.1732158942095,6.27345833333326));
#27719=CARTESIAN_POINT('Ctrl Pts',(13.5679367061316,16.6154772628064,6.2317916666666));
#27720=CARTESIAN_POINT('Ctrl Pts',(13.5679367061316,15.5000000000001,6.19012499999993));
#27721=CARTESIAN_POINT('Ctrl Pts',(13.5679367061316,14.3845227371939,6.14845833333326));
#27722=CARTESIAN_POINT('Ctrl Pts',(14.5339683530657,13.8267841057908,6.10679166666659));
#27723=CARTESIAN_POINT('Ctrl Pts',(15.4999999999999,13.2690454743877,6.06512499999993));
#27724=CARTESIAN_POINT('Ctrl Pts',(16.466031646934,13.8267841057908,6.02345833333326));
#27725=CARTESIAN_POINT('Ctrl Pts',(17.4320632938681,14.3845227371939,5.98179166666659));
#27726=CARTESIAN_POINT('Ctrl Pts',(17.4320632938681,15.5000000000002,5.94012499999993));
#27727=CARTESIAN_POINT('Ctrl Pts',(17.4320632938681,16.6154772628064,5.89845833333326));
#27728=CARTESIAN_POINT('Ctrl Pts',(16.466031646934,17.1732158942095,5.85679166666659));
#27729=CARTESIAN_POINT('Ctrl Pts',(15.4999999999998,17.7309545256126,5.81512499999992));
#27730=CARTESIAN_POINT('Ctrl Pts',(14.5339683530657,17.1732158942095,5.77345833333326));
#27731=CARTESIAN_POINT('Ctrl Pts',(13.5679367061316,16.6154772628064,5.73179166666659));
#27732=CARTESIAN_POINT('Ctrl Pts',(13.5679367061316,15.5000000000001,5.69012499999992));
#27733=CARTESIAN_POINT('Ctrl Pts',(13.5679367061316,14.3845227371939,5.64845833333326));
#27734=CARTESIAN_POINT('Ctrl Pts',(14.5339683530657,13.8267841057908,5.60679166666659));
#27735=CARTESIAN_POINT('Ctrl Pts',(15.4999999999999,13.2690454743877,5.56512499999992));
#27736=CARTESIAN_POINT('Ctrl Pts',(16.466031646934,13.8267841057908,5.52345833333325));
#27737=CARTESIAN_POINT('Ctrl Pts',(17.4320632938681,14.3845227371939,5.48179166666659));
#27738=CARTESIAN_POINT('Ctrl Pts',(17.4320632938681,15.5000000000002,5.44012499999992));
#27739=CARTESIAN_POINT('Ctrl Pts',(17.4320632938681,16.6154772628064,5.39845833333325));
#27740=CARTESIAN_POINT('Ctrl Pts',(16.466031646934,17.1732158942095,5.35679166666658));
#27741=CARTESIAN_POINT('Ctrl Pts',(15.4999999999998,17.7309545256126,5.31512499999992));
#27742=CARTESIAN_POINT('Ctrl Pts',(14.5339683530657,17.1732158942095,5.27345833333325));
#27743=CARTESIAN_POINT('Ctrl Pts',(13.5679367061316,16.6154772628064,5.23179166666658));
#27744=CARTESIAN_POINT('Ctrl Pts',(13.5679367061316,15.5000000000001,5.19012499999992));
#27745=CARTESIAN_POINT('Ctrl Pts',(13.5679367061316,14.3845227371939,5.14845833333325));
#27746=CARTESIAN_POINT('Ctrl Pts',(14.5339683530657,13.8267841057908,5.10679166666658));
#27747=CARTESIAN_POINT('Ctrl Pts',(15.4999999999999,13.2690454743877,5.06512499999991));
#27748=CARTESIAN_POINT('Ctrl Pts',(16.466031646934,13.8267841057908,5.02345833333325));
#27749=CARTESIAN_POINT('Ctrl Pts',(17.4320632938681,14.3845227371939,4.98179166666658));
#27750=CARTESIAN_POINT('Ctrl Pts',(17.4320632938681,15.5000000000002,4.94012499999991));
#27751=CARTESIAN_POINT('Ctrl Pts',(17.4320632938681,16.6154772628064,4.89845833333325));
#27752=CARTESIAN_POINT('Ctrl Pts',(16.466031646934,17.1732158942095,4.85679166666658));
#27753=CARTESIAN_POINT('Ctrl Pts',(15.4999999999998,17.7309545256126,4.81512499999991));
#27754=CARTESIAN_POINT('Ctrl Pts',(14.5339683530657,17.1732158942095,4.77345833333324));
#27755=CARTESIAN_POINT('Ctrl Pts',(13.5679367061316,16.6154772628064,4.73179166666658));
#27756=CARTESIAN_POINT('Ctrl Pts',(13.5679367061316,15.5000000000001,4.69012499999991));
#27757=CARTESIAN_POINT('Ctrl Pts',(13.5679367061316,14.3845227371939,4.64845833333324));
#27758=CARTESIAN_POINT('Ctrl Pts',(14.5339683530657,13.8267841057908,4.60679166666657));
#27759=CARTESIAN_POINT('Ctrl Pts',(15.4999999999999,13.2690454743877,4.56512499999991));
#27760=CARTESIAN_POINT('Ctrl Pts',(16.466031646934,13.8267841057908,4.52345833333324));
#27761=CARTESIAN_POINT('Ctrl Pts',(17.4320632938681,14.3845227371939,4.48179166666657));
#27762=CARTESIAN_POINT('Ctrl Pts',(17.4320632938681,15.5000000000002,4.44012499999991));
#27763=CARTESIAN_POINT('Ctrl Pts',(17.4320632938681,16.6154772628064,4.39845833333324));
#27764=CARTESIAN_POINT('Ctrl Pts',(16.466031646934,17.1732158942095,4.35679166666657));
#27765=CARTESIAN_POINT('Ctrl Pts',(15.4999999999998,17.7309545256126,4.31512499999991));
#27766=CARTESIAN_POINT('Ctrl Pts',(14.5339683530657,17.1732158942095,4.27345833333324));
#27767=CARTESIAN_POINT('Ctrl Pts',(13.5679367061316,16.6154772628064,4.23179166666657));
#27768=CARTESIAN_POINT('Ctrl Pts',(13.5679367061316,15.5000000000001,4.1901249999999));
#27769=CARTESIAN_POINT('Ctrl Pts',(13.5679367061316,14.3845227371939,4.14845833333324));
#27770=CARTESIAN_POINT('Ctrl Pts',(14.5339683530657,13.8267841057908,4.10679166666657));
#27771=CARTESIAN_POINT('Ctrl Pts',(15.4999999999999,13.2690454743877,4.0651249999999));
#27772=CARTESIAN_POINT('Ctrl Pts',(16.466031646934,13.8267841057908,4.02345833333323));
#27773=CARTESIAN_POINT('Ctrl Pts',(17.4320632938681,14.3845227371939,3.98179166666657));
#27774=CARTESIAN_POINT('Ctrl Pts',(17.4320632938681,15.5000000000002,3.9401249999999));
#27775=CARTESIAN_POINT('Ctrl Pts',(17.4320632938681,16.6154772628064,3.89845833333323));
#27776=CARTESIAN_POINT('Ctrl Pts',(16.466031646934,17.1732158942095,3.85679166666657));
#27777=CARTESIAN_POINT('Ctrl Pts',(15.4999999999998,17.7309545256126,3.8151249999999));
#27778=CARTESIAN_POINT('Ctrl Pts',(14.5339683530657,17.1732158942095,3.77345833333323));
#27779=CARTESIAN_POINT('Ctrl Pts',(13.5679367061316,16.6154772628064,3.73179166666656));
#27780=CARTESIAN_POINT('Ctrl Pts',(13.5679367061316,15.5000000000001,3.6901249999999));
#27781=CARTESIAN_POINT('Ctrl Pts',(13.5679367061316,14.3845227371939,3.64845833333323));
#27782=CARTESIAN_POINT('Ctrl Pts',(14.5339683530657,13.8267841057908,3.60679166666656));
#27783=CARTESIAN_POINT('Ctrl Pts',(15.4999999999999,13.2690454743877,3.5651249999999));
#27784=CARTESIAN_POINT('Ctrl Pts',(16.466031646934,13.8267841057908,3.52345833333323));
#27785=CARTESIAN_POINT('Ctrl Pts',(17.4320632938681,14.3845227371939,3.48179166666656));
#27786=CARTESIAN_POINT('Ctrl Pts',(17.4320632938681,15.5000000000002,3.44012499999989));
#27787=CARTESIAN_POINT('Ctrl Pts',(17.4320632938681,16.6154772628064,3.39845833333323));
#27788=CARTESIAN_POINT('Ctrl Pts',(16.466031646934,17.1732158942095,3.35679166666656));
#27789=CARTESIAN_POINT('Ctrl Pts',(15.4999999999998,17.7309545256126,3.31512499999989));
#27790=CARTESIAN_POINT('Ctrl Pts',(14.5339683530657,17.1732158942095,3.27345833333322));
#27791=CARTESIAN_POINT('Ctrl Pts',(13.5679367061316,16.6154772628064,3.23179166666656));
#27792=CARTESIAN_POINT('Ctrl Pts',(13.5679367061316,15.5000000000001,3.19012499999989));
#27793=CARTESIAN_POINT('Ctrl Pts',(13.5679367061316,14.3845227371939,3.14845833333322));
#27794=CARTESIAN_POINT('Ctrl Pts',(14.5339683530657,13.8267841057908,3.10679166666655));
#27795=CARTESIAN_POINT('Ctrl Pts',(15.4999999999999,13.2690454743877,3.06512499999989));
#27796=CARTESIAN_POINT('Ctrl Pts',(16.466031646934,13.8267841057908,3.02345833333322));
#27797=CARTESIAN_POINT('Ctrl Pts',(17.4320632938681,14.3845227371939,2.98179166666655));
#27798=CARTESIAN_POINT('Ctrl Pts',(17.4320632938681,15.5000000000002,2.94012499999989));
#27799=CARTESIAN_POINT('Ctrl Pts',(17.4320632938681,16.6154772628064,2.89845833333322));
#27800=CARTESIAN_POINT('Ctrl Pts',(16.466031646934,17.1732158942095,2.85679166666655));
#27801=CARTESIAN_POINT('Ctrl Pts',(15.4999999999998,17.7309545256126,2.81512499999988));
#27802=CARTESIAN_POINT('Ctrl Pts',(14.5339683530657,17.1732158942095,2.77345833333322));
#27803=CARTESIAN_POINT('Ctrl Pts',(13.5679367061316,16.6154772628064,2.73179166666655));
#27804=CARTESIAN_POINT('Ctrl Pts',(13.5679367061316,15.5000000000001,2.69012499999988));
#27805=CARTESIAN_POINT('Ctrl Pts',(13.5679367061316,14.3845227371939,2.64845833333321));
#27806=CARTESIAN_POINT('Ctrl Pts',(14.5339683530657,13.8267841057908,2.60679166666655));
#27807=CARTESIAN_POINT('Ctrl Pts',(15.4999999999999,13.2690454743877,2.56512499999988));
#27808=CARTESIAN_POINT('Ctrl Pts',(16.466031646934,13.8267841057908,2.52345833333321));
#27809=CARTESIAN_POINT('Ctrl Pts',(17.4320632938681,14.3845227371939,2.48179166666655));
#27810=CARTESIAN_POINT('Ctrl Pts',(17.4320632938681,15.5000000000002,2.44012499999988));
#27811=CARTESIAN_POINT('Ctrl Pts',(17.4320632938681,16.6154772628064,2.39845833333321));
#27812=CARTESIAN_POINT('Ctrl Pts',(16.466031646934,17.1732158942095,2.35679166666655));
#27813=CARTESIAN_POINT('Ctrl Pts',(15.4999999999998,17.7309545256126,2.31512499999988));
#27814=CARTESIAN_POINT('Ctrl Pts',(14.5339683530657,17.1732158942095,2.27345833333321));
#27815=CARTESIAN_POINT('Ctrl Pts',(13.5679367061316,16.6154772628064,2.23179166666654));
#27816=CARTESIAN_POINT('Ctrl Pts',(13.5679367061316,15.5000000000001,2.19012499999988));
#27817=CARTESIAN_POINT('Ctrl Pts',(13.5679367061316,14.3845227371939,2.14845833333321));
#27818=CARTESIAN_POINT('Ctrl Pts',(14.5339683530657,13.8267841057908,2.10679166666654));
#27819=CARTESIAN_POINT('Ctrl Pts',(15.4999999999999,13.2690454743877,2.06512499999987));
#27820=CARTESIAN_POINT('Ctrl Pts',(16.466031646934,13.8267841057908,2.02345833333321));
#27821=CARTESIAN_POINT('Ctrl Pts',(17.4320632938681,14.3845227371939,1.98179166666654));
#27822=CARTESIAN_POINT('Ctrl Pts',(17.4320632938681,15.5000000000002,1.94012499999987));
#27823=CARTESIAN_POINT('Ctrl Pts',(17.4320632938681,16.6154772628064,1.89845833333321));
#27824=CARTESIAN_POINT('Ctrl Pts',(16.466031646934,17.1732158942095,1.85679166666654));
#27825=CARTESIAN_POINT('Ctrl Pts',(15.4999999999998,17.7309545256126,1.81512499999987));
#27826=CARTESIAN_POINT('Ctrl Pts',(14.5339683530657,17.1732158942095,1.7734583333332));
#27827=CARTESIAN_POINT('Ctrl Pts',(13.5679367061316,16.6154772628064,1.73179166666654));
#27828=CARTESIAN_POINT('Ctrl Pts',(13.5679367061316,15.5000000000001,1.69012499999987));
#27829=CARTESIAN_POINT('Ctrl Pts',(13.5679367061316,14.3845227371939,1.6484583333332));
#27830=CARTESIAN_POINT('Ctrl Pts',(14.5339683530657,13.8267841057908,1.60679166666653));
#27831=CARTESIAN_POINT('Ctrl Pts',(15.4999999999999,13.2690454743877,1.56512499999987));
#27832=CARTESIAN_POINT('Ctrl Pts',(16.466031646934,13.8267841057908,1.5234583333332));
#27833=CARTESIAN_POINT('Ctrl Pts',(17.4320632938681,14.3845227371939,1.48179166666653));
#27834=CARTESIAN_POINT('Ctrl Pts',(17.4320632938681,15.5000000000002,1.44012499999987));
#27835=CARTESIAN_POINT('Ctrl Pts',(17.4320632938681,16.6154772628064,1.3984583333332));
#27836=CARTESIAN_POINT('Ctrl Pts',(16.466031646934,17.1732158942095,1.35679166666653));
#27837=CARTESIAN_POINT('Ctrl Pts',(15.4999999999998,17.7309545256126,1.31512499999987));
#27838=CARTESIAN_POINT('Ctrl Pts',(14.5339683530657,17.1732158942095,1.2734583333332));
#27839=CARTESIAN_POINT('Ctrl Pts',(13.5679367061316,16.6154772628064,1.23179166666653));
#27840=CARTESIAN_POINT('Ctrl Pts',(13.5679367061316,15.5000000000001,1.19012499999986));
#27841=CARTESIAN_POINT('Ctrl Pts',(13.5679367061316,14.3845227371939,1.1484583333332));
#27842=CARTESIAN_POINT('Ctrl Pts',(14.5339683530657,13.8267841057908,1.10679166666653));
#27843=CARTESIAN_POINT('Ctrl Pts',(15.4999999999999,13.2690454743877,1.06512499999986));
#27844=CARTESIAN_POINT('Ctrl Pts',(16.466031646934,13.8267841057908,1.02345833333319));
#27845=CARTESIAN_POINT('Ctrl Pts',(17.4320632938681,14.3845227371939,0.981791666666527));
#27846=CARTESIAN_POINT('Ctrl Pts',(17.4320632938681,15.5000000000002,0.94012499999986));
#27847=CARTESIAN_POINT('Ctrl Pts',(17.4320632938681,16.6154772628064,0.898458333333192));
#27848=CARTESIAN_POINT('Ctrl Pts',(16.466031646934,17.1732158942095,0.856791666666525));
#27849=CARTESIAN_POINT('Ctrl Pts',(15.4999999999998,17.7309545256126,0.815124999999858));
#27850=CARTESIAN_POINT('Ctrl Pts',(14.5339683530657,17.1732158942095,0.77345833333319));
#27851=CARTESIAN_POINT('Ctrl Pts',(13.5679367061316,16.6154772628064,0.731791666666523));
#27852=CARTESIAN_POINT('Ctrl Pts',(13.5679367061316,15.5000000000001,0.690124999999856));
#27853=CARTESIAN_POINT('Ctrl Pts',(13.5679367061316,14.3845227371939,0.648458333333188));
#27854=CARTESIAN_POINT('Ctrl Pts',(14.5339683530657,13.8267841057908,0.606791666666521));
#27855=CARTESIAN_POINT('Ctrl Pts',(15.4999999999999,13.2690454743877,0.565124999999854));
#27856=CARTESIAN_POINT('Ctrl Pts',(16.466031646934,13.8267841057908,0.523458333333187));
#27857=CARTESIAN_POINT('Ctrl Pts',(17.4320632938681,14.3845227371939,0.481791666666519));
#27858=CARTESIAN_POINT('Ctrl Pts',(17.4320632938681,15.5000000000002,0.440124999999852));
#27859=CARTESIAN_POINT('Ctrl Pts',(17.4320632938681,16.6154772628064,0.398458333333185));
#27860=CARTESIAN_POINT('Ctrl Pts',(16.466031646934,17.1732158942095,0.356791666666518));
#27861=CARTESIAN_POINT('Ctrl Pts',(15.4999999999998,17.7309545256126,0.31512499999985));
#27862=CARTESIAN_POINT('Ctrl Pts',(14.5339683530657,17.1732158942095,0.273458333333183));
#27863=CARTESIAN_POINT('Ctrl Pts',(13.5679367061316,16.6154772628064,0.231791666666516));
#27864=CARTESIAN_POINT('Ctrl Pts',(13.5679367061316,15.5000000000001,0.190124999999848));
#27865=CARTESIAN_POINT('Ctrl Pts',(13.5679367061316,14.3845227371939,0.148458333333183));
#27866=CARTESIAN_POINT('Ctrl Pts',(14.5339683530657,13.8267841057908,0.106791666666516));
#27867=CARTESIAN_POINT('Ctrl Pts',(15.4999999999999,13.2690454743877,0.0651249999998483));
#27868=CARTESIAN_POINT('Ctrl Pts',(16.466031646934,13.8267841057908,0.023458333333181));
#27869=CARTESIAN_POINT('Ctrl Pts',(17.4320632938681,14.3845227371939,-0.0182083333334863));
#27870=CARTESIAN_POINT('Ctrl Pts',(17.4320632938681,15.5000000000002,-0.0598750000001536));
#27871=CARTESIAN_POINT('Ctrl Pts',(17.4320632938681,16.6154772628064,-0.101541666666821));
#27872=CARTESIAN_POINT('Ctrl Pts',(16.466031646934,17.1732158942095,-0.143208333333488));
#27873=CARTESIAN_POINT('Ctrl Pts',(15.4999999999998,17.7309545256126,-0.184875000000155));
#27874=CARTESIAN_POINT('Ctrl Pts',(14.5339683530657,17.1732158942095,-0.226541666666823));
#27875=CARTESIAN_POINT('Ctrl Pts',(13.5679367061316,16.6154772628064,-0.26820833333349));
#27876=CARTESIAN_POINT('Ctrl Pts',(13.5679367061316,15.5000000000001,-0.309875000000157));
#27877=CARTESIAN_POINT('Ctrl Pts',(13.5679367061316,14.3845227371939,-0.351541666666825));
#27878=CARTESIAN_POINT('Ctrl Pts',(14.5339683530657,13.8267841057908,-0.393208333333492));
#27879=CARTESIAN_POINT('Ctrl Pts',(15.4999999999999,13.2690454743877,-0.434875000000159));
#27880=CARTESIAN_POINT('Ctrl Pts',(16.466031646934,13.8267841057908,-0.476541666666826));
#27881=CARTESIAN_POINT('Ctrl Pts',(17.4320632938681,14.3845227371939,-0.518208333333494));
#27882=CARTESIAN_POINT('Ctrl Pts',(17.4320632938681,15.5000000000002,-0.559875000000161));
#27883=CARTESIAN_POINT('Ctrl Pts',(17.4320632938681,16.6154772628064,-0.601541666666828));
#27884=CARTESIAN_POINT('Ctrl Pts',(16.466031646934,17.1732158942095,-0.643208333333495));
#27885=CARTESIAN_POINT('Ctrl Pts',(15.4999999999998,17.7309545256126,-0.684875000000163));
#27886=CARTESIAN_POINT('Ctrl Pts',(14.5339683530657,17.1732158942095,-0.72654166666683));
#27887=CARTESIAN_POINT('Ctrl Pts',(13.5679367061316,16.6154772628064,-0.768208333333497));
#27888=CARTESIAN_POINT('Ctrl Pts',(13.5679367061316,15.5000000000001,-0.809875000000165));
#27889=CARTESIAN_POINT('Ctrl Pts',(13.5679367061316,14.3845227371939,-0.851541666666832));
#27890=CARTESIAN_POINT('Ctrl Pts',(14.5339683530657,13.8267841057908,-0.893208333333499));
#27891=CARTESIAN_POINT('Ctrl Pts',(15.4999999999999,13.2690454743877,-0.934875000000167));
#27892=CARTESIAN_POINT('Ctrl Pts',(16.466031646934,13.8267841057908,-0.976541666666834));
#27893=CARTESIAN_POINT('Ctrl Pts',(17.4320632938681,14.3845227371939,-1.0182083333335));
#27894=CARTESIAN_POINT('Ctrl Pts',(17.4320632938681,15.5000000000002,-1.05987500000017));
#27895=CARTESIAN_POINT('Ctrl Pts',(17.4320632938681,16.6154772628064,-1.10154166666683));
#27896=CARTESIAN_POINT('Ctrl Pts',(16.466031646934,17.1732158942095,-1.1432083333335));
#27897=CARTESIAN_POINT('Ctrl Pts',(15.4999999999998,17.7309545256126,-1.18487500000017));
#27898=CARTESIAN_POINT('Ctrl Pts',(14.5339683530657,17.1732158942095,-1.22654166666684));
#27899=CARTESIAN_POINT('Ctrl Pts',(13.5679367061316,16.6154772628064,-1.2682083333335));
#27900=CARTESIAN_POINT('Ctrl Pts',(13.5679367061316,15.5000000000001,-1.30987500000017));
#27901=CARTESIAN_POINT('Ctrl Pts',(13.5679367061316,14.3845227371939,-1.35154166666684));
#27902=CARTESIAN_POINT('Ctrl Pts',(14.5339683530657,13.8267841057908,-1.3932083333335));
#27903=CARTESIAN_POINT('Ctrl Pts',(15.4999999999999,13.2690454743877,-1.43487500000017));
#27904=CARTESIAN_POINT('Ctrl Pts',(16.466031646934,13.8267841057908,-1.47654166666684));
#27905=CARTESIAN_POINT('Ctrl Pts',(17.4320632938681,14.3845227371939,-1.51820833333351));
#27906=CARTESIAN_POINT('Ctrl Pts',(17.4320632938681,15.5000000000002,-1.55987500000017));
#27907=CARTESIAN_POINT('Ctrl Pts',(17.4320632938681,16.6154772628064,-1.60154166666684));
#27908=CARTESIAN_POINT('Ctrl Pts',(16.466031646934,17.1732158942095,-1.64320833333351));
#27909=CARTESIAN_POINT('Ctrl Pts',(15.4999999999998,17.7309545256126,-1.68487500000018));
#27910=CARTESIAN_POINT('Ctrl Pts',(14.5339683530657,17.1732158942095,-1.72654166666684));
#27911=CARTESIAN_POINT('Ctrl Pts',(14.1783081829976,16.9678753992807,-1.74188192368624));
#27912=CARTESIAN_POINT('Ctrl Pts',(13.936918671564,16.6356255246377,-1.75949830599533));
#27913=CARTESIAN_POINT('Ctrl Pts',(17.0802357869869,15.5000000000002,11.2369972941938));
#27914=CARTESIAN_POINT('Ctrl Pts',(17.0802357869869,16.4123495570002,11.1953306275271));
#27915=CARTESIAN_POINT('Ctrl Pts',(16.2901178934933,16.8685243355002,11.1536639608605));
#27916=CARTESIAN_POINT('Ctrl Pts',(15.4999999999998,17.3246991140003,11.1119972941938));
#27917=CARTESIAN_POINT('Ctrl Pts',(14.7098821065064,16.8685243355002,11.0703306275271));
#27918=CARTESIAN_POINT('Ctrl Pts',(13.9197642130128,16.4123495570002,11.0286639608605));
#27919=CARTESIAN_POINT('Ctrl Pts',(13.9197642130128,15.5000000000001,10.9869972941938));
#27920=CARTESIAN_POINT('Ctrl Pts',(13.9197642130128,14.5876504430001,10.9453306275271));
#27921=CARTESIAN_POINT('Ctrl Pts',(14.7098821065064,14.1314756645001,10.9036639608605));
#27922=CARTESIAN_POINT('Ctrl Pts',(15.4999999999999,13.6753008860001,10.8619972941938));
#27923=CARTESIAN_POINT('Ctrl Pts',(16.2901178934933,14.1314756645001,10.8203306275271));
#27924=CARTESIAN_POINT('Ctrl Pts',(17.0802357869869,14.5876504430001,10.7786639608605));
#27925=CARTESIAN_POINT('Ctrl Pts',(17.0802357869869,15.5000000000002,10.7369972941938));
#27926=CARTESIAN_POINT('Ctrl Pts',(17.0802357869869,16.4123495570002,10.6953306275271));
#27927=CARTESIAN_POINT('Ctrl Pts',(16.2901178934933,16.8685243355002,10.6536639608605));
#27928=CARTESIAN_POINT('Ctrl Pts',(15.4999999999998,17.3246991140003,10.6119972941938));
#27929=CARTESIAN_POINT('Ctrl Pts',(14.7098821065064,16.8685243355002,10.5703306275271));
#27930=CARTESIAN_POINT('Ctrl Pts',(13.9197642130128,16.4123495570002,10.5286639608605));
#27931=CARTESIAN_POINT('Ctrl Pts',(13.9197642130128,15.5000000000001,10.4869972941938));
#27932=CARTESIAN_POINT('Ctrl Pts',(13.9197642130128,14.5876504430001,10.4453306275271));
#27933=CARTESIAN_POINT('Ctrl Pts',(14.7098821065064,14.1314756645001,10.4036639608605));
#27934=CARTESIAN_POINT('Ctrl Pts',(15.4999999999999,13.6753008860001,10.3619972941938));
#27935=CARTESIAN_POINT('Ctrl Pts',(16.2901178934933,14.1314756645001,10.3203306275271));
#27936=CARTESIAN_POINT('Ctrl Pts',(17.0802357869869,14.5876504430001,10.2786639608605));
#27937=CARTESIAN_POINT('Ctrl Pts',(17.0802357869869,15.5000000000002,10.2369972941938));
#27938=CARTESIAN_POINT('Ctrl Pts',(17.0802357869869,16.4123495570002,10.1953306275271));
#27939=CARTESIAN_POINT('Ctrl Pts',(16.2901178934933,16.8685243355002,10.1536639608605));
#27940=CARTESIAN_POINT('Ctrl Pts',(15.4999999999998,17.3246991140003,10.1119972941938));
#27941=CARTESIAN_POINT('Ctrl Pts',(14.7098821065064,16.8685243355002,10.0703306275271));
#27942=CARTESIAN_POINT('Ctrl Pts',(13.9197642130128,16.4123495570002,10.0286639608605));
#27943=CARTESIAN_POINT('Ctrl Pts',(13.9197642130128,15.5000000000001,9.98699729419377));
#27944=CARTESIAN_POINT('Ctrl Pts',(13.9197642130128,14.5876504430001,9.94533062752711));
#27945=CARTESIAN_POINT('Ctrl Pts',(14.7098821065064,14.1314756645001,9.90366396086044));
#27946=CARTESIAN_POINT('Ctrl Pts',(15.4999999999999,13.6753008860001,9.86199729419377));
#27947=CARTESIAN_POINT('Ctrl Pts',(16.2901178934933,14.1314756645001,9.82033062752711));
#27948=CARTESIAN_POINT('Ctrl Pts',(17.0802357869869,14.5876504430001,9.77866396086044));
#27949=CARTESIAN_POINT('Ctrl Pts',(17.0802357869869,15.5000000000002,9.73699729419377));
#27950=CARTESIAN_POINT('Ctrl Pts',(17.0802357869869,16.4123495570002,9.6953306275271));
#27951=CARTESIAN_POINT('Ctrl Pts',(16.2901178934933,16.8685243355002,9.65366396086044));
#27952=CARTESIAN_POINT('Ctrl Pts',(15.4999999999998,17.3246991140003,9.61199729419377));
#27953=CARTESIAN_POINT('Ctrl Pts',(14.7098821065064,16.8685243355002,9.5703306275271));
#27954=CARTESIAN_POINT('Ctrl Pts',(13.9197642130128,16.4123495570002,9.52866396086043));
#27955=CARTESIAN_POINT('Ctrl Pts',(13.9197642130128,15.5000000000001,9.48699729419377));
#27956=CARTESIAN_POINT('Ctrl Pts',(13.9197642130128,14.5876504430001,9.4453306275271));
#27957=CARTESIAN_POINT('Ctrl Pts',(14.7098821065064,14.1314756645001,9.40366396086043));
#27958=CARTESIAN_POINT('Ctrl Pts',(15.4999999999999,13.6753008860001,9.36199729419377));
#27959=CARTESIAN_POINT('Ctrl Pts',(16.2901178934933,14.1314756645001,9.3203306275271));
#27960=CARTESIAN_POINT('Ctrl Pts',(17.0802357869869,14.5876504430001,9.27866396086043));
#27961=CARTESIAN_POINT('Ctrl Pts',(17.0802357869869,15.5000000000002,9.23699729419377));
#27962=CARTESIAN_POINT('Ctrl Pts',(17.0802357869869,16.4123495570002,9.1953306275271));
#27963=CARTESIAN_POINT('Ctrl Pts',(16.2901178934933,16.8685243355002,9.15366396086043));
#27964=CARTESIAN_POINT('Ctrl Pts',(15.4999999999998,17.3246991140003,9.11199729419376));
#27965=CARTESIAN_POINT('Ctrl Pts',(14.7098821065064,16.8685243355002,9.07033062752709));
#27966=CARTESIAN_POINT('Ctrl Pts',(13.9197642130128,16.4123495570002,9.02866396086043));
#27967=CARTESIAN_POINT('Ctrl Pts',(13.9197642130128,15.5000000000001,8.98699729419377));
#27968=CARTESIAN_POINT('Ctrl Pts',(13.9197642130128,14.5876504430001,8.94533062752709));
#27969=CARTESIAN_POINT('Ctrl Pts',(14.7098821065064,14.1314756645001,8.90366396086043));
#27970=CARTESIAN_POINT('Ctrl Pts',(15.4999999999999,13.6753008860001,8.86199729419377));
#27971=CARTESIAN_POINT('Ctrl Pts',(16.2901178934933,14.1314756645001,8.82033062752709));
#27972=CARTESIAN_POINT('Ctrl Pts',(17.0802357869869,14.5876504430001,8.77866396086042));
#27973=CARTESIAN_POINT('Ctrl Pts',(17.0802357869869,15.5000000000002,8.73699729419377));
#27974=CARTESIAN_POINT('Ctrl Pts',(17.0802357869869,16.4123495570002,8.69533062752709));
#27975=CARTESIAN_POINT('Ctrl Pts',(16.2901178934933,16.8685243355002,8.65366396086042));
#27976=CARTESIAN_POINT('Ctrl Pts',(15.4999999999998,17.3246991140003,8.61199729419376));
#27977=CARTESIAN_POINT('Ctrl Pts',(14.7098821065064,16.8685243355002,8.57033062752709));
#27978=CARTESIAN_POINT('Ctrl Pts',(13.9197642130128,16.4123495570002,8.52866396086042));
#27979=CARTESIAN_POINT('Ctrl Pts',(13.9197642130128,15.5000000000001,8.48699729419375));
#27980=CARTESIAN_POINT('Ctrl Pts',(13.9197642130128,14.5876504430001,8.44533062752709));
#27981=CARTESIAN_POINT('Ctrl Pts',(14.7098821065064,14.1314756645001,8.40366396086042));
#27982=CARTESIAN_POINT('Ctrl Pts',(15.4999999999999,13.6753008860001,8.36199729419375));
#27983=CARTESIAN_POINT('Ctrl Pts',(16.2901178934933,14.1314756645001,8.32033062752709));
#27984=CARTESIAN_POINT('Ctrl Pts',(17.0802357869869,14.5876504430001,8.27866396086042));
#27985=CARTESIAN_POINT('Ctrl Pts',(17.0802357869869,15.5000000000002,8.23699729419376));
#27986=CARTESIAN_POINT('Ctrl Pts',(17.0802357869869,16.4123495570002,8.19533062752708));
#27987=CARTESIAN_POINT('Ctrl Pts',(16.2901178934933,16.8685243355002,8.15366396086042));
#27988=CARTESIAN_POINT('Ctrl Pts',(15.4999999999998,17.3246991140003,8.11199729419375));
#27989=CARTESIAN_POINT('Ctrl Pts',(14.7098821065064,16.8685243355002,8.07033062752709));
#27990=CARTESIAN_POINT('Ctrl Pts',(13.9197642130128,16.4123495570002,8.02866396086042));
#27991=CARTESIAN_POINT('Ctrl Pts',(13.9197642130128,15.5000000000001,7.98699729419375));
#27992=CARTESIAN_POINT('Ctrl Pts',(13.9197642130128,14.5876504430001,7.94533062752708));
#27993=CARTESIAN_POINT('Ctrl Pts',(14.7098821065064,14.1314756645001,7.90366396086042));
#27994=CARTESIAN_POINT('Ctrl Pts',(15.4999999999999,13.6753008860001,7.86199729419375));
#27995=CARTESIAN_POINT('Ctrl Pts',(16.2901178934933,14.1314756645001,7.82033062752708));
#27996=CARTESIAN_POINT('Ctrl Pts',(17.0802357869869,14.5876504430001,7.77866396086041));
#27997=CARTESIAN_POINT('Ctrl Pts',(17.0802357869869,15.5000000000002,7.73699729419374));
#27998=CARTESIAN_POINT('Ctrl Pts',(17.0802357869869,16.4123495570002,7.69533062752708));
#27999=CARTESIAN_POINT('Ctrl Pts',(16.2901178934933,16.8685243355002,7.65366396086041));
#28000=CARTESIAN_POINT('Ctrl Pts',(15.4999999999998,17.3246991140003,7.61199729419374));
#28001=CARTESIAN_POINT('Ctrl Pts',(14.7098821065064,16.8685243355002,7.57033062752708));
#28002=CARTESIAN_POINT('Ctrl Pts',(13.9197642130128,16.4123495570002,7.52866396086041));
#28003=CARTESIAN_POINT('Ctrl Pts',(13.9197642130128,15.5000000000001,7.48699729419375));
#28004=CARTESIAN_POINT('Ctrl Pts',(13.9197642130128,14.5876504430001,7.44533062752707));
#28005=CARTESIAN_POINT('Ctrl Pts',(14.7098821065064,14.1314756645001,7.4036639608604));
#28006=CARTESIAN_POINT('Ctrl Pts',(15.4999999999999,13.6753008860001,7.36199729419374));
#28007=CARTESIAN_POINT('Ctrl Pts',(16.2901178934933,14.1314756645001,7.32033062752707));
#28008=CARTESIAN_POINT('Ctrl Pts',(17.0802357869869,14.5876504430001,7.27866396086041));
#28009=CARTESIAN_POINT('Ctrl Pts',(17.0802357869869,15.5000000000002,7.23699729419374));
#28010=CARTESIAN_POINT('Ctrl Pts',(17.0802357869869,16.4123495570002,7.19533062752707));
#28011=CARTESIAN_POINT('Ctrl Pts',(16.2901178934933,16.8685243355002,7.1536639608604));
#28012=CARTESIAN_POINT('Ctrl Pts',(15.4999999999998,17.3246991140003,7.11199729419373));
#28013=CARTESIAN_POINT('Ctrl Pts',(14.7098821065064,16.8685243355002,7.07033062752707));
#28014=CARTESIAN_POINT('Ctrl Pts',(13.9197642130128,16.4123495570002,7.0286639608604));
#28015=CARTESIAN_POINT('Ctrl Pts',(13.9197642130128,15.5000000000001,6.98699729419373));
#28016=CARTESIAN_POINT('Ctrl Pts',(13.9197642130128,14.5876504430001,6.94533062752707));
#28017=CARTESIAN_POINT('Ctrl Pts',(14.7098821065064,14.1314756645001,6.90366396086041));
#28018=CARTESIAN_POINT('Ctrl Pts',(15.4999999999999,13.6753008860001,6.86199729419373));
#28019=CARTESIAN_POINT('Ctrl Pts',(16.2901178934933,14.1314756645001,6.82033062752706));
#28020=CARTESIAN_POINT('Ctrl Pts',(17.0802357869869,14.5876504430001,6.7786639608604));
#28021=CARTESIAN_POINT('Ctrl Pts',(17.0802357869869,15.5000000000002,6.73699729419373));
#28022=CARTESIAN_POINT('Ctrl Pts',(17.0802357869869,16.4123495570002,6.69533062752706));
#28023=CARTESIAN_POINT('Ctrl Pts',(16.2901178934933,16.8685243355002,6.6536639608604));
#28024=CARTESIAN_POINT('Ctrl Pts',(15.4999999999998,17.3246991140003,6.61199729419373));
#28025=CARTESIAN_POINT('Ctrl Pts',(14.7098821065064,16.8685243355002,6.57033062752706));
#28026=CARTESIAN_POINT('Ctrl Pts',(13.9197642130128,16.4123495570002,6.52866396086039));
#28027=CARTESIAN_POINT('Ctrl Pts',(13.9197642130128,15.5000000000001,6.48699729419373));
#28028=CARTESIAN_POINT('Ctrl Pts',(13.9197642130128,14.5876504430001,6.44533062752706));
#28029=CARTESIAN_POINT('Ctrl Pts',(14.7098821065064,14.1314756645001,6.40366396086039));
#28030=CARTESIAN_POINT('Ctrl Pts',(15.4999999999999,13.6753008860001,6.36199729419373));
#28031=CARTESIAN_POINT('Ctrl Pts',(16.2901178934933,14.1314756645001,6.32033062752707));
#28032=CARTESIAN_POINT('Ctrl Pts',(17.0802357869869,14.5876504430001,6.27866396086039));
#28033=CARTESIAN_POINT('Ctrl Pts',(17.0802357869869,15.5000000000002,6.23699729419372));
#28034=CARTESIAN_POINT('Ctrl Pts',(17.0802357869869,16.4123495570002,6.19533062752706));
#28035=CARTESIAN_POINT('Ctrl Pts',(16.2901178934933,16.8685243355002,6.1536639608604));
#28036=CARTESIAN_POINT('Ctrl Pts',(15.4999999999998,17.3246991140003,6.11199729419372));
#28037=CARTESIAN_POINT('Ctrl Pts',(14.7098821065064,16.8685243355002,6.07033062752705));
#28038=CARTESIAN_POINT('Ctrl Pts',(13.9197642130128,16.4123495570002,6.02866396086039));
#28039=CARTESIAN_POINT('Ctrl Pts',(13.9197642130128,15.5000000000001,5.98699729419372));
#28040=CARTESIAN_POINT('Ctrl Pts',(13.9197642130128,14.5876504430001,5.94533062752705));
#28041=CARTESIAN_POINT('Ctrl Pts',(14.7098821065064,14.1314756645001,5.90366396086039));
#28042=CARTESIAN_POINT('Ctrl Pts',(15.4999999999999,13.6753008860001,5.86199729419372));
#28043=CARTESIAN_POINT('Ctrl Pts',(16.2901178934933,14.1314756645001,5.82033062752705));
#28044=CARTESIAN_POINT('Ctrl Pts',(17.0802357869869,14.5876504430001,5.77866396086038));
#28045=CARTESIAN_POINT('Ctrl Pts',(17.0802357869869,15.5000000000002,5.73699729419372));
#28046=CARTESIAN_POINT('Ctrl Pts',(17.0802357869869,16.4123495570002,5.69533062752705));
#28047=CARTESIAN_POINT('Ctrl Pts',(16.2901178934933,16.8685243355002,5.65366396086038));
#28048=CARTESIAN_POINT('Ctrl Pts',(15.4999999999998,17.3246991140003,5.61199729419371));
#28049=CARTESIAN_POINT('Ctrl Pts',(14.7098821065064,16.8685243355002,5.57033062752705));
#28050=CARTESIAN_POINT('Ctrl Pts',(13.9197642130128,16.4123495570002,5.52866396086038));
#28051=CARTESIAN_POINT('Ctrl Pts',(13.9197642130128,15.5000000000001,5.48699729419371));
#28052=CARTESIAN_POINT('Ctrl Pts',(13.9197642130128,14.5876504430001,5.44533062752705));
#28053=CARTESIAN_POINT('Ctrl Pts',(14.7098821065064,14.1314756645001,5.40366396086038));
#28054=CARTESIAN_POINT('Ctrl Pts',(15.4999999999999,13.6753008860001,5.36199729419371));
#28055=CARTESIAN_POINT('Ctrl Pts',(16.2901178934933,14.1314756645001,5.32033062752704));
#28056=CARTESIAN_POINT('Ctrl Pts',(17.0802357869869,14.5876504430001,5.27866396086038));
#28057=CARTESIAN_POINT('Ctrl Pts',(17.0802357869869,15.5000000000002,5.23699729419371));
#28058=CARTESIAN_POINT('Ctrl Pts',(17.0802357869869,16.4123495570002,5.19533062752704));
#28059=CARTESIAN_POINT('Ctrl Pts',(16.2901178934933,16.8685243355002,5.15366396086038));
#28060=CARTESIAN_POINT('Ctrl Pts',(15.4999999999998,17.3246991140003,5.11199729419371));
#28061=CARTESIAN_POINT('Ctrl Pts',(14.7098821065064,16.8685243355002,5.07033062752704));
#28062=CARTESIAN_POINT('Ctrl Pts',(13.9197642130128,16.4123495570002,5.02866396086037));
#28063=CARTESIAN_POINT('Ctrl Pts',(13.9197642130128,15.5000000000001,4.98699729419371));
#28064=CARTESIAN_POINT('Ctrl Pts',(13.9197642130128,14.5876504430001,4.94533062752704));
#28065=CARTESIAN_POINT('Ctrl Pts',(14.7098821065064,14.1314756645001,4.90366396086037));
#28066=CARTESIAN_POINT('Ctrl Pts',(15.4999999999999,13.6753008860001,4.8619972941937));
#28067=CARTESIAN_POINT('Ctrl Pts',(16.2901178934933,14.1314756645001,4.82033062752704));
#28068=CARTESIAN_POINT('Ctrl Pts',(17.0802357869869,14.5876504430001,4.77866396086037));
#28069=CARTESIAN_POINT('Ctrl Pts',(17.0802357869869,15.5000000000002,4.7369972941937));
#28070=CARTESIAN_POINT('Ctrl Pts',(17.0802357869869,16.4123495570002,4.69533062752704));
#28071=CARTESIAN_POINT('Ctrl Pts',(16.2901178934933,16.8685243355002,4.65366396086037));
#28072=CARTESIAN_POINT('Ctrl Pts',(15.4999999999998,17.3246991140003,4.6119972941937));
#28073=CARTESIAN_POINT('Ctrl Pts',(14.7098821065064,16.8685243355002,4.57033062752703));
#28074=CARTESIAN_POINT('Ctrl Pts',(13.9197642130128,16.4123495570002,4.52866396086037));
#28075=CARTESIAN_POINT('Ctrl Pts',(13.9197642130128,15.5000000000001,4.4869972941937));
#28076=CARTESIAN_POINT('Ctrl Pts',(13.9197642130128,14.5876504430001,4.44533062752703));
#28077=CARTESIAN_POINT('Ctrl Pts',(14.7098821065064,14.1314756645001,4.40366396086037));
#28078=CARTESIAN_POINT('Ctrl Pts',(15.4999999999999,13.6753008860001,4.3619972941937));
#28079=CARTESIAN_POINT('Ctrl Pts',(16.2901178934933,14.1314756645001,4.32033062752703));
#28080=CARTESIAN_POINT('Ctrl Pts',(17.0802357869869,14.5876504430001,4.27866396086036));
#28081=CARTESIAN_POINT('Ctrl Pts',(17.0802357869869,15.5000000000002,4.2369972941937));
#28082=CARTESIAN_POINT('Ctrl Pts',(17.0802357869869,16.4123495570002,4.19533062752703));
#28083=CARTESIAN_POINT('Ctrl Pts',(16.2901178934933,16.8685243355002,4.15366396086036));
#28084=CARTESIAN_POINT('Ctrl Pts',(15.4999999999998,17.3246991140003,4.11199729419369));
#28085=CARTESIAN_POINT('Ctrl Pts',(14.7098821065064,16.8685243355002,4.07033062752703));
#28086=CARTESIAN_POINT('Ctrl Pts',(13.9197642130128,16.4123495570002,4.02866396086036));
#28087=CARTESIAN_POINT('Ctrl Pts',(13.9197642130128,15.5000000000001,3.98699729419369));
#28088=CARTESIAN_POINT('Ctrl Pts',(13.9197642130128,14.5876504430001,3.94533062752703));
#28089=CARTESIAN_POINT('Ctrl Pts',(14.7098821065064,14.1314756645001,3.90366396086036));
#28090=CARTESIAN_POINT('Ctrl Pts',(15.4999999999999,13.6753008860001,3.86199729419369));
#28091=CARTESIAN_POINT('Ctrl Pts',(16.2901178934933,14.1314756645001,3.82033062752702));
#28092=CARTESIAN_POINT('Ctrl Pts',(17.0802357869869,14.5876504430001,3.77866396086036));
#28093=CARTESIAN_POINT('Ctrl Pts',(17.0802357869869,15.5000000000002,3.73699729419369));
#28094=CARTESIAN_POINT('Ctrl Pts',(17.0802357869869,16.4123495570002,3.69533062752702));
#28095=CARTESIAN_POINT('Ctrl Pts',(16.2901178934933,16.8685243355002,3.65366396086036));
#28096=CARTESIAN_POINT('Ctrl Pts',(15.4999999999998,17.3246991140003,3.61199729419369));
#28097=CARTESIAN_POINT('Ctrl Pts',(14.7098821065064,16.8685243355002,3.57033062752702));
#28098=CARTESIAN_POINT('Ctrl Pts',(13.9197642130128,16.4123495570002,3.52866396086035));
#28099=CARTESIAN_POINT('Ctrl Pts',(13.9197642130128,15.5000000000001,3.48699729419369));
#28100=CARTESIAN_POINT('Ctrl Pts',(13.9197642130128,14.5876504430001,3.44533062752702));
#28101=CARTESIAN_POINT('Ctrl Pts',(14.7098821065064,14.1314756645001,3.40366396086035));
#28102=CARTESIAN_POINT('Ctrl Pts',(15.4999999999999,13.6753008860001,3.36199729419369));
#28103=CARTESIAN_POINT('Ctrl Pts',(16.2901178934933,14.1314756645001,3.32033062752702));
#28104=CARTESIAN_POINT('Ctrl Pts',(17.0802357869869,14.5876504430001,3.27866396086035));
#28105=CARTESIAN_POINT('Ctrl Pts',(17.0802357869869,15.5000000000002,3.23699729419368));
#28106=CARTESIAN_POINT('Ctrl Pts',(17.0802357869869,16.4123495570002,3.19533062752702));
#28107=CARTESIAN_POINT('Ctrl Pts',(16.2901178934933,16.8685243355002,3.15366396086035));
#28108=CARTESIAN_POINT('Ctrl Pts',(15.4999999999998,17.3246991140003,3.11199729419368));
#28109=CARTESIAN_POINT('Ctrl Pts',(14.7098821065064,16.8685243355002,3.07033062752702));
#28110=CARTESIAN_POINT('Ctrl Pts',(13.9197642130128,16.4123495570002,3.02866396086035));
#28111=CARTESIAN_POINT('Ctrl Pts',(13.9197642130128,15.5000000000001,2.98699729419368));
#28112=CARTESIAN_POINT('Ctrl Pts',(13.9197642130128,14.5876504430001,2.94533062752701));
#28113=CARTESIAN_POINT('Ctrl Pts',(14.7098821065064,14.1314756645001,2.90366396086035));
#28114=CARTESIAN_POINT('Ctrl Pts',(15.4999999999999,13.6753008860001,2.86199729419368));
#28115=CARTESIAN_POINT('Ctrl Pts',(16.2901178934933,14.1314756645001,2.82033062752701));
#28116=CARTESIAN_POINT('Ctrl Pts',(17.0802357869869,14.5876504430001,2.77866396086034));
#28117=CARTESIAN_POINT('Ctrl Pts',(17.0802357869869,15.5000000000002,2.73699729419368));
#28118=CARTESIAN_POINT('Ctrl Pts',(17.0802357869869,16.4123495570002,2.69533062752701));
#28119=CARTESIAN_POINT('Ctrl Pts',(16.2901178934933,16.8685243355002,2.65366396086034));
#28120=CARTESIAN_POINT('Ctrl Pts',(15.4999999999998,17.3246991140003,2.61199729419367));
#28121=CARTESIAN_POINT('Ctrl Pts',(14.7098821065064,16.8685243355002,2.57033062752701));
#28122=CARTESIAN_POINT('Ctrl Pts',(13.9197642130128,16.4123495570002,2.52866396086034));
#28123=CARTESIAN_POINT('Ctrl Pts',(13.9197642130128,15.5000000000001,2.48699729419367));
#28124=CARTESIAN_POINT('Ctrl Pts',(13.9197642130128,14.5876504430001,2.44533062752701));
#28125=CARTESIAN_POINT('Ctrl Pts',(14.7098821065064,14.1314756645001,2.40366396086034));
#28126=CARTESIAN_POINT('Ctrl Pts',(15.4999999999999,13.6753008860001,2.36199729419367));
#28127=CARTESIAN_POINT('Ctrl Pts',(16.2901178934933,14.1314756645001,2.32033062752701));
#28128=CARTESIAN_POINT('Ctrl Pts',(17.0802357869869,14.5876504430001,2.27866396086034));
#28129=CARTESIAN_POINT('Ctrl Pts',(17.0802357869869,15.5000000000002,2.23699729419367));
#28130=CARTESIAN_POINT('Ctrl Pts',(17.0802357869869,16.4123495570002,2.195330627527));
#28131=CARTESIAN_POINT('Ctrl Pts',(16.2901178934933,16.8685243355002,2.15366396086034));
#28132=CARTESIAN_POINT('Ctrl Pts',(15.4999999999998,17.3246991140003,2.11199729419367));
#28133=CARTESIAN_POINT('Ctrl Pts',(14.7098821065064,16.8685243355002,2.070330627527));
#28134=CARTESIAN_POINT('Ctrl Pts',(13.9197642130128,16.4123495570002,2.02866396086033));
#28135=CARTESIAN_POINT('Ctrl Pts',(13.9197642130128,15.5000000000001,1.98699729419367));
#28136=CARTESIAN_POINT('Ctrl Pts',(13.9197642130128,14.5876504430001,1.945330627527));
#28137=CARTESIAN_POINT('Ctrl Pts',(14.7098821065064,14.1314756645001,1.90366396086033));
#28138=CARTESIAN_POINT('Ctrl Pts',(15.4999999999999,13.6753008860001,1.86199729419367));
#28139=CARTESIAN_POINT('Ctrl Pts',(16.2901178934933,14.1314756645001,1.820330627527));
#28140=CARTESIAN_POINT('Ctrl Pts',(17.0802357869869,14.5876504430001,1.77866396086033));
#28141=CARTESIAN_POINT('Ctrl Pts',(17.0802357869869,15.5000000000002,1.73699729419366));
#28142=CARTESIAN_POINT('Ctrl Pts',(17.0802357869869,16.4123495570002,1.695330627527));
#28143=CARTESIAN_POINT('Ctrl Pts',(16.2901178934933,16.8685243355002,1.65366396086033));
#28144=CARTESIAN_POINT('Ctrl Pts',(15.4999999999998,17.3246991140003,1.61199729419366));
#28145=CARTESIAN_POINT('Ctrl Pts',(14.7098821065064,16.8685243355002,1.57033062752699));
#28146=CARTESIAN_POINT('Ctrl Pts',(13.9197642130128,16.4123495570002,1.52866396086033));
#28147=CARTESIAN_POINT('Ctrl Pts',(13.9197642130128,15.5000000000001,1.48699729419366));
#28148=CARTESIAN_POINT('Ctrl Pts',(13.9197642130128,14.5876504430001,1.44533062752699));
#28149=CARTESIAN_POINT('Ctrl Pts',(14.7098821065064,14.1314756645001,1.40366396086033));
#28150=CARTESIAN_POINT('Ctrl Pts',(15.4999999999999,13.6753008860001,1.36199729419366));
#28151=CARTESIAN_POINT('Ctrl Pts',(16.2901178934933,14.1314756645001,1.32033062752699));
#28152=CARTESIAN_POINT('Ctrl Pts',(17.0802357869869,14.5876504430001,1.27866396086032));
#28153=CARTESIAN_POINT('Ctrl Pts',(17.0802357869869,15.5000000000002,1.23699729419366));
#28154=CARTESIAN_POINT('Ctrl Pts',(17.0802357869869,16.4123495570002,1.19533062752699));
#28155=CARTESIAN_POINT('Ctrl Pts',(16.2901178934933,16.8685243355002,1.15366396086032));
#28156=CARTESIAN_POINT('Ctrl Pts',(15.4999999999998,17.3246991140003,1.11199729419366));
#28157=CARTESIAN_POINT('Ctrl Pts',(14.7098821065064,16.8685243355002,1.07033062752699));
#28158=CARTESIAN_POINT('Ctrl Pts',(13.9197642130128,16.4123495570002,1.02866396086032));
#28159=CARTESIAN_POINT('Ctrl Pts',(13.9197642130128,15.5000000000001,0.986997294193658));
#28160=CARTESIAN_POINT('Ctrl Pts',(13.9197642130128,14.5876504430001,0.945330627526991));
#28161=CARTESIAN_POINT('Ctrl Pts',(14.7098821065064,14.1314756645001,0.903663960860324));
#28162=CARTESIAN_POINT('Ctrl Pts',(15.4999999999999,13.6753008860001,0.861997294193656));
#28163=CARTESIAN_POINT('Ctrl Pts',(16.2901178934933,14.1314756645001,0.820330627526989));
#28164=CARTESIAN_POINT('Ctrl Pts',(17.0802357869869,14.5876504430001,0.778663960860322));
#28165=CARTESIAN_POINT('Ctrl Pts',(17.0802357869869,15.5000000000002,0.736997294193654));
#28166=CARTESIAN_POINT('Ctrl Pts',(17.0802357869869,16.4123495570002,0.695330627526987));
#28167=CARTESIAN_POINT('Ctrl Pts',(16.2901178934933,16.8685243355002,0.65366396086032));
#28168=CARTESIAN_POINT('Ctrl Pts',(15.4999999999998,17.3246991140003,0.611997294193653));
#28169=CARTESIAN_POINT('Ctrl Pts',(14.7098821065064,16.8685243355002,0.570330627526985));
#28170=CARTESIAN_POINT('Ctrl Pts',(13.9197642130128,16.4123495570002,0.528663960860318));
#28171=CARTESIAN_POINT('Ctrl Pts',(13.9197642130128,15.5000000000001,0.486997294193651));
#28172=CARTESIAN_POINT('Ctrl Pts',(13.9197642130128,14.5876504430001,0.445330627526983));
#28173=CARTESIAN_POINT('Ctrl Pts',(14.7098821065064,14.1314756645001,0.403663960860316));
#28174=CARTESIAN_POINT('Ctrl Pts',(15.4999999999999,13.6753008860001,0.361997294193649));
#28175=CARTESIAN_POINT('Ctrl Pts',(16.2901178934933,14.1314756645001,0.320330627526982));
#28176=CARTESIAN_POINT('Ctrl Pts',(17.0802357869869,14.5876504430001,0.278663960860314));
#28177=CARTESIAN_POINT('Ctrl Pts',(17.0802357869869,15.5000000000002,0.236997294193647));
#28178=CARTESIAN_POINT('Ctrl Pts',(17.0802357869869,16.4123495570002,0.19533062752698));
#28179=CARTESIAN_POINT('Ctrl Pts',(16.2901178934933,16.8685243355002,0.153663960860312));
#28180=CARTESIAN_POINT('Ctrl Pts',(15.4999999999998,17.3246991140003,0.111997294193645));
#28181=CARTESIAN_POINT('Ctrl Pts',(14.7098821065064,16.8685243355002,0.0703306275269777));
#28182=CARTESIAN_POINT('Ctrl Pts',(13.9197642130128,16.4123495570002,0.0286639608603104));
#28183=CARTESIAN_POINT('Ctrl Pts',(13.9197642130128,15.5000000000001,-0.0130027058063568));
#28184=CARTESIAN_POINT('Ctrl Pts',(13.9197642130128,14.5876504430001,-0.0546693724730224));
#28185=CARTESIAN_POINT('Ctrl Pts',(14.7098821065064,14.1314756645001,-0.0963360391396897));
#28186=CARTESIAN_POINT('Ctrl Pts',(15.4999999999999,13.6753008860001,-0.138002705806357));
#28187=CARTESIAN_POINT('Ctrl Pts',(16.2901178934933,14.1314756645001,-0.179669372473024));
#28188=CARTESIAN_POINT('Ctrl Pts',(17.0802357869869,14.5876504430001,-0.221336039139691));
#28189=CARTESIAN_POINT('Ctrl Pts',(17.0802357869869,15.5000000000002,-0.263002705806359));
#28190=CARTESIAN_POINT('Ctrl Pts',(17.0802357869869,16.4123495570002,-0.304669372473026));
#28191=CARTESIAN_POINT('Ctrl Pts',(16.2901178934933,16.8685243355002,-0.346336039139693));
#28192=CARTESIAN_POINT('Ctrl Pts',(15.4999999999998,17.3246991140003,-0.38800270580636));
#28193=CARTESIAN_POINT('Ctrl Pts',(14.7098821065064,16.8685243355002,-0.429669372473028));
#28194=CARTESIAN_POINT('Ctrl Pts',(13.9197642130128,16.4123495570002,-0.471336039139695));
#28195=CARTESIAN_POINT('Ctrl Pts',(13.9197642130128,15.5000000000001,-0.513002705806362));
#28196=CARTESIAN_POINT('Ctrl Pts',(13.9197642130128,14.5876504430001,-0.55466937247303));
#28197=CARTESIAN_POINT('Ctrl Pts',(14.7098821065064,14.1314756645001,-0.596336039139697));
#28198=CARTESIAN_POINT('Ctrl Pts',(15.4999999999999,13.6753008860001,-0.638002705806364));
#28199=CARTESIAN_POINT('Ctrl Pts',(16.2901178934933,14.1314756645001,-0.679669372473032));
#28200=CARTESIAN_POINT('Ctrl Pts',(17.0802357869869,14.5876504430001,-0.721336039139699));
#28201=CARTESIAN_POINT('Ctrl Pts',(17.0802357869869,15.5000000000002,-0.763002705806366));
#28202=CARTESIAN_POINT('Ctrl Pts',(17.0802357869869,16.4123495570002,-0.804669372473033));
#28203=CARTESIAN_POINT('Ctrl Pts',(16.2901178934933,16.8685243355002,-0.846336039139701));
#28204=CARTESIAN_POINT('Ctrl Pts',(15.4999999999998,17.3246991140003,-0.888002705806368));
#28205=CARTESIAN_POINT('Ctrl Pts',(14.7098821065064,16.8685243355002,-0.929669372473035));
#28206=CARTESIAN_POINT('Ctrl Pts',(13.9197642130128,16.4123495570002,-0.971336039139702));
#28207=CARTESIAN_POINT('Ctrl Pts',(13.9197642130128,15.5000000000001,-1.01300270580637));
#28208=CARTESIAN_POINT('Ctrl Pts',(13.9197642130128,14.5876504430001,-1.05466937247304));
#28209=CARTESIAN_POINT('Ctrl Pts',(14.7098821065064,14.1314756645001,-1.09633603913971));
#28210=CARTESIAN_POINT('Ctrl Pts',(15.4999999999999,13.6753008860001,-1.13800270580638));
#28211=CARTESIAN_POINT('Ctrl Pts',(16.2901178934933,14.1314756645001,-1.17966937247304));
#28212=CARTESIAN_POINT('Ctrl Pts',(17.0802357869869,14.5876504430001,-1.22133603913971));
#28213=CARTESIAN_POINT('Ctrl Pts',(17.0802357869869,15.5000000000002,-1.26300270580638));
#28214=CARTESIAN_POINT('Ctrl Pts',(17.0802357869869,16.4123495570002,-1.30466937247304));
#28215=CARTESIAN_POINT('Ctrl Pts',(16.2901178934933,16.8685243355002,-1.34633603913971));
#28216=CARTESIAN_POINT('Ctrl Pts',(15.4999999999998,17.3246991140003,-1.38800270580638));
#28217=CARTESIAN_POINT('Ctrl Pts',(14.7098821065064,16.8685243355002,-1.42966937247304));
#28218=CARTESIAN_POINT('Ctrl Pts',(13.9197642130128,16.4123495570002,-1.47133603913971));
#28219=CARTESIAN_POINT('Ctrl Pts',(13.9197642130128,15.5000000000001,-1.51300270580638));
#28220=CARTESIAN_POINT('Ctrl Pts',(13.9197642130128,14.5876504430001,-1.55466937247305));
#28221=CARTESIAN_POINT('Ctrl Pts',(14.7098821065064,14.1314756645001,-1.59633603913971));
#28222=CARTESIAN_POINT('Ctrl Pts',(15.4999999999999,13.6753008860001,-1.63800270580638));
#28223=CARTESIAN_POINT('Ctrl Pts',(16.2901178934933,14.1314756645001,-1.67966937247305));
#28224=CARTESIAN_POINT('Ctrl Pts',(17.0802357869869,14.5876504430001,-1.72133603913972));
#28225=CARTESIAN_POINT('Ctrl Pts',(17.0802357869869,15.5000000000002,-1.76300270580638));
#28226=CARTESIAN_POINT('Ctrl Pts',(17.0802357869869,16.4123495570002,-1.80466937247305));
#28227=CARTESIAN_POINT('Ctrl Pts',(16.2901178934933,16.8685243355002,-1.84633603913972));
#28228=CARTESIAN_POINT('Ctrl Pts',(15.4999999999998,17.3246991140003,-1.88800270580639));
#28229=CARTESIAN_POINT('Ctrl Pts',(14.7098821065064,16.8685243355002,-1.92966937247305));
#28230=CARTESIAN_POINT('Ctrl Pts',(14.4189874290229,16.7005762151493,-1.94500962949244));
#28231=CARTESIAN_POINT('Ctrl Pts',(14.2215547953295,16.4288288330635,-1.96262601180154));
#28232=CARTESIAN_POINT('',(14.2215509627455,16.4288315898518,-1.9626232418845));
#28233=CARTESIAN_POINT('',(14.2215500160355,16.4288304039467,-1.96262332703658));
#28234=CARTESIAN_POINT('Ctrl Pts',(14.5577749122401,14.231389800475,10.4122404735808));
#28235=CARTESIAN_POINT('Ctrl Pts',(14.6309457974486,14.177044152171,10.407829216981));
#28236=CARTESIAN_POINT('Ctrl Pts',(14.7098797632094,14.1314716057908,10.4036666666667));
#28237=CARTESIAN_POINT('Ctrl Pts',(15.4999999999999,13.6752954743877,10.362));
#28238=CARTESIAN_POINT('Ctrl Pts',(16.2901202367903,14.1314716057908,10.3203333333333));
#28239=CARTESIAN_POINT('Ctrl Pts',(17.0802404735807,14.5876477371939,10.2786666666667));
#28240=CARTESIAN_POINT('Ctrl Pts',(17.0802404735807,15.5000000000002,10.237));
#28241=CARTESIAN_POINT('Ctrl Pts',(17.0802404735807,16.4123522628064,10.1953333333333));
#28242=CARTESIAN_POINT('Ctrl Pts',(16.2901202367902,16.8685283942095,10.1536666666667));
#28243=CARTESIAN_POINT('Ctrl Pts',(15.4999999999998,17.3247045256126,10.112));
#28244=CARTESIAN_POINT('Ctrl Pts',(14.7098797632094,16.8685283942095,10.0703333333333));
#28245=CARTESIAN_POINT('Ctrl Pts',(13.919759526419,16.4123522628064,10.0286666666667));
#28246=CARTESIAN_POINT('Ctrl Pts',(13.919759526419,15.5000000000001,9.98699999999998));
#28247=CARTESIAN_POINT('Ctrl Pts',(13.919759526419,14.5876477371939,9.94533333333331));
#28248=CARTESIAN_POINT('Ctrl Pts',(14.7098797632094,14.1314716057908,9.90366666666665));
#28249=CARTESIAN_POINT('Ctrl Pts',(15.4999999999999,13.6752954743877,9.86199999999998));
#28250=CARTESIAN_POINT('Ctrl Pts',(16.2901202367903,14.1314716057908,9.82033333333331));
#28251=CARTESIAN_POINT('Ctrl Pts',(17.0802404735807,14.5876477371939,9.77866666666665));
#28252=CARTESIAN_POINT('Ctrl Pts',(17.0802404735807,15.5000000000002,9.73699999999998));
#28253=CARTESIAN_POINT('Ctrl Pts',(17.0802404735807,16.4123522628064,9.69533333333331));
#28254=CARTESIAN_POINT('Ctrl Pts',(16.2901202367902,16.8685283942095,9.65366666666664));
#28255=CARTESIAN_POINT('Ctrl Pts',(15.4999999999998,17.3247045256126,9.61199999999998));
#28256=CARTESIAN_POINT('Ctrl Pts',(14.7098797632094,16.8685283942095,9.57033333333331));
#28257=CARTESIAN_POINT('Ctrl Pts',(13.919759526419,16.4123522628064,9.52866666666664));
#28258=CARTESIAN_POINT('Ctrl Pts',(13.919759526419,15.5000000000001,9.48699999999998));
#28259=CARTESIAN_POINT('Ctrl Pts',(13.919759526419,14.5876477371939,9.44533333333331));
#28260=CARTESIAN_POINT('Ctrl Pts',(14.7098797632094,14.1314716057908,9.40366666666664));
#28261=CARTESIAN_POINT('Ctrl Pts',(15.4999999999999,13.6752954743877,9.36199999999998));
#28262=CARTESIAN_POINT('Ctrl Pts',(16.2901202367903,14.1314716057908,9.32033333333331));
#28263=CARTESIAN_POINT('Ctrl Pts',(17.0802404735807,14.5876477371939,9.27866666666664));
#28264=CARTESIAN_POINT('Ctrl Pts',(17.0802404735807,15.5000000000002,9.23699999999997));
#28265=CARTESIAN_POINT('Ctrl Pts',(17.0802404735807,16.4123522628064,9.19533333333331));
#28266=CARTESIAN_POINT('Ctrl Pts',(16.2901202367902,16.8685283942095,9.15366666666664));
#28267=CARTESIAN_POINT('Ctrl Pts',(15.4999999999998,17.3247045256126,9.11199999999997));
#28268=CARTESIAN_POINT('Ctrl Pts',(14.7098797632094,16.8685283942095,9.0703333333333));
#28269=CARTESIAN_POINT('Ctrl Pts',(13.919759526419,16.4123522628064,9.02866666666664));
#28270=CARTESIAN_POINT('Ctrl Pts',(13.919759526419,15.5000000000001,8.98699999999997));
#28271=CARTESIAN_POINT('Ctrl Pts',(13.919759526419,14.5876477371939,8.9453333333333));
#28272=CARTESIAN_POINT('Ctrl Pts',(14.7098797632094,14.1314716057908,8.90366666666664));
#28273=CARTESIAN_POINT('Ctrl Pts',(15.4999999999999,13.6752954743877,8.86199999999997));
#28274=CARTESIAN_POINT('Ctrl Pts',(16.2901202367903,14.1314716057908,8.8203333333333));
#28275=CARTESIAN_POINT('Ctrl Pts',(17.0802404735807,14.5876477371939,8.77866666666663));
#28276=CARTESIAN_POINT('Ctrl Pts',(17.0802404735807,15.5000000000002,8.73699999999997));
#28277=CARTESIAN_POINT('Ctrl Pts',(17.0802404735807,16.4123522628064,8.6953333333333));
#28278=CARTESIAN_POINT('Ctrl Pts',(16.2901202367902,16.8685283942095,8.65366666666663));
#28279=CARTESIAN_POINT('Ctrl Pts',(15.4999999999998,17.3247045256126,8.61199999999996));
#28280=CARTESIAN_POINT('Ctrl Pts',(14.7098797632094,16.8685283942095,8.57033333333329));
#28281=CARTESIAN_POINT('Ctrl Pts',(13.919759526419,16.4123522628064,8.52866666666663));
#28282=CARTESIAN_POINT('Ctrl Pts',(13.919759526419,15.5000000000001,8.48699999999996));
#28283=CARTESIAN_POINT('Ctrl Pts',(13.919759526419,14.5876477371939,8.44533333333329));
#28284=CARTESIAN_POINT('Ctrl Pts',(14.7098797632094,14.1314716057908,8.40366666666663));
#28285=CARTESIAN_POINT('Ctrl Pts',(15.4999999999999,13.6752954743877,8.36199999999996));
#28286=CARTESIAN_POINT('Ctrl Pts',(16.2901202367903,14.1314716057908,8.32033333333329));
#28287=CARTESIAN_POINT('Ctrl Pts',(17.0802404735807,14.5876477371939,8.27866666666663));
#28288=CARTESIAN_POINT('Ctrl Pts',(17.0802404735807,15.5000000000002,8.23699999999996));
#28289=CARTESIAN_POINT('Ctrl Pts',(17.0802404735807,16.4123522628064,8.19533333333329));
#28290=CARTESIAN_POINT('Ctrl Pts',(16.2901202367902,16.8685283942095,8.15366666666663));
#28291=CARTESIAN_POINT('Ctrl Pts',(15.4999999999998,17.3247045256126,8.11199999999996));
#28292=CARTESIAN_POINT('Ctrl Pts',(14.7098797632094,16.8685283942095,8.07033333333329));
#28293=CARTESIAN_POINT('Ctrl Pts',(13.919759526419,16.4123522628064,8.02866666666662));
#28294=CARTESIAN_POINT('Ctrl Pts',(13.919759526419,15.5000000000001,7.98699999999996));
#28295=CARTESIAN_POINT('Ctrl Pts',(13.919759526419,14.5876477371939,7.94533333333329));
#28296=CARTESIAN_POINT('Ctrl Pts',(14.7098797632094,14.1314716057908,7.90366666666662));
#28297=CARTESIAN_POINT('Ctrl Pts',(15.4999999999999,13.6752954743877,7.86199999999995));
#28298=CARTESIAN_POINT('Ctrl Pts',(16.2901202367903,14.1314716057908,7.82033333333329));
#28299=CARTESIAN_POINT('Ctrl Pts',(17.0802404735807,14.5876477371939,7.77866666666662));
#28300=CARTESIAN_POINT('Ctrl Pts',(17.0802404735807,15.5000000000002,7.73699999999995));
#28301=CARTESIAN_POINT('Ctrl Pts',(17.0802404735807,16.4123522628064,7.69533333333329));
#28302=CARTESIAN_POINT('Ctrl Pts',(16.2901202367902,16.8685283942095,7.65366666666662));
#28303=CARTESIAN_POINT('Ctrl Pts',(15.4999999999998,17.3247045256126,7.61199999999995));
#28304=CARTESIAN_POINT('Ctrl Pts',(14.7098797632094,16.8685283942095,7.57033333333328));
#28305=CARTESIAN_POINT('Ctrl Pts',(13.919759526419,16.4123522628064,7.52866666666662));
#28306=CARTESIAN_POINT('Ctrl Pts',(13.919759526419,15.5000000000001,7.48699999999995));
#28307=CARTESIAN_POINT('Ctrl Pts',(13.919759526419,14.5876477371939,7.44533333333328));
#28308=CARTESIAN_POINT('Ctrl Pts',(14.7098797632094,14.1314716057908,7.40366666666661));
#28309=CARTESIAN_POINT('Ctrl Pts',(15.4999999999999,13.6752954743877,7.36199999999995));
#28310=CARTESIAN_POINT('Ctrl Pts',(16.2901202367903,14.1314716057908,7.32033333333328));
#28311=CARTESIAN_POINT('Ctrl Pts',(17.0802404735807,14.5876477371939,7.27866666666661));
#28312=CARTESIAN_POINT('Ctrl Pts',(17.0802404735807,15.5000000000002,7.23699999999995));
#28313=CARTESIAN_POINT('Ctrl Pts',(17.0802404735807,16.4123522628064,7.19533333333328));
#28314=CARTESIAN_POINT('Ctrl Pts',(16.2901202367902,16.8685283942095,7.15366666666661));
#28315=CARTESIAN_POINT('Ctrl Pts',(15.4999999999998,17.3247045256126,7.11199999999994));
#28316=CARTESIAN_POINT('Ctrl Pts',(14.7098797632094,16.8685283942095,7.07033333333328));
#28317=CARTESIAN_POINT('Ctrl Pts',(13.919759526419,16.4123522628064,7.02866666666661));
#28318=CARTESIAN_POINT('Ctrl Pts',(13.919759526419,15.5000000000001,6.98699999999994));
#28319=CARTESIAN_POINT('Ctrl Pts',(13.919759526419,14.5876477371939,6.94533333333327));
#28320=CARTESIAN_POINT('Ctrl Pts',(14.7098797632094,14.1314716057908,6.90366666666661));
#28321=CARTESIAN_POINT('Ctrl Pts',(15.4999999999999,13.6752954743877,6.86199999999994));
#28322=CARTESIAN_POINT('Ctrl Pts',(16.2901202367903,14.1314716057908,6.82033333333327));
#28323=CARTESIAN_POINT('Ctrl Pts',(17.0802404735807,14.5876477371939,6.77866666666661));
#28324=CARTESIAN_POINT('Ctrl Pts',(17.0802404735807,15.5000000000002,6.73699999999994));
#28325=CARTESIAN_POINT('Ctrl Pts',(17.0802404735807,16.4123522628064,6.69533333333327));
#28326=CARTESIAN_POINT('Ctrl Pts',(16.2901202367902,16.8685283942095,6.65366666666661));
#28327=CARTESIAN_POINT('Ctrl Pts',(15.4999999999998,17.3247045256126,6.61199999999994));
#28328=CARTESIAN_POINT('Ctrl Pts',(14.7098797632094,16.8685283942095,6.57033333333327));
#28329=CARTESIAN_POINT('Ctrl Pts',(13.919759526419,16.4123522628064,6.5286666666666));
#28330=CARTESIAN_POINT('Ctrl Pts',(13.919759526419,15.5000000000001,6.48699999999994));
#28331=CARTESIAN_POINT('Ctrl Pts',(13.919759526419,14.5876477371939,6.44533333333327));
#28332=CARTESIAN_POINT('Ctrl Pts',(14.7098797632094,14.1314716057908,6.4036666666666));
#28333=CARTESIAN_POINT('Ctrl Pts',(15.4999999999999,13.6752954743877,6.36199999999993));
#28334=CARTESIAN_POINT('Ctrl Pts',(16.2901202367903,14.1314716057908,6.32033333333327));
#28335=CARTESIAN_POINT('Ctrl Pts',(17.0802404735807,14.5876477371939,6.2786666666666));
#28336=CARTESIAN_POINT('Ctrl Pts',(17.0802404735807,15.5000000000002,6.23699999999993));
#28337=CARTESIAN_POINT('Ctrl Pts',(17.0802404735807,16.4123522628064,6.19533333333326));
#28338=CARTESIAN_POINT('Ctrl Pts',(16.2901202367902,16.8685283942095,6.1536666666666));
#28339=CARTESIAN_POINT('Ctrl Pts',(15.4999999999998,17.3247045256126,6.11199999999993));
#28340=CARTESIAN_POINT('Ctrl Pts',(14.7098797632094,16.8685283942095,6.07033333333326));
#28341=CARTESIAN_POINT('Ctrl Pts',(13.919759526419,16.4123522628064,6.0286666666666));
#28342=CARTESIAN_POINT('Ctrl Pts',(13.919759526419,15.5000000000001,5.98699999999993));
#28343=CARTESIAN_POINT('Ctrl Pts',(13.919759526419,14.5876477371939,5.94533333333326));
#28344=CARTESIAN_POINT('Ctrl Pts',(14.7098797632094,14.1314716057908,5.9036666666666));
#28345=CARTESIAN_POINT('Ctrl Pts',(15.4999999999999,13.6752954743877,5.86199999999993));
#28346=CARTESIAN_POINT('Ctrl Pts',(16.2901202367903,14.1314716057908,5.82033333333326));
#28347=CARTESIAN_POINT('Ctrl Pts',(17.0802404735807,14.5876477371939,5.77866666666659));
#28348=CARTESIAN_POINT('Ctrl Pts',(17.0802404735807,15.5000000000002,5.73699999999993));
#28349=CARTESIAN_POINT('Ctrl Pts',(17.0802404735807,16.4123522628064,5.69533333333326));
#28350=CARTESIAN_POINT('Ctrl Pts',(16.2901202367902,16.8685283942095,5.65366666666659));
#28351=CARTESIAN_POINT('Ctrl Pts',(15.4999999999998,17.3247045256126,5.61199999999992));
#28352=CARTESIAN_POINT('Ctrl Pts',(14.7098797632094,16.8685283942095,5.57033333333326));
#28353=CARTESIAN_POINT('Ctrl Pts',(13.919759526419,16.4123522628064,5.52866666666659));
#28354=CARTESIAN_POINT('Ctrl Pts',(13.919759526419,15.5000000000001,5.48699999999992));
#28355=CARTESIAN_POINT('Ctrl Pts',(13.919759526419,14.5876477371939,5.44533333333326));
#28356=CARTESIAN_POINT('Ctrl Pts',(14.7098797632094,14.1314716057908,5.40366666666659));
#28357=CARTESIAN_POINT('Ctrl Pts',(15.4999999999999,13.6752954743877,5.36199999999992));
#28358=CARTESIAN_POINT('Ctrl Pts',(16.2901202367903,14.1314716057908,5.32033333333325));
#28359=CARTESIAN_POINT('Ctrl Pts',(17.0802404735807,14.5876477371939,5.27866666666659));
#28360=CARTESIAN_POINT('Ctrl Pts',(17.0802404735807,15.5000000000002,5.23699999999992));
#28361=CARTESIAN_POINT('Ctrl Pts',(17.0802404735807,16.4123522628064,5.19533333333325));
#28362=CARTESIAN_POINT('Ctrl Pts',(16.2901202367902,16.8685283942095,5.15366666666658));
#28363=CARTESIAN_POINT('Ctrl Pts',(15.4999999999998,17.3247045256126,5.11199999999992));
#28364=CARTESIAN_POINT('Ctrl Pts',(14.7098797632094,16.8685283942095,5.07033333333325));
#28365=CARTESIAN_POINT('Ctrl Pts',(13.919759526419,16.4123522628064,5.02866666666658));
#28366=CARTESIAN_POINT('Ctrl Pts',(13.919759526419,15.5000000000001,4.98699999999992));
#28367=CARTESIAN_POINT('Ctrl Pts',(13.919759526419,14.5876477371939,4.94533333333325));
#28368=CARTESIAN_POINT('Ctrl Pts',(14.7098797632094,14.1314716057908,4.90366666666658));
#28369=CARTESIAN_POINT('Ctrl Pts',(15.4999999999999,13.6752954743877,4.86199999999991));
#28370=CARTESIAN_POINT('Ctrl Pts',(16.2901202367903,14.1314716057908,4.82033333333325));
#28371=CARTESIAN_POINT('Ctrl Pts',(17.0802404735807,14.5876477371939,4.77866666666658));
#28372=CARTESIAN_POINT('Ctrl Pts',(17.0802404735807,15.5000000000002,4.73699999999991));
#28373=CARTESIAN_POINT('Ctrl Pts',(17.0802404735807,16.4123522628064,4.69533333333325));
#28374=CARTESIAN_POINT('Ctrl Pts',(16.2901202367902,16.8685283942095,4.65366666666658));
#28375=CARTESIAN_POINT('Ctrl Pts',(15.4999999999998,17.3247045256126,4.61199999999991));
#28376=CARTESIAN_POINT('Ctrl Pts',(14.7098797632094,16.8685283942095,4.57033333333324));
#28377=CARTESIAN_POINT('Ctrl Pts',(13.919759526419,16.4123522628064,4.52866666666658));
#28378=CARTESIAN_POINT('Ctrl Pts',(13.919759526419,15.5000000000001,4.48699999999991));
#28379=CARTESIAN_POINT('Ctrl Pts',(13.919759526419,14.5876477371939,4.44533333333324));
#28380=CARTESIAN_POINT('Ctrl Pts',(14.7098797632094,14.1314716057908,4.40366666666658));
#28381=CARTESIAN_POINT('Ctrl Pts',(15.4999999999999,13.6752954743877,4.36199999999991));
#28382=CARTESIAN_POINT('Ctrl Pts',(16.2901202367903,14.1314716057908,4.32033333333324));
#28383=CARTESIAN_POINT('Ctrl Pts',(17.0802404735807,14.5876477371939,4.27866666666657));
#28384=CARTESIAN_POINT('Ctrl Pts',(17.0802404735807,15.5000000000002,4.23699999999991));
#28385=CARTESIAN_POINT('Ctrl Pts',(17.0802404735807,16.4123522628064,4.19533333333324));
#28386=CARTESIAN_POINT('Ctrl Pts',(16.2901202367902,16.8685283942095,4.15366666666657));
#28387=CARTESIAN_POINT('Ctrl Pts',(15.4999999999998,17.3247045256126,4.1119999999999));
#28388=CARTESIAN_POINT('Ctrl Pts',(14.7098797632094,16.8685283942095,4.07033333333324));
#28389=CARTESIAN_POINT('Ctrl Pts',(13.919759526419,16.4123522628064,4.02866666666657));
#28390=CARTESIAN_POINT('Ctrl Pts',(13.919759526419,15.5000000000001,3.9869999999999));
#28391=CARTESIAN_POINT('Ctrl Pts',(13.919759526419,14.5876477371939,3.94533333333323));
#28392=CARTESIAN_POINT('Ctrl Pts',(14.7098797632094,14.1314716057908,3.90366666666657));
#28393=CARTESIAN_POINT('Ctrl Pts',(15.4999999999999,13.6752954743877,3.8619999999999));
#28394=CARTESIAN_POINT('Ctrl Pts',(16.2901202367903,14.1314716057908,3.82033333333323));
#28395=CARTESIAN_POINT('Ctrl Pts',(17.0802404735807,14.5876477371939,3.77866666666657));
#28396=CARTESIAN_POINT('Ctrl Pts',(17.0802404735807,15.5000000000002,3.7369999999999));
#28397=CARTESIAN_POINT('Ctrl Pts',(17.0802404735807,16.4123522628064,3.69533333333323));
#28398=CARTESIAN_POINT('Ctrl Pts',(16.2901202367902,16.8685283942095,3.65366666666656));
#28399=CARTESIAN_POINT('Ctrl Pts',(15.4999999999998,17.3247045256126,3.6119999999999));
#28400=CARTESIAN_POINT('Ctrl Pts',(14.7098797632094,16.8685283942095,3.57033333333323));
#28401=CARTESIAN_POINT('Ctrl Pts',(13.919759526419,16.4123522628064,3.52866666666656));
#28402=CARTESIAN_POINT('Ctrl Pts',(13.919759526419,15.5000000000001,3.4869999999999));
#28403=CARTESIAN_POINT('Ctrl Pts',(13.919759526419,14.5876477371939,3.44533333333323));
#28404=CARTESIAN_POINT('Ctrl Pts',(14.7098797632094,14.1314716057908,3.40366666666656));
#28405=CARTESIAN_POINT('Ctrl Pts',(15.4999999999999,13.6752954743877,3.36199999999989));
#28406=CARTESIAN_POINT('Ctrl Pts',(16.2901202367903,14.1314716057908,3.32033333333323));
#28407=CARTESIAN_POINT('Ctrl Pts',(17.0802404735807,14.5876477371939,3.27866666666656));
#28408=CARTESIAN_POINT('Ctrl Pts',(17.0802404735807,15.5000000000002,3.23699999999989));
#28409=CARTESIAN_POINT('Ctrl Pts',(17.0802404735807,16.4123522628064,3.19533333333323));
#28410=CARTESIAN_POINT('Ctrl Pts',(16.2901202367902,16.8685283942095,3.15366666666656));
#28411=CARTESIAN_POINT('Ctrl Pts',(15.4999999999998,17.3247045256126,3.11199999999989));
#28412=CARTESIAN_POINT('Ctrl Pts',(14.7098797632094,16.8685283942095,3.07033333333322));
#28413=CARTESIAN_POINT('Ctrl Pts',(13.919759526419,16.4123522628064,3.02866666666656));
#28414=CARTESIAN_POINT('Ctrl Pts',(13.919759526419,15.5000000000001,2.98699999999989));
#28415=CARTESIAN_POINT('Ctrl Pts',(13.919759526419,14.5876477371939,2.94533333333322));
#28416=CARTESIAN_POINT('Ctrl Pts',(14.7098797632094,14.1314716057908,2.90366666666656));
#28417=CARTESIAN_POINT('Ctrl Pts',(15.4999999999999,13.6752954743877,2.86199999999989));
#28418=CARTESIAN_POINT('Ctrl Pts',(16.2901202367903,14.1314716057908,2.82033333333322));
#28419=CARTESIAN_POINT('Ctrl Pts',(17.0802404735807,14.5876477371939,2.77866666666655));
#28420=CARTESIAN_POINT('Ctrl Pts',(17.0802404735807,15.5000000000002,2.73699999999989));
#28421=CARTESIAN_POINT('Ctrl Pts',(17.0802404735807,16.4123522628064,2.69533333333322));
#28422=CARTESIAN_POINT('Ctrl Pts',(16.2901202367902,16.8685283942095,2.65366666666655));
#28423=CARTESIAN_POINT('Ctrl Pts',(15.4999999999998,17.3247045256126,2.61199999999988));
#28424=CARTESIAN_POINT('Ctrl Pts',(14.7098797632094,16.8685283942095,2.57033333333322));
#28425=CARTESIAN_POINT('Ctrl Pts',(13.919759526419,16.4123522628064,2.52866666666655));
#28426=CARTESIAN_POINT('Ctrl Pts',(13.919759526419,15.5000000000001,2.48699999999988));
#28427=CARTESIAN_POINT('Ctrl Pts',(13.919759526419,14.5876477371939,2.44533333333321));
#28428=CARTESIAN_POINT('Ctrl Pts',(14.7098797632094,14.1314716057908,2.40366666666655));
#28429=CARTESIAN_POINT('Ctrl Pts',(15.4999999999999,13.6752954743877,2.36199999999988));
#28430=CARTESIAN_POINT('Ctrl Pts',(16.2901202367903,14.1314716057908,2.32033333333321));
#28431=CARTESIAN_POINT('Ctrl Pts',(17.0802404735807,14.5876477371939,2.27866666666655));
#28432=CARTESIAN_POINT('Ctrl Pts',(17.0802404735807,15.5000000000002,2.23699999999988));
#28433=CARTESIAN_POINT('Ctrl Pts',(17.0802404735807,16.4123522628064,2.19533333333321));
#28434=CARTESIAN_POINT('Ctrl Pts',(16.2901202367902,16.8685283942095,2.15366666666655));
#28435=CARTESIAN_POINT('Ctrl Pts',(15.4999999999998,17.3247045256126,2.11199999999988));
#28436=CARTESIAN_POINT('Ctrl Pts',(14.7098797632094,16.8685283942095,2.07033333333321));
#28437=CARTESIAN_POINT('Ctrl Pts',(13.919759526419,16.4123522628064,2.02866666666654));
#28438=CARTESIAN_POINT('Ctrl Pts',(13.919759526419,15.5000000000001,1.98699999999988));
#28439=CARTESIAN_POINT('Ctrl Pts',(13.919759526419,14.5876477371939,1.94533333333321));
#28440=CARTESIAN_POINT('Ctrl Pts',(14.7098797632094,14.1314716057908,1.90366666666654));
#28441=CARTESIAN_POINT('Ctrl Pts',(15.4999999999999,13.6752954743877,1.86199999999987));
#28442=CARTESIAN_POINT('Ctrl Pts',(16.2901202367903,14.1314716057908,1.82033333333321));
#28443=CARTESIAN_POINT('Ctrl Pts',(17.0802404735807,14.5876477371939,1.77866666666654));
#28444=CARTESIAN_POINT('Ctrl Pts',(17.0802404735807,15.5000000000002,1.73699999999987));
#28445=CARTESIAN_POINT('Ctrl Pts',(17.0802404735807,16.4123522628064,1.6953333333332));
#28446=CARTESIAN_POINT('Ctrl Pts',(16.2901202367902,16.8685283942095,1.65366666666654));
#28447=CARTESIAN_POINT('Ctrl Pts',(15.4999999999998,17.3247045256126,1.61199999999987));
#28448=CARTESIAN_POINT('Ctrl Pts',(14.7098797632094,16.8685283942095,1.5703333333332));
#28449=CARTESIAN_POINT('Ctrl Pts',(13.919759526419,16.4123522628064,1.52866666666654));
#28450=CARTESIAN_POINT('Ctrl Pts',(13.919759526419,15.5000000000001,1.48699999999987));
#28451=CARTESIAN_POINT('Ctrl Pts',(13.919759526419,14.5876477371939,1.4453333333332));
#28452=CARTESIAN_POINT('Ctrl Pts',(14.7098797632094,14.1314716057908,1.40366666666653));
#28453=CARTESIAN_POINT('Ctrl Pts',(15.4999999999999,13.6752954743877,1.36199999999987));
#28454=CARTESIAN_POINT('Ctrl Pts',(16.2901202367903,14.1314716057908,1.3203333333332));
#28455=CARTESIAN_POINT('Ctrl Pts',(17.0802404735807,14.5876477371939,1.27866666666653));
#28456=CARTESIAN_POINT('Ctrl Pts',(17.0802404735807,15.5000000000002,1.23699999999987));
#28457=CARTESIAN_POINT('Ctrl Pts',(17.0802404735807,16.4123522628064,1.1953333333332));
#28458=CARTESIAN_POINT('Ctrl Pts',(16.2901202367902,16.8685283942095,1.15366666666653));
#28459=CARTESIAN_POINT('Ctrl Pts',(15.4999999999998,17.3247045256126,1.11199999999986));
#28460=CARTESIAN_POINT('Ctrl Pts',(14.7098797632094,16.8685283942095,1.0703333333332));
#28461=CARTESIAN_POINT('Ctrl Pts',(13.919759526419,16.4123522628064,1.02866666666653));
#28462=CARTESIAN_POINT('Ctrl Pts',(13.919759526419,15.5000000000001,0.986999999999863));
#28463=CARTESIAN_POINT('Ctrl Pts',(13.919759526419,14.5876477371939,0.945333333333196));
#28464=CARTESIAN_POINT('Ctrl Pts',(14.7098797632094,14.1314716057908,0.903666666666529));
#28465=CARTESIAN_POINT('Ctrl Pts',(15.4999999999999,13.6752954743877,0.861999999999861));
#28466=CARTESIAN_POINT('Ctrl Pts',(16.2901202367903,14.1314716057908,0.820333333333194));
#28467=CARTESIAN_POINT('Ctrl Pts',(17.0802404735807,14.5876477371939,0.778666666666527));
#28468=CARTESIAN_POINT('Ctrl Pts',(17.0802404735807,15.5000000000002,0.736999999999859));
#28469=CARTESIAN_POINT('Ctrl Pts',(17.0802404735807,16.4123522628064,0.695333333333192));
#28470=CARTESIAN_POINT('Ctrl Pts',(16.2901202367902,16.8685283942095,0.653666666666525));
#28471=CARTESIAN_POINT('Ctrl Pts',(15.4999999999998,17.3247045256126,0.611999999999858));
#28472=CARTESIAN_POINT('Ctrl Pts',(14.7098797632094,16.8685283942095,0.57033333333319));
#28473=CARTESIAN_POINT('Ctrl Pts',(13.919759526419,16.4123522628064,0.528666666666523));
#28474=CARTESIAN_POINT('Ctrl Pts',(13.919759526419,15.5000000000001,0.486999999999856));
#28475=CARTESIAN_POINT('Ctrl Pts',(13.919759526419,14.5876477371939,0.445333333333188));
#28476=CARTESIAN_POINT('Ctrl Pts',(14.7098797632094,14.1314716057908,0.403666666666521));
#28477=CARTESIAN_POINT('Ctrl Pts',(15.4999999999999,13.6752954743877,0.361999999999854));
#28478=CARTESIAN_POINT('Ctrl Pts',(16.2901202367903,14.1314716057908,0.320333333333186));
#28479=CARTESIAN_POINT('Ctrl Pts',(17.0802404735807,14.5876477371939,0.278666666666519));
#28480=CARTESIAN_POINT('Ctrl Pts',(17.0802404735807,15.5000000000002,0.236999999999852));
#28481=CARTESIAN_POINT('Ctrl Pts',(17.0802404735807,16.4123522628064,0.195333333333185));
#28482=CARTESIAN_POINT('Ctrl Pts',(16.2901202367902,16.8685283942095,0.153666666666517));
#28483=CARTESIAN_POINT('Ctrl Pts',(15.4999999999998,17.3247045256126,0.11199999999985));
#28484=CARTESIAN_POINT('Ctrl Pts',(14.7098797632094,16.8685283942095,0.0703333333331828));
#28485=CARTESIAN_POINT('Ctrl Pts',(13.919759526419,16.4123522628064,0.0286666666665155));
#28486=CARTESIAN_POINT('Ctrl Pts',(13.919759526419,15.5000000000001,-0.0130000000001518));
#28487=CARTESIAN_POINT('Ctrl Pts',(13.919759526419,14.5876477371939,-0.0546666666668173));
#28488=CARTESIAN_POINT('Ctrl Pts',(14.7098797632094,14.1314716057908,-0.0963333333334846));
#28489=CARTESIAN_POINT('Ctrl Pts',(15.4999999999999,13.6752954743877,-0.138000000000152));
#28490=CARTESIAN_POINT('Ctrl Pts',(16.2901202367903,14.1314716057908,-0.179666666666819));
#28491=CARTESIAN_POINT('Ctrl Pts',(17.0802404735807,14.5876477371939,-0.221333333333486));
#28492=CARTESIAN_POINT('Ctrl Pts',(17.0802404735807,15.5000000000002,-0.263000000000154));
#28493=CARTESIAN_POINT('Ctrl Pts',(17.0802404735807,16.4123522628064,-0.304666666666821));
#28494=CARTESIAN_POINT('Ctrl Pts',(16.2901202367902,16.8685283942095,-0.346333333333488));
#28495=CARTESIAN_POINT('Ctrl Pts',(15.4999999999998,17.3247045256126,-0.388000000000156));
#28496=CARTESIAN_POINT('Ctrl Pts',(14.7098797632094,16.8685283942095,-0.429666666666823));
#28497=CARTESIAN_POINT('Ctrl Pts',(13.919759526419,16.4123522628064,-0.47133333333349));
#28498=CARTESIAN_POINT('Ctrl Pts',(13.919759526419,15.5000000000001,-0.513000000000157));
#28499=CARTESIAN_POINT('Ctrl Pts',(13.919759526419,14.5876477371939,-0.554666666666825));
#28500=CARTESIAN_POINT('Ctrl Pts',(14.7098797632094,14.1314716057908,-0.596333333333492));
#28501=CARTESIAN_POINT('Ctrl Pts',(15.4999999999999,13.6752954743877,-0.638000000000159));
#28502=CARTESIAN_POINT('Ctrl Pts',(16.2901202367903,14.1314716057908,-0.679666666666827));
#28503=CARTESIAN_POINT('Ctrl Pts',(17.0802404735807,14.5876477371939,-0.721333333333494));
#28504=CARTESIAN_POINT('Ctrl Pts',(17.0802404735807,15.5000000000002,-0.763000000000161));
#28505=CARTESIAN_POINT('Ctrl Pts',(17.0802404735807,16.4123522628064,-0.804666666666829));
#28506=CARTESIAN_POINT('Ctrl Pts',(16.2901202367902,16.8685283942095,-0.846333333333496));
#28507=CARTESIAN_POINT('Ctrl Pts',(15.4999999999998,17.3247045256126,-0.888000000000163));
#28508=CARTESIAN_POINT('Ctrl Pts',(14.7098797632094,16.8685283942095,-0.92966666666683));
#28509=CARTESIAN_POINT('Ctrl Pts',(13.919759526419,16.4123522628064,-0.971333333333498));
#28510=CARTESIAN_POINT('Ctrl Pts',(13.919759526419,15.5000000000001,-1.01300000000016));
#28511=CARTESIAN_POINT('Ctrl Pts',(13.919759526419,14.5876477371939,-1.05466666666683));
#28512=CARTESIAN_POINT('Ctrl Pts',(14.7098797632094,14.1314716057908,-1.0963333333335));
#28513=CARTESIAN_POINT('Ctrl Pts',(15.4999999999999,13.6752954743877,-1.13800000000017));
#28514=CARTESIAN_POINT('Ctrl Pts',(16.2901202367903,14.1314716057908,-1.17966666666683));
#28515=CARTESIAN_POINT('Ctrl Pts',(17.0802404735807,14.5876477371939,-1.2213333333335));
#28516=CARTESIAN_POINT('Ctrl Pts',(17.0802404735807,15.5000000000002,-1.26300000000017));
#28517=CARTESIAN_POINT('Ctrl Pts',(17.0802404735807,16.4123522628064,-1.30466666666683));
#28518=CARTESIAN_POINT('Ctrl Pts',(16.2901202367902,16.8685283942095,-1.3463333333335));
#28519=CARTESIAN_POINT('Ctrl Pts',(15.4999999999998,17.3247045256126,-1.38800000000017));
#28520=CARTESIAN_POINT('Ctrl Pts',(14.7098797632094,16.8685283942095,-1.42966666666684));
#28521=CARTESIAN_POINT('Ctrl Pts',(13.919759526419,16.4123522628064,-1.4713333333335));
#28522=CARTESIAN_POINT('Ctrl Pts',(13.919759526419,15.5000000000001,-1.51300000000017));
#28523=CARTESIAN_POINT('Ctrl Pts',(13.919759526419,14.5876477371939,-1.55466666666684));
#28524=CARTESIAN_POINT('Ctrl Pts',(14.7098797632094,14.1314716057908,-1.59633333333351));
#28525=CARTESIAN_POINT('Ctrl Pts',(15.4999999999999,13.6752954743877,-1.63800000000017));
#28526=CARTESIAN_POINT('Ctrl Pts',(16.2901202367903,14.1314716057908,-1.67966666666684));
#28527=CARTESIAN_POINT('Ctrl Pts',(17.0802404735807,14.5876477371939,-1.72133333333351));
#28528=CARTESIAN_POINT('Ctrl Pts',(17.0802404735807,15.5000000000002,-1.76300000000017));
#28529=CARTESIAN_POINT('Ctrl Pts',(17.0802404735807,16.4123522628064,-1.80466666666684));
#28530=CARTESIAN_POINT('Ctrl Pts',(16.2901202367902,16.8685283942095,-1.84633333333351));
#28531=CARTESIAN_POINT('Ctrl Pts',(15.4999999999998,17.3247045256126,-1.88800000000018));
#28532=CARTESIAN_POINT('Ctrl Pts',(14.7098797632094,16.8685283942095,-1.92966666666684));
#28533=CARTESIAN_POINT('Ctrl Pts',(14.4189900731897,16.7005831533722,-1.94500661517905));
#28534=CARTESIAN_POINT('Ctrl Pts',(14.221552772606,16.4288340223701,-1.96262314816781));
#28535=CARTESIAN_POINT('Origin',(14.0080754615184,16.5839252605848,-2.17746715486548));
#28536=CARTESIAN_POINT('',(14.2215498957102,16.428830062579,-2.02512301642217));
#28537=CARTESIAN_POINT('Ctrl Pts',(17.0802404735807,15.5000000000002,11.2370201234482));
#28538=CARTESIAN_POINT('Ctrl Pts',(17.0802404735807,16.4123522628064,11.1953534567815));
#28539=CARTESIAN_POINT('Ctrl Pts',(16.2901202367902,16.8685283942095,11.1536867901149));
#28540=CARTESIAN_POINT('Ctrl Pts',(15.4999999999998,17.3247045256126,11.1120201234482));
#28541=CARTESIAN_POINT('Ctrl Pts',(14.7098797632094,16.8685283942095,11.0703534567815));
#28542=CARTESIAN_POINT('Ctrl Pts',(13.919759526419,16.4123522628064,11.0286867901149));
#28543=CARTESIAN_POINT('Ctrl Pts',(13.919759526419,15.5000000000001,10.9870201234482));
#28544=CARTESIAN_POINT('Ctrl Pts',(13.919759526419,14.5876477371939,10.9453534567815));
#28545=CARTESIAN_POINT('Ctrl Pts',(14.7098797632094,14.1314716057908,10.9036867901149));
#28546=CARTESIAN_POINT('Ctrl Pts',(15.4999999999999,13.6752954743877,10.8620201234482));
#28547=CARTESIAN_POINT('Ctrl Pts',(16.2901202367903,14.1314716057908,10.8203534567815));
#28548=CARTESIAN_POINT('Ctrl Pts',(17.0802404735807,14.5876477371939,10.7786867901149));
#28549=CARTESIAN_POINT('Ctrl Pts',(17.0802404735807,15.5000000000002,10.7370201234482));
#28550=CARTESIAN_POINT('Ctrl Pts',(17.0802404735807,16.4123522628064,10.6953534567815));
#28551=CARTESIAN_POINT('Ctrl Pts',(16.2901202367902,16.8685283942095,10.6536867901149));
#28552=CARTESIAN_POINT('Ctrl Pts',(15.4999999999998,17.3247045256126,10.6120201234482));
#28553=CARTESIAN_POINT('Ctrl Pts',(14.7098797632094,16.8685283942095,10.5703534567815));
#28554=CARTESIAN_POINT('Ctrl Pts',(13.919759526419,16.4123522628064,10.5286867901149));
#28555=CARTESIAN_POINT('Ctrl Pts',(13.919759526419,15.5000000000001,10.4870201234482));
#28556=CARTESIAN_POINT('Ctrl Pts',(13.919759526419,14.5876477371939,10.4453534567815));
#28557=CARTESIAN_POINT('Ctrl Pts',(14.7098797632094,14.1314716057908,10.4036867901149));
#28558=CARTESIAN_POINT('Ctrl Pts',(15.4999999999999,13.6752954743877,10.3620201234482));
#28559=CARTESIAN_POINT('Ctrl Pts',(16.2901202367903,14.1314716057908,10.3203534567815));
#28560=CARTESIAN_POINT('Ctrl Pts',(17.0802404735807,14.5876477371939,10.2786867901149));
#28561=CARTESIAN_POINT('Ctrl Pts',(17.0802404735807,15.5000000000002,10.2370201234482));
#28562=CARTESIAN_POINT('Ctrl Pts',(17.0802404735807,16.4123522628064,10.1953534567815));
#28563=CARTESIAN_POINT('Ctrl Pts',(16.2901202367902,16.8685283942095,10.1536867901149));
#28564=CARTESIAN_POINT('Ctrl Pts',(15.4999999999998,17.3247045256126,10.1120201234482));
#28565=CARTESIAN_POINT('Ctrl Pts',(14.7098797632094,16.8685283942095,10.0703534567815));
#28566=CARTESIAN_POINT('Ctrl Pts',(13.919759526419,16.4123522628064,10.0286867901149));
#28567=CARTESIAN_POINT('Ctrl Pts',(13.919759526419,15.5000000000001,9.98702012344819));
#28568=CARTESIAN_POINT('Ctrl Pts',(13.919759526419,14.5876477371939,9.94535345678152));
#28569=CARTESIAN_POINT('Ctrl Pts',(14.7098797632094,14.1314716057908,9.90368679011485));
#28570=CARTESIAN_POINT('Ctrl Pts',(15.4999999999999,13.6752954743877,9.86202012344818));
#28571=CARTESIAN_POINT('Ctrl Pts',(16.2901202367903,14.1314716057908,9.82035345678152));
#28572=CARTESIAN_POINT('Ctrl Pts',(17.0802404735807,14.5876477371939,9.77868679011485));
#28573=CARTESIAN_POINT('Ctrl Pts',(17.0802404735807,15.5000000000002,9.73702012344818));
#28574=CARTESIAN_POINT('Ctrl Pts',(17.0802404735807,16.4123522628064,9.69535345678151));
#28575=CARTESIAN_POINT('Ctrl Pts',(16.2901202367902,16.8685283942095,9.65368679011485));
#28576=CARTESIAN_POINT('Ctrl Pts',(15.4999999999998,17.3247045256126,9.61202012344818));
#28577=CARTESIAN_POINT('Ctrl Pts',(14.7098797632094,16.8685283942095,9.57035345678151));
#28578=CARTESIAN_POINT('Ctrl Pts',(13.919759526419,16.4123522628064,9.52868679011484));
#28579=CARTESIAN_POINT('Ctrl Pts',(13.919759526419,15.5000000000001,9.48702012344818));
#28580=CARTESIAN_POINT('Ctrl Pts',(13.919759526419,14.5876477371939,9.44535345678151));
#28581=CARTESIAN_POINT('Ctrl Pts',(14.7098797632094,14.1314716057908,9.40368679011484));
#28582=CARTESIAN_POINT('Ctrl Pts',(15.4999999999999,13.6752954743877,9.36202012344818));
#28583=CARTESIAN_POINT('Ctrl Pts',(16.2901202367903,14.1314716057908,9.32035345678151));
#28584=CARTESIAN_POINT('Ctrl Pts',(17.0802404735807,14.5876477371939,9.27868679011484));
#28585=CARTESIAN_POINT('Ctrl Pts',(17.0802404735807,15.5000000000002,9.23702012344818));
#28586=CARTESIAN_POINT('Ctrl Pts',(17.0802404735807,16.4123522628064,9.19535345678151));
#28587=CARTESIAN_POINT('Ctrl Pts',(16.2901202367902,16.8685283942095,9.15368679011484));
#28588=CARTESIAN_POINT('Ctrl Pts',(15.4999999999998,17.3247045256126,9.11202012344818));
#28589=CARTESIAN_POINT('Ctrl Pts',(14.7098797632094,16.8685283942095,9.07035345678151));
#28590=CARTESIAN_POINT('Ctrl Pts',(13.919759526419,16.4123522628064,9.02868679011484));
#28591=CARTESIAN_POINT('Ctrl Pts',(13.919759526419,15.5000000000001,8.98702012344817));
#28592=CARTESIAN_POINT('Ctrl Pts',(13.919759526419,14.5876477371939,8.94535345678151));
#28593=CARTESIAN_POINT('Ctrl Pts',(14.7098797632094,14.1314716057908,8.90368679011484));
#28594=CARTESIAN_POINT('Ctrl Pts',(15.4999999999999,13.6752954743877,8.86202012344817));
#28595=CARTESIAN_POINT('Ctrl Pts',(16.2901202367903,14.1314716057908,8.8203534567815));
#28596=CARTESIAN_POINT('Ctrl Pts',(17.0802404735807,14.5876477371939,8.77868679011484));
#28597=CARTESIAN_POINT('Ctrl Pts',(17.0802404735807,15.5000000000002,8.73702012344817));
#28598=CARTESIAN_POINT('Ctrl Pts',(17.0802404735807,16.4123522628064,8.6953534567815));
#28599=CARTESIAN_POINT('Ctrl Pts',(16.2901202367902,16.8685283942095,8.65368679011483));
#28600=CARTESIAN_POINT('Ctrl Pts',(15.4999999999998,17.3247045256126,8.61202012344817));
#28601=CARTESIAN_POINT('Ctrl Pts',(14.7098797632094,16.8685283942095,8.5703534567815));
#28602=CARTESIAN_POINT('Ctrl Pts',(13.919759526419,16.4123522628064,8.52868679011483));
#28603=CARTESIAN_POINT('Ctrl Pts',(13.919759526419,15.5000000000001,8.48702012344816));
#28604=CARTESIAN_POINT('Ctrl Pts',(13.919759526419,14.5876477371939,8.4453534567815));
#28605=CARTESIAN_POINT('Ctrl Pts',(14.7098797632094,14.1314716057908,8.40368679011483));
#28606=CARTESIAN_POINT('Ctrl Pts',(15.4999999999999,13.6752954743877,8.36202012344816));
#28607=CARTESIAN_POINT('Ctrl Pts',(16.2901202367903,14.1314716057908,8.3203534567815));
#28608=CARTESIAN_POINT('Ctrl Pts',(17.0802404735807,14.5876477371939,8.27868679011483));
#28609=CARTESIAN_POINT('Ctrl Pts',(17.0802404735807,15.5000000000002,8.23702012344816));
#28610=CARTESIAN_POINT('Ctrl Pts',(17.0802404735807,16.4123522628064,8.1953534567815));
#28611=CARTESIAN_POINT('Ctrl Pts',(16.2901202367902,16.8685283942095,8.15368679011483));
#28612=CARTESIAN_POINT('Ctrl Pts',(15.4999999999998,17.3247045256126,8.11202012344816));
#28613=CARTESIAN_POINT('Ctrl Pts',(14.7098797632094,16.8685283942095,8.07035345678149));
#28614=CARTESIAN_POINT('Ctrl Pts',(13.919759526419,16.4123522628064,8.02868679011483));
#28615=CARTESIAN_POINT('Ctrl Pts',(13.919759526419,15.5000000000001,7.98702012344816));
#28616=CARTESIAN_POINT('Ctrl Pts',(13.919759526419,14.5876477371939,7.94535345678149));
#28617=CARTESIAN_POINT('Ctrl Pts',(14.7098797632094,14.1314716057908,7.90368679011482));
#28618=CARTESIAN_POINT('Ctrl Pts',(15.4999999999999,13.6752954743877,7.86202012344816));
#28619=CARTESIAN_POINT('Ctrl Pts',(16.2901202367903,14.1314716057908,7.82035345678149));
#28620=CARTESIAN_POINT('Ctrl Pts',(17.0802404735807,14.5876477371939,7.77868679011482));
#28621=CARTESIAN_POINT('Ctrl Pts',(17.0802404735807,15.5000000000002,7.73702012344816));
#28622=CARTESIAN_POINT('Ctrl Pts',(17.0802404735807,16.4123522628064,7.69535345678149));
#28623=CARTESIAN_POINT('Ctrl Pts',(16.2901202367902,16.8685283942095,7.65368679011482));
#28624=CARTESIAN_POINT('Ctrl Pts',(15.4999999999998,17.3247045256126,7.61202012344815));
#28625=CARTESIAN_POINT('Ctrl Pts',(14.7098797632094,16.8685283942095,7.57035345678149));
#28626=CARTESIAN_POINT('Ctrl Pts',(13.919759526419,16.4123522628064,7.52868679011482));
#28627=CARTESIAN_POINT('Ctrl Pts',(13.919759526419,15.5000000000001,7.48702012344815));
#28628=CARTESIAN_POINT('Ctrl Pts',(13.919759526419,14.5876477371939,7.44535345678148));
#28629=CARTESIAN_POINT('Ctrl Pts',(14.7098797632094,14.1314716057908,7.40368679011482));
#28630=CARTESIAN_POINT('Ctrl Pts',(15.4999999999999,13.6752954743877,7.36202012344815));
#28631=CARTESIAN_POINT('Ctrl Pts',(16.2901202367903,14.1314716057908,7.32035345678148));
#28632=CARTESIAN_POINT('Ctrl Pts',(17.0802404735807,14.5876477371939,7.27868679011482));
#28633=CARTESIAN_POINT('Ctrl Pts',(17.0802404735807,15.5000000000002,7.23702012344815));
#28634=CARTESIAN_POINT('Ctrl Pts',(17.0802404735807,16.4123522628064,7.19535345678148));
#28635=CARTESIAN_POINT('Ctrl Pts',(16.2901202367902,16.8685283942095,7.15368679011481));
#28636=CARTESIAN_POINT('Ctrl Pts',(15.4999999999998,17.3247045256126,7.11202012344815));
#28637=CARTESIAN_POINT('Ctrl Pts',(14.7098797632094,16.8685283942095,7.07035345678148));
#28638=CARTESIAN_POINT('Ctrl Pts',(13.919759526419,16.4123522628064,7.02868679011481));
#28639=CARTESIAN_POINT('Ctrl Pts',(13.919759526419,15.5000000000001,6.98702012344815));
#28640=CARTESIAN_POINT('Ctrl Pts',(13.919759526419,14.5876477371939,6.94535345678148));
#28641=CARTESIAN_POINT('Ctrl Pts',(14.7098797632094,14.1314716057908,6.90368679011481));
#28642=CARTESIAN_POINT('Ctrl Pts',(15.4999999999999,13.6752954743877,6.86202012344814));
#28643=CARTESIAN_POINT('Ctrl Pts',(16.2901202367903,14.1314716057908,6.82035345678148));
#28644=CARTESIAN_POINT('Ctrl Pts',(17.0802404735807,14.5876477371939,6.77868679011481));
#28645=CARTESIAN_POINT('Ctrl Pts',(17.0802404735807,15.5000000000002,6.73702012344814));
#28646=CARTESIAN_POINT('Ctrl Pts',(17.0802404735807,16.4123522628064,6.69535345678147));
#28647=CARTESIAN_POINT('Ctrl Pts',(16.2901202367902,16.8685283942095,6.65368679011481));
#28648=CARTESIAN_POINT('Ctrl Pts',(15.4999999999998,17.3247045256126,6.61202012344814));
#28649=CARTESIAN_POINT('Ctrl Pts',(14.7098797632094,16.8685283942095,6.57035345678147));
#28650=CARTESIAN_POINT('Ctrl Pts',(13.919759526419,16.4123522628064,6.52868679011481));
#28651=CARTESIAN_POINT('Ctrl Pts',(13.919759526419,15.5000000000001,6.48702012344814));
#28652=CARTESIAN_POINT('Ctrl Pts',(13.919759526419,14.5876477371939,6.44535345678147));
#28653=CARTESIAN_POINT('Ctrl Pts',(14.7098797632094,14.1314716057908,6.40368679011481));
#28654=CARTESIAN_POINT('Ctrl Pts',(15.4999999999999,13.6752954743877,6.36202012344814));
#28655=CARTESIAN_POINT('Ctrl Pts',(16.2901202367903,14.1314716057908,6.32035345678147));
#28656=CARTESIAN_POINT('Ctrl Pts',(17.0802404735807,14.5876477371939,6.2786867901148));
#28657=CARTESIAN_POINT('Ctrl Pts',(17.0802404735807,15.5000000000002,6.23702012344813));
#28658=CARTESIAN_POINT('Ctrl Pts',(17.0802404735807,16.4123522628064,6.19535345678147));
#28659=CARTESIAN_POINT('Ctrl Pts',(16.2901202367902,16.8685283942095,6.1536867901148));
#28660=CARTESIAN_POINT('Ctrl Pts',(15.4999999999998,17.3247045256126,6.11202012344813));
#28661=CARTESIAN_POINT('Ctrl Pts',(14.7098797632094,16.8685283942095,6.07035345678146));
#28662=CARTESIAN_POINT('Ctrl Pts',(13.919759526419,16.4123522628064,6.0286867901148));
#28663=CARTESIAN_POINT('Ctrl Pts',(13.919759526419,15.5000000000001,5.98702012344813));
#28664=CARTESIAN_POINT('Ctrl Pts',(13.919759526419,14.5876477371939,5.94535345678146));
#28665=CARTESIAN_POINT('Ctrl Pts',(14.7098797632094,14.1314716057908,5.9036867901148));
#28666=CARTESIAN_POINT('Ctrl Pts',(15.4999999999999,13.6752954743877,5.86202012344813));
#28667=CARTESIAN_POINT('Ctrl Pts',(16.2901202367903,14.1314716057908,5.82035345678146));
#28668=CARTESIAN_POINT('Ctrl Pts',(17.0802404735807,14.5876477371939,5.7786867901148));
#28669=CARTESIAN_POINT('Ctrl Pts',(17.0802404735807,15.5000000000002,5.73702012344813));
#28670=CARTESIAN_POINT('Ctrl Pts',(17.0802404735807,16.4123522628064,5.69535345678146));
#28671=CARTESIAN_POINT('Ctrl Pts',(16.2901202367902,16.8685283942095,5.65368679011479));
#28672=CARTESIAN_POINT('Ctrl Pts',(15.4999999999998,17.3247045256126,5.61202012344813));
#28673=CARTESIAN_POINT('Ctrl Pts',(14.7098797632094,16.8685283942095,5.57035345678146));
#28674=CARTESIAN_POINT('Ctrl Pts',(13.919759526419,16.4123522628064,5.52868679011479));
#28675=CARTESIAN_POINT('Ctrl Pts',(13.919759526419,15.5000000000001,5.48702012344813));
#28676=CARTESIAN_POINT('Ctrl Pts',(13.919759526419,14.5876477371939,5.44535345678146));
#28677=CARTESIAN_POINT('Ctrl Pts',(14.7098797632094,14.1314716057908,5.40368679011479));
#28678=CARTESIAN_POINT('Ctrl Pts',(15.4999999999999,13.6752954743877,5.36202012344812));
#28679=CARTESIAN_POINT('Ctrl Pts',(16.2901202367903,14.1314716057908,5.32035345678146));
#28680=CARTESIAN_POINT('Ctrl Pts',(17.0802404735807,14.5876477371939,5.27868679011479));
#28681=CARTESIAN_POINT('Ctrl Pts',(17.0802404735807,15.5000000000002,5.23702012344812));
#28682=CARTESIAN_POINT('Ctrl Pts',(17.0802404735807,16.4123522628064,5.19535345678145));
#28683=CARTESIAN_POINT('Ctrl Pts',(16.2901202367902,16.8685283942095,5.15368679011479));
#28684=CARTESIAN_POINT('Ctrl Pts',(15.4999999999998,17.3247045256126,5.11202012344812));
#28685=CARTESIAN_POINT('Ctrl Pts',(14.7098797632094,16.8685283942095,5.07035345678145));
#28686=CARTESIAN_POINT('Ctrl Pts',(13.919759526419,16.4123522628064,5.02868679011479));
#28687=CARTESIAN_POINT('Ctrl Pts',(13.919759526419,15.5000000000001,4.98702012344812));
#28688=CARTESIAN_POINT('Ctrl Pts',(13.919759526419,14.5876477371939,4.94535345678145));
#28689=CARTESIAN_POINT('Ctrl Pts',(14.7098797632094,14.1314716057908,4.90368679011478));
#28690=CARTESIAN_POINT('Ctrl Pts',(15.4999999999999,13.6752954743877,4.86202012344812));
#28691=CARTESIAN_POINT('Ctrl Pts',(16.2901202367903,14.1314716057908,4.82035345678145));
#28692=CARTESIAN_POINT('Ctrl Pts',(17.0802404735807,14.5876477371939,4.77868679011478));
#28693=CARTESIAN_POINT('Ctrl Pts',(17.0802404735807,15.5000000000002,4.73702012344812));
#28694=CARTESIAN_POINT('Ctrl Pts',(17.0802404735807,16.4123522628064,4.69535345678145));
#28695=CARTESIAN_POINT('Ctrl Pts',(16.2901202367902,16.8685283942095,4.65368679011478));
#28696=CARTESIAN_POINT('Ctrl Pts',(15.4999999999998,17.3247045256126,4.61202012344811));
#28697=CARTESIAN_POINT('Ctrl Pts',(14.7098797632094,16.8685283942095,4.57035345678145));
#28698=CARTESIAN_POINT('Ctrl Pts',(13.919759526419,16.4123522628064,4.52868679011478));
#28699=CARTESIAN_POINT('Ctrl Pts',(13.919759526419,15.5000000000001,4.48702012344811));
#28700=CARTESIAN_POINT('Ctrl Pts',(13.919759526419,14.5876477371939,4.44535345678144));
#28701=CARTESIAN_POINT('Ctrl Pts',(14.7098797632094,14.1314716057908,4.40368679011478));
#28702=CARTESIAN_POINT('Ctrl Pts',(15.4999999999999,13.6752954743877,4.36202012344811));
#28703=CARTESIAN_POINT('Ctrl Pts',(16.2901202367903,14.1314716057908,4.32035345678144));
#28704=CARTESIAN_POINT('Ctrl Pts',(17.0802404735807,14.5876477371939,4.27868679011477));
#28705=CARTESIAN_POINT('Ctrl Pts',(17.0802404735807,15.5000000000002,4.23702012344811));
#28706=CARTESIAN_POINT('Ctrl Pts',(17.0802404735807,16.4123522628064,4.19535345678144));
#28707=CARTESIAN_POINT('Ctrl Pts',(16.2901202367902,16.8685283942095,4.15368679011477));
#28708=CARTESIAN_POINT('Ctrl Pts',(15.4999999999998,17.3247045256126,4.11202012344811));
#28709=CARTESIAN_POINT('Ctrl Pts',(14.7098797632094,16.8685283942095,4.07035345678144));
#28710=CARTESIAN_POINT('Ctrl Pts',(13.919759526419,16.4123522628064,4.02868679011477));
#28711=CARTESIAN_POINT('Ctrl Pts',(13.919759526419,15.5000000000001,3.9870201234481));
#28712=CARTESIAN_POINT('Ctrl Pts',(13.919759526419,14.5876477371939,3.94535345678144));
#28713=CARTESIAN_POINT('Ctrl Pts',(14.7098797632094,14.1314716057908,3.90368679011477));
#28714=CARTESIAN_POINT('Ctrl Pts',(15.4999999999999,13.6752954743877,3.8620201234481));
#28715=CARTESIAN_POINT('Ctrl Pts',(16.2901202367903,14.1314716057908,3.82035345678144));
#28716=CARTESIAN_POINT('Ctrl Pts',(17.0802404735807,14.5876477371939,3.77868679011477));
#28717=CARTESIAN_POINT('Ctrl Pts',(17.0802404735807,15.5000000000002,3.7370201234481));
#28718=CARTESIAN_POINT('Ctrl Pts',(17.0802404735807,16.4123522628064,3.69535345678143));
#28719=CARTESIAN_POINT('Ctrl Pts',(16.2901202367902,16.8685283942095,3.65368679011477));
#28720=CARTESIAN_POINT('Ctrl Pts',(15.4999999999998,17.3247045256126,3.6120201234481));
#28721=CARTESIAN_POINT('Ctrl Pts',(14.7098797632094,16.8685283942095,3.57035345678143));
#28722=CARTESIAN_POINT('Ctrl Pts',(13.919759526419,16.4123522628064,3.52868679011477));
#28723=CARTESIAN_POINT('Ctrl Pts',(13.919759526419,15.5000000000001,3.4870201234481));
#28724=CARTESIAN_POINT('Ctrl Pts',(13.919759526419,14.5876477371939,3.44535345678143));
#28725=CARTESIAN_POINT('Ctrl Pts',(14.7098797632094,14.1314716057908,3.40368679011476));
#28726=CARTESIAN_POINT('Ctrl Pts',(15.4999999999999,13.6752954743877,3.3620201234481));
#28727=CARTESIAN_POINT('Ctrl Pts',(16.2901202367903,14.1314716057908,3.32035345678143));
#28728=CARTESIAN_POINT('Ctrl Pts',(17.0802404735807,14.5876477371939,3.27868679011476));
#28729=CARTESIAN_POINT('Ctrl Pts',(17.0802404735807,15.5000000000002,3.2370201234481));
#28730=CARTESIAN_POINT('Ctrl Pts',(17.0802404735807,16.4123522628064,3.19535345678143));
#28731=CARTESIAN_POINT('Ctrl Pts',(16.2901202367902,16.8685283942095,3.15368679011476));
#28732=CARTESIAN_POINT('Ctrl Pts',(15.4999999999998,17.3247045256126,3.11202012344809));
#28733=CARTESIAN_POINT('Ctrl Pts',(14.7098797632094,16.8685283942095,3.07035345678143));
#28734=CARTESIAN_POINT('Ctrl Pts',(13.919759526419,16.4123522628064,3.02868679011476));
#28735=CARTESIAN_POINT('Ctrl Pts',(13.919759526419,15.5000000000001,2.98702012344809));
#28736=CARTESIAN_POINT('Ctrl Pts',(13.919759526419,14.5876477371939,2.94535345678143));
#28737=CARTESIAN_POINT('Ctrl Pts',(14.7098797632094,14.1314716057908,2.90368679011476));
#28738=CARTESIAN_POINT('Ctrl Pts',(15.4999999999999,13.6752954743877,2.86202012344809));
#28739=CARTESIAN_POINT('Ctrl Pts',(16.2901202367903,14.1314716057908,2.82035345678142));
#28740=CARTESIAN_POINT('Ctrl Pts',(17.0802404735807,14.5876477371939,2.77868679011476));
#28741=CARTESIAN_POINT('Ctrl Pts',(17.0802404735807,15.5000000000002,2.73702012344809));
#28742=CARTESIAN_POINT('Ctrl Pts',(17.0802404735807,16.4123522628064,2.69535345678142));
#28743=CARTESIAN_POINT('Ctrl Pts',(16.2901202367902,16.8685283942095,2.65368679011475));
#28744=CARTESIAN_POINT('Ctrl Pts',(15.4999999999998,17.3247045256126,2.61202012344809));
#28745=CARTESIAN_POINT('Ctrl Pts',(14.7098797632094,16.8685283942095,2.57035345678142));
#28746=CARTESIAN_POINT('Ctrl Pts',(13.919759526419,16.4123522628064,2.52868679011475));
#28747=CARTESIAN_POINT('Ctrl Pts',(13.919759526419,15.5000000000001,2.48702012344808));
#28748=CARTESIAN_POINT('Ctrl Pts',(13.919759526419,14.5876477371939,2.44535345678142));
#28749=CARTESIAN_POINT('Ctrl Pts',(14.7098797632094,14.1314716057908,2.40368679011475));
#28750=CARTESIAN_POINT('Ctrl Pts',(15.4999999999999,13.6752954743877,2.36202012344808));
#28751=CARTESIAN_POINT('Ctrl Pts',(16.2901202367903,14.1314716057908,2.32035345678142));
#28752=CARTESIAN_POINT('Ctrl Pts',(17.0802404735807,14.5876477371939,2.27868679011475));
#28753=CARTESIAN_POINT('Ctrl Pts',(17.0802404735807,15.5000000000002,2.23702012344808));
#28754=CARTESIAN_POINT('Ctrl Pts',(17.0802404735807,16.4123522628064,2.19535345678142));
#28755=CARTESIAN_POINT('Ctrl Pts',(16.2901202367902,16.8685283942095,2.15368679011475));
#28756=CARTESIAN_POINT('Ctrl Pts',(15.4999999999998,17.3247045256126,2.11202012344808));
#28757=CARTESIAN_POINT('Ctrl Pts',(14.7098797632094,16.8685283942095,2.07035345678141));
#28758=CARTESIAN_POINT('Ctrl Pts',(13.919759526419,16.4123522628064,2.02868679011475));
#28759=CARTESIAN_POINT('Ctrl Pts',(13.919759526419,15.5000000000001,1.98702012344808));
#28760=CARTESIAN_POINT('Ctrl Pts',(13.919759526419,14.5876477371939,1.94535345678141));
#28761=CARTESIAN_POINT('Ctrl Pts',(14.7098797632094,14.1314716057908,1.90368679011474));
#28762=CARTESIAN_POINT('Ctrl Pts',(15.4999999999999,13.6752954743877,1.86202012344808));
#28763=CARTESIAN_POINT('Ctrl Pts',(16.2901202367903,14.1314716057908,1.82035345678141));
#28764=CARTESIAN_POINT('Ctrl Pts',(17.0802404735807,14.5876477371939,1.77868679011474));
#28765=CARTESIAN_POINT('Ctrl Pts',(17.0802404735807,15.5000000000002,1.73702012344808));
#28766=CARTESIAN_POINT('Ctrl Pts',(17.0802404735807,16.4123522628064,1.69535345678141));
#28767=CARTESIAN_POINT('Ctrl Pts',(16.2901202367902,16.8685283942095,1.65368679011474));
#28768=CARTESIAN_POINT('Ctrl Pts',(15.4999999999998,17.3247045256126,1.61202012344807));
#28769=CARTESIAN_POINT('Ctrl Pts',(14.7098797632094,16.8685283942095,1.57035345678141));
#28770=CARTESIAN_POINT('Ctrl Pts',(13.919759526419,16.4123522628064,1.52868679011474));
#28771=CARTESIAN_POINT('Ctrl Pts',(13.919759526419,15.5000000000001,1.48702012344807));
#28772=CARTESIAN_POINT('Ctrl Pts',(13.919759526419,14.5876477371939,1.4453534567814));
#28773=CARTESIAN_POINT('Ctrl Pts',(14.7098797632094,14.1314716057908,1.40368679011474));
#28774=CARTESIAN_POINT('Ctrl Pts',(15.4999999999999,13.6752954743877,1.36202012344807));
#28775=CARTESIAN_POINT('Ctrl Pts',(16.2901202367903,14.1314716057908,1.3203534567814));
#28776=CARTESIAN_POINT('Ctrl Pts',(17.0802404735807,14.5876477371939,1.27868679011473));
#28777=CARTESIAN_POINT('Ctrl Pts',(17.0802404735807,15.5000000000002,1.23702012344807));
#28778=CARTESIAN_POINT('Ctrl Pts',(17.0802404735807,16.4123522628064,1.1953534567814));
#28779=CARTESIAN_POINT('Ctrl Pts',(16.2901202367902,16.8685283942095,1.15368679011473));
#28780=CARTESIAN_POINT('Ctrl Pts',(15.4999999999998,17.3247045256126,1.11202012344807));
#28781=CARTESIAN_POINT('Ctrl Pts',(14.7098797632094,16.8685283942095,1.0703534567814));
#28782=CARTESIAN_POINT('Ctrl Pts',(13.919759526419,16.4123522628064,1.02868679011473));
#28783=CARTESIAN_POINT('Ctrl Pts',(13.919759526419,15.5000000000001,0.987020123448066));
#28784=CARTESIAN_POINT('Ctrl Pts',(13.919759526419,14.5876477371939,0.945353456781398));
#28785=CARTESIAN_POINT('Ctrl Pts',(14.7098797632094,14.1314716057908,0.903686790114731));
#28786=CARTESIAN_POINT('Ctrl Pts',(15.4999999999999,13.6752954743877,0.862020123448064));
#28787=CARTESIAN_POINT('Ctrl Pts',(16.2901202367903,14.1314716057908,0.820353456781396));
#28788=CARTESIAN_POINT('Ctrl Pts',(17.0802404735807,14.5876477371939,0.778686790114729));
#28789=CARTESIAN_POINT('Ctrl Pts',(17.0802404735807,15.5000000000002,0.737020123448062));
#28790=CARTESIAN_POINT('Ctrl Pts',(17.0802404735807,16.4123522628064,0.695353456781394));
#28791=CARTESIAN_POINT('Ctrl Pts',(16.2901202367902,16.8685283942095,0.653686790114727));
#28792=CARTESIAN_POINT('Ctrl Pts',(15.4999999999998,17.3247045256126,0.61202012344806));
#28793=CARTESIAN_POINT('Ctrl Pts',(14.7098797632094,16.8685283942095,0.570353456781393));
#28794=CARTESIAN_POINT('Ctrl Pts',(13.919759526419,16.4123522628064,0.528686790114725));
#28795=CARTESIAN_POINT('Ctrl Pts',(13.919759526419,15.5000000000001,0.487020123448058));
#28796=CARTESIAN_POINT('Ctrl Pts',(13.919759526419,14.5876477371939,0.445353456781391));
#28797=CARTESIAN_POINT('Ctrl Pts',(14.7098797632094,14.1314716057908,0.403686790114723));
#28798=CARTESIAN_POINT('Ctrl Pts',(15.4999999999999,13.6752954743877,0.362020123448056));
#28799=CARTESIAN_POINT('Ctrl Pts',(16.2901202367903,14.1314716057908,0.320353456781389));
#28800=CARTESIAN_POINT('Ctrl Pts',(17.0802404735807,14.5876477371939,0.278686790114722));
#28801=CARTESIAN_POINT('Ctrl Pts',(17.0802404735807,15.5000000000002,0.237020123448054));
#28802=CARTESIAN_POINT('Ctrl Pts',(17.0802404735807,16.4123522628064,0.195353456781387));
#28803=CARTESIAN_POINT('Ctrl Pts',(16.2901202367902,16.8685283942095,0.15368679011472));
#28804=CARTESIAN_POINT('Ctrl Pts',(15.4999999999998,17.3247045256126,0.112020123448053));
#28805=CARTESIAN_POINT('Ctrl Pts',(14.7098797632094,16.8685283942095,0.0703534567813852));
#28806=CARTESIAN_POINT('Ctrl Pts',(13.919759526419,16.4123522628064,0.0286867901147179));
#28807=CARTESIAN_POINT('Ctrl Pts',(13.919759526419,15.5000000000001,-0.0129798765519493));
#28808=CARTESIAN_POINT('Ctrl Pts',(13.919759526419,14.5876477371939,-0.0546465432186149));
#28809=CARTESIAN_POINT('Ctrl Pts',(14.7098797632094,14.1314716057908,-0.0963132098852822));
#28810=CARTESIAN_POINT('Ctrl Pts',(15.4999999999999,13.6752954743877,-0.137979876551949));
#28811=CARTESIAN_POINT('Ctrl Pts',(16.2901202367903,14.1314716057908,-0.179646543218617));
#28812=CARTESIAN_POINT('Ctrl Pts',(17.0802404735807,14.5876477371939,-0.221313209885284));
#28813=CARTESIAN_POINT('Ctrl Pts',(17.0802404735807,15.5000000000002,-0.262979876551951));
#28814=CARTESIAN_POINT('Ctrl Pts',(17.0802404735807,16.4123522628064,-0.304646543218619));
#28815=CARTESIAN_POINT('Ctrl Pts',(16.2901202367902,16.8685283942095,-0.346313209885286));
#28816=CARTESIAN_POINT('Ctrl Pts',(15.4999999999998,17.3247045256126,-0.387979876551953));
#28817=CARTESIAN_POINT('Ctrl Pts',(14.7098797632094,16.8685283942095,-0.429646543218621));
#28818=CARTESIAN_POINT('Ctrl Pts',(13.919759526419,16.4123522628064,-0.471313209885288));
#28819=CARTESIAN_POINT('Ctrl Pts',(13.919759526419,15.5000000000001,-0.512979876551955));
#28820=CARTESIAN_POINT('Ctrl Pts',(13.919759526419,14.5876477371939,-0.554646543218622));
#28821=CARTESIAN_POINT('Ctrl Pts',(14.7098797632094,14.1314716057908,-0.59631320988529));
#28822=CARTESIAN_POINT('Ctrl Pts',(15.4999999999999,13.6752954743877,-0.637979876551957));
#28823=CARTESIAN_POINT('Ctrl Pts',(16.2901202367903,14.1314716057908,-0.679646543218624));
#28824=CARTESIAN_POINT('Ctrl Pts',(17.0802404735807,14.5876477371939,-0.721313209885291));
#28825=CARTESIAN_POINT('Ctrl Pts',(17.0802404735807,15.5000000000002,-0.762979876551959));
#28826=CARTESIAN_POINT('Ctrl Pts',(17.0802404735807,16.4123522628064,-0.804646543218626));
#28827=CARTESIAN_POINT('Ctrl Pts',(16.2901202367902,16.8685283942095,-0.846313209885293));
#28828=CARTESIAN_POINT('Ctrl Pts',(15.4999999999998,17.3247045256126,-0.887979876551961));
#28829=CARTESIAN_POINT('Ctrl Pts',(14.7098797632094,16.8685283942095,-0.929646543218628));
#28830=CARTESIAN_POINT('Ctrl Pts',(13.919759526419,16.4123522628064,-0.971313209885295));
#28831=CARTESIAN_POINT('Ctrl Pts',(13.919759526419,15.5000000000001,-1.01297987655196));
#28832=CARTESIAN_POINT('Ctrl Pts',(13.919759526419,14.5876477371939,-1.05464654321863));
#28833=CARTESIAN_POINT('Ctrl Pts',(14.7098797632094,14.1314716057908,-1.0963132098853));
#28834=CARTESIAN_POINT('Ctrl Pts',(15.4999999999999,13.6752954743877,-1.13797987655196));
#28835=CARTESIAN_POINT('Ctrl Pts',(16.2901202367903,14.1314716057908,-1.17964654321863));
#28836=CARTESIAN_POINT('Ctrl Pts',(17.0802404735807,14.5876477371939,-1.2213132098853));
#28837=CARTESIAN_POINT('Ctrl Pts',(17.0802404735807,15.5000000000002,-1.26297987655196));
#28838=CARTESIAN_POINT('Ctrl Pts',(17.0802404735807,16.4123522628064,-1.30464654321863));
#28839=CARTESIAN_POINT('Ctrl Pts',(16.2901202367902,16.8685283942095,-1.3463132098853));
#28840=CARTESIAN_POINT('Ctrl Pts',(15.4999999999998,17.3247045256126,-1.38797987655197));
#28841=CARTESIAN_POINT('Ctrl Pts',(14.7098797632094,16.8685283942095,-1.42964654321863));
#28842=CARTESIAN_POINT('Ctrl Pts',(13.919759526419,16.4123522628064,-1.4713132098853));
#28843=CARTESIAN_POINT('Ctrl Pts',(13.919759526419,15.5000000000001,-1.51297987655197));
#28844=CARTESIAN_POINT('Ctrl Pts',(13.919759526419,14.5876477371939,-1.55464654321864));
#28845=CARTESIAN_POINT('Ctrl Pts',(14.7098797632094,14.1314716057908,-1.5963132098853));
#28846=CARTESIAN_POINT('Ctrl Pts',(15.4999999999999,13.6752954743877,-1.63797987655197));
#28847=CARTESIAN_POINT('Ctrl Pts',(16.2901202367903,14.1314716057908,-1.67964654321864));
#28848=CARTESIAN_POINT('Ctrl Pts',(17.0802404735807,14.5876477371939,-1.7213132098853));
#28849=CARTESIAN_POINT('Ctrl Pts',(17.0802404735807,15.5000000000002,-1.76297987655197));
#28850=CARTESIAN_POINT('Ctrl Pts',(17.0802404735807,16.4123522628064,-1.80464654321864));
#28851=CARTESIAN_POINT('Ctrl Pts',(16.2901202367902,16.8685283942095,-1.84631320988531));
#28852=CARTESIAN_POINT('Ctrl Pts',(15.4999999999998,17.3247045256126,-1.88797987655197));
#28853=CARTESIAN_POINT('Ctrl Pts',(14.7098797632094,16.8685283942095,-1.92964654321864));
#28854=CARTESIAN_POINT('Ctrl Pts',(14.4189900731897,16.7005831533721,-1.94498649173085));
#28855=CARTESIAN_POINT('Ctrl Pts',(14.2215586016754,16.4288420454489,-1.96260250461286));
#28856=CARTESIAN_POINT('Ctrl Pts',(13.4352476007233,15.3465777998747,-2.03276185973389));
#28857=CARTESIAN_POINT('Ctrl Pts',(12.6489365997711,14.2643135543005,-2.10292121485492));
#28858=CARTESIAN_POINT('Ctrl Pts',(17.0802404735807,15.5000000000002,11.1745));
#28859=CARTESIAN_POINT('Ctrl Pts',(17.0802404735807,16.4123522628064,11.1328333333333));
#28860=CARTESIAN_POINT('Ctrl Pts',(16.2901202367902,16.8685283942095,11.0911666666667));
#28861=CARTESIAN_POINT('Ctrl Pts',(15.4999999999998,17.3247045256126,11.0495));
#28862=CARTESIAN_POINT('Ctrl Pts',(14.7098797632094,16.8685283942095,11.0078333333333));
#28863=CARTESIAN_POINT('Ctrl Pts',(13.919759526419,16.4123522628064,10.9661666666667));
#28864=CARTESIAN_POINT('Ctrl Pts',(13.919759526419,15.5000000000001,10.9245));
#28865=CARTESIAN_POINT('Ctrl Pts',(13.919759526419,14.5876477371939,10.8828333333333));
#28866=CARTESIAN_POINT('Ctrl Pts',(14.7098797632094,14.1314716057908,10.8411666666667));
#28867=CARTESIAN_POINT('Ctrl Pts',(15.4999999999999,13.6752954743877,10.7995));
#28868=CARTESIAN_POINT('Ctrl Pts',(16.2901202367903,14.1314716057908,10.7578333333333));
#28869=CARTESIAN_POINT('Ctrl Pts',(17.0802404735807,14.5876477371939,10.7161666666667));
#28870=CARTESIAN_POINT('Ctrl Pts',(17.0802404735807,15.5000000000002,10.6745));
#28871=CARTESIAN_POINT('Ctrl Pts',(17.0802404735807,16.4123522628064,10.6328333333333));
#28872=CARTESIAN_POINT('Ctrl Pts',(16.2901202367902,16.8685283942095,10.5911666666667));
#28873=CARTESIAN_POINT('Ctrl Pts',(15.4999999999998,17.3247045256126,10.5495));
#28874=CARTESIAN_POINT('Ctrl Pts',(14.7098797632094,16.8685283942095,10.5078333333333));
#28875=CARTESIAN_POINT('Ctrl Pts',(13.919759526419,16.4123522628064,10.4661666666667));
#28876=CARTESIAN_POINT('Ctrl Pts',(13.919759526419,15.5000000000001,10.4245));
#28877=CARTESIAN_POINT('Ctrl Pts',(13.919759526419,14.5876477371939,10.3828333333333));
#28878=CARTESIAN_POINT('Ctrl Pts',(14.7098797632094,14.1314716057908,10.3411666666667));
#28879=CARTESIAN_POINT('Ctrl Pts',(15.4999999999999,13.6752954743877,10.2995));
#28880=CARTESIAN_POINT('Ctrl Pts',(16.2901202367903,14.1314716057908,10.2578333333333));
#28881=CARTESIAN_POINT('Ctrl Pts',(17.0802404735807,14.5876477371939,10.2161666666667));
#28882=CARTESIAN_POINT('Ctrl Pts',(17.0802404735807,15.5000000000002,10.1745));
#28883=CARTESIAN_POINT('Ctrl Pts',(17.0802404735807,16.4123522628064,10.1328333333333));
#28884=CARTESIAN_POINT('Ctrl Pts',(16.2901202367902,16.8685283942095,10.0911666666667));
#28885=CARTESIAN_POINT('Ctrl Pts',(15.4999999999998,17.3247045256126,10.0495));
#28886=CARTESIAN_POINT('Ctrl Pts',(14.7098797632094,16.8685283942095,10.0078333333333));
#28887=CARTESIAN_POINT('Ctrl Pts',(13.919759526419,16.4123522628064,9.96616666666665));
#28888=CARTESIAN_POINT('Ctrl Pts',(13.919759526419,15.5000000000001,9.92449999999998));
#28889=CARTESIAN_POINT('Ctrl Pts',(13.919759526419,14.5876477371939,9.88283333333331));
#28890=CARTESIAN_POINT('Ctrl Pts',(14.7098797632094,14.1314716057908,9.84116666666665));
#28891=CARTESIAN_POINT('Ctrl Pts',(15.4999999999999,13.6752954743877,9.79949999999998));
#28892=CARTESIAN_POINT('Ctrl Pts',(16.2901202367903,14.1314716057908,9.75783333333331));
#28893=CARTESIAN_POINT('Ctrl Pts',(17.0802404735807,14.5876477371939,9.71616666666665));
#28894=CARTESIAN_POINT('Ctrl Pts',(17.0802404735807,15.5000000000002,9.67449999999998));
#28895=CARTESIAN_POINT('Ctrl Pts',(17.0802404735807,16.4123522628064,9.63283333333331));
#28896=CARTESIAN_POINT('Ctrl Pts',(16.2901202367902,16.8685283942095,9.59116666666664));
#28897=CARTESIAN_POINT('Ctrl Pts',(15.4999999999998,17.3247045256126,9.54949999999998));
#28898=CARTESIAN_POINT('Ctrl Pts',(14.7098797632094,16.8685283942095,9.50783333333331));
#28899=CARTESIAN_POINT('Ctrl Pts',(13.919759526419,16.4123522628064,9.46616666666664));
#28900=CARTESIAN_POINT('Ctrl Pts',(13.919759526419,15.5000000000001,9.42449999999998));
#28901=CARTESIAN_POINT('Ctrl Pts',(13.919759526419,14.5876477371939,9.38283333333331));
#28902=CARTESIAN_POINT('Ctrl Pts',(14.7098797632094,14.1314716057908,9.34116666666664));
#28903=CARTESIAN_POINT('Ctrl Pts',(15.4999999999999,13.6752954743877,9.29949999999998));
#28904=CARTESIAN_POINT('Ctrl Pts',(16.2901202367903,14.1314716057908,9.25783333333331));
#28905=CARTESIAN_POINT('Ctrl Pts',(17.0802404735807,14.5876477371939,9.21616666666664));
#28906=CARTESIAN_POINT('Ctrl Pts',(17.0802404735807,15.5000000000002,9.17449999999997));
#28907=CARTESIAN_POINT('Ctrl Pts',(17.0802404735807,16.4123522628064,9.13283333333331));
#28908=CARTESIAN_POINT('Ctrl Pts',(16.2901202367902,16.8685283942095,9.09116666666664));
#28909=CARTESIAN_POINT('Ctrl Pts',(15.4999999999998,17.3247045256126,9.04949999999997));
#28910=CARTESIAN_POINT('Ctrl Pts',(14.7098797632094,16.8685283942095,9.0078333333333));
#28911=CARTESIAN_POINT('Ctrl Pts',(13.919759526419,16.4123522628064,8.96616666666664));
#28912=CARTESIAN_POINT('Ctrl Pts',(13.919759526419,15.5000000000001,8.92449999999997));
#28913=CARTESIAN_POINT('Ctrl Pts',(13.919759526419,14.5876477371939,8.8828333333333));
#28914=CARTESIAN_POINT('Ctrl Pts',(14.7098797632094,14.1314716057908,8.84116666666664));
#28915=CARTESIAN_POINT('Ctrl Pts',(15.4999999999999,13.6752954743877,8.79949999999997));
#28916=CARTESIAN_POINT('Ctrl Pts',(16.2901202367903,14.1314716057908,8.7578333333333));
#28917=CARTESIAN_POINT('Ctrl Pts',(17.0802404735807,14.5876477371939,8.71616666666663));
#28918=CARTESIAN_POINT('Ctrl Pts',(17.0802404735807,15.5000000000002,8.67449999999997));
#28919=CARTESIAN_POINT('Ctrl Pts',(17.0802404735807,16.4123522628064,8.6328333333333));
#28920=CARTESIAN_POINT('Ctrl Pts',(16.2901202367902,16.8685283942095,8.59116666666663));
#28921=CARTESIAN_POINT('Ctrl Pts',(15.4999999999998,17.3247045256126,8.54949999999996));
#28922=CARTESIAN_POINT('Ctrl Pts',(14.7098797632094,16.8685283942095,8.50783333333329));
#28923=CARTESIAN_POINT('Ctrl Pts',(13.919759526419,16.4123522628064,8.46616666666663));
#28924=CARTESIAN_POINT('Ctrl Pts',(13.919759526419,15.5000000000001,8.42449999999996));
#28925=CARTESIAN_POINT('Ctrl Pts',(13.919759526419,14.5876477371939,8.3828333333333));
#28926=CARTESIAN_POINT('Ctrl Pts',(14.7098797632094,14.1314716057908,8.34116666666663));
#28927=CARTESIAN_POINT('Ctrl Pts',(15.4999999999999,13.6752954743877,8.29949999999996));
#28928=CARTESIAN_POINT('Ctrl Pts',(16.2901202367903,14.1314716057908,8.25783333333329));
#28929=CARTESIAN_POINT('Ctrl Pts',(17.0802404735807,14.5876477371939,8.21616666666663));
#28930=CARTESIAN_POINT('Ctrl Pts',(17.0802404735807,15.5000000000002,8.17449999999996));
#28931=CARTESIAN_POINT('Ctrl Pts',(17.0802404735807,16.4123522628064,8.13283333333329));
#28932=CARTESIAN_POINT('Ctrl Pts',(16.2901202367902,16.8685283942095,8.09116666666663));
#28933=CARTESIAN_POINT('Ctrl Pts',(15.4999999999998,17.3247045256126,8.04949999999996));
#28934=CARTESIAN_POINT('Ctrl Pts',(14.7098797632094,16.8685283942095,8.00783333333329));
#28935=CARTESIAN_POINT('Ctrl Pts',(13.919759526419,16.4123522628064,7.96616666666662));
#28936=CARTESIAN_POINT('Ctrl Pts',(13.919759526419,15.5000000000001,7.92449999999996));
#28937=CARTESIAN_POINT('Ctrl Pts',(13.919759526419,14.5876477371939,7.88283333333329));
#28938=CARTESIAN_POINT('Ctrl Pts',(14.7098797632094,14.1314716057908,7.84116666666662));
#28939=CARTESIAN_POINT('Ctrl Pts',(15.4999999999999,13.6752954743877,7.79949999999995));
#28940=CARTESIAN_POINT('Ctrl Pts',(16.2901202367903,14.1314716057908,7.75783333333329));
#28941=CARTESIAN_POINT('Ctrl Pts',(17.0802404735807,14.5876477371939,7.71616666666662));
#28942=CARTESIAN_POINT('Ctrl Pts',(17.0802404735807,15.5000000000002,7.67449999999995));
#28943=CARTESIAN_POINT('Ctrl Pts',(17.0802404735807,16.4123522628064,7.63283333333328));
#28944=CARTESIAN_POINT('Ctrl Pts',(16.2901202367902,16.8685283942095,7.59116666666662));
#28945=CARTESIAN_POINT('Ctrl Pts',(15.4999999999998,17.3247045256126,7.54949999999995));
#28946=CARTESIAN_POINT('Ctrl Pts',(14.7098797632094,16.8685283942095,7.50783333333328));
#28947=CARTESIAN_POINT('Ctrl Pts',(13.919759526419,16.4123522628064,7.46616666666662));
#28948=CARTESIAN_POINT('Ctrl Pts',(13.919759526419,15.5000000000001,7.42449999999995));
#28949=CARTESIAN_POINT('Ctrl Pts',(13.919759526419,14.5876477371939,7.38283333333328));
#28950=CARTESIAN_POINT('Ctrl Pts',(14.7098797632094,14.1314716057908,7.34116666666661));
#28951=CARTESIAN_POINT('Ctrl Pts',(15.4999999999999,13.6752954743877,7.29949999999995));
#28952=CARTESIAN_POINT('Ctrl Pts',(16.2901202367903,14.1314716057908,7.25783333333328));
#28953=CARTESIAN_POINT('Ctrl Pts',(17.0802404735807,14.5876477371939,7.21616666666661));
#28954=CARTESIAN_POINT('Ctrl Pts',(17.0802404735807,15.5000000000002,7.17449999999995));
#28955=CARTESIAN_POINT('Ctrl Pts',(17.0802404735807,16.4123522628064,7.13283333333328));
#28956=CARTESIAN_POINT('Ctrl Pts',(16.2901202367902,16.8685283942095,7.09116666666661));
#28957=CARTESIAN_POINT('Ctrl Pts',(15.4999999999998,17.3247045256126,7.04949999999994));
#28958=CARTESIAN_POINT('Ctrl Pts',(14.7098797632094,16.8685283942095,7.00783333333328));
#28959=CARTESIAN_POINT('Ctrl Pts',(13.919759526419,16.4123522628064,6.96616666666661));
#28960=CARTESIAN_POINT('Ctrl Pts',(13.919759526419,15.5000000000001,6.92449999999994));
#28961=CARTESIAN_POINT('Ctrl Pts',(13.919759526419,14.5876477371939,6.88283333333327));
#28962=CARTESIAN_POINT('Ctrl Pts',(14.7098797632094,14.1314716057908,6.84116666666661));
#28963=CARTESIAN_POINT('Ctrl Pts',(15.4999999999999,13.6752954743877,6.79949999999994));
#28964=CARTESIAN_POINT('Ctrl Pts',(16.2901202367903,14.1314716057908,6.75783333333327));
#28965=CARTESIAN_POINT('Ctrl Pts',(17.0802404735807,14.5876477371939,6.71616666666661));
#28966=CARTESIAN_POINT('Ctrl Pts',(17.0802404735807,15.5000000000002,6.67449999999994));
#28967=CARTESIAN_POINT('Ctrl Pts',(17.0802404735807,16.4123522628064,6.63283333333327));
#28968=CARTESIAN_POINT('Ctrl Pts',(16.2901202367902,16.8685283942095,6.59116666666661));
#28969=CARTESIAN_POINT('Ctrl Pts',(15.4999999999998,17.3247045256126,6.54949999999994));
#28970=CARTESIAN_POINT('Ctrl Pts',(14.7098797632094,16.8685283942095,6.50783333333327));
#28971=CARTESIAN_POINT('Ctrl Pts',(13.919759526419,16.4123522628064,6.4661666666666));
#28972=CARTESIAN_POINT('Ctrl Pts',(13.919759526419,15.5000000000001,6.42449999999994));
#28973=CARTESIAN_POINT('Ctrl Pts',(13.919759526419,14.5876477371939,6.38283333333327));
#28974=CARTESIAN_POINT('Ctrl Pts',(14.7098797632094,14.1314716057908,6.3411666666666));
#28975=CARTESIAN_POINT('Ctrl Pts',(15.4999999999999,13.6752954743877,6.29949999999993));
#28976=CARTESIAN_POINT('Ctrl Pts',(16.2901202367903,14.1314716057908,6.25783333333327));
#28977=CARTESIAN_POINT('Ctrl Pts',(17.0802404735807,14.5876477371939,6.2161666666666));
#28978=CARTESIAN_POINT('Ctrl Pts',(17.0802404735807,15.5000000000002,6.17449999999993));
#28979=CARTESIAN_POINT('Ctrl Pts',(17.0802404735807,16.4123522628064,6.13283333333326));
#28980=CARTESIAN_POINT('Ctrl Pts',(16.2901202367902,16.8685283942095,6.0911666666666));
#28981=CARTESIAN_POINT('Ctrl Pts',(15.4999999999998,17.3247045256126,6.04949999999993));
#28982=CARTESIAN_POINT('Ctrl Pts',(14.7098797632094,16.8685283942095,6.00783333333326));
#28983=CARTESIAN_POINT('Ctrl Pts',(13.919759526419,16.4123522628064,5.9661666666666));
#28984=CARTESIAN_POINT('Ctrl Pts',(13.919759526419,15.5000000000001,5.92449999999993));
#28985=CARTESIAN_POINT('Ctrl Pts',(13.919759526419,14.5876477371939,5.88283333333326));
#28986=CARTESIAN_POINT('Ctrl Pts',(14.7098797632094,14.1314716057908,5.8411666666666));
#28987=CARTESIAN_POINT('Ctrl Pts',(15.4999999999999,13.6752954743877,5.79949999999993));
#28988=CARTESIAN_POINT('Ctrl Pts',(16.2901202367903,14.1314716057908,5.75783333333326));
#28989=CARTESIAN_POINT('Ctrl Pts',(17.0802404735807,14.5876477371939,5.71616666666659));
#28990=CARTESIAN_POINT('Ctrl Pts',(17.0802404735807,15.5000000000002,5.67449999999993));
#28991=CARTESIAN_POINT('Ctrl Pts',(17.0802404735807,16.4123522628064,5.63283333333326));
#28992=CARTESIAN_POINT('Ctrl Pts',(16.2901202367902,16.8685283942095,5.59116666666659));
#28993=CARTESIAN_POINT('Ctrl Pts',(15.4999999999998,17.3247045256126,5.54949999999992));
#28994=CARTESIAN_POINT('Ctrl Pts',(14.7098797632094,16.8685283942095,5.50783333333326));
#28995=CARTESIAN_POINT('Ctrl Pts',(13.919759526419,16.4123522628064,5.46616666666659));
#28996=CARTESIAN_POINT('Ctrl Pts',(13.919759526419,15.5000000000001,5.42449999999992));
#28997=CARTESIAN_POINT('Ctrl Pts',(13.919759526419,14.5876477371939,5.38283333333326));
#28998=CARTESIAN_POINT('Ctrl Pts',(14.7098797632094,14.1314716057908,5.34116666666659));
#28999=CARTESIAN_POINT('Ctrl Pts',(15.4999999999999,13.6752954743877,5.29949999999992));
#29000=CARTESIAN_POINT('Ctrl Pts',(16.2901202367903,14.1314716057908,5.25783333333325));
#29001=CARTESIAN_POINT('Ctrl Pts',(17.0802404735807,14.5876477371939,5.21616666666659));
#29002=CARTESIAN_POINT('Ctrl Pts',(17.0802404735807,15.5000000000002,5.17449999999992));
#29003=CARTESIAN_POINT('Ctrl Pts',(17.0802404735807,16.4123522628064,5.13283333333325));
#29004=CARTESIAN_POINT('Ctrl Pts',(16.2901202367902,16.8685283942095,5.09116666666658));
#29005=CARTESIAN_POINT('Ctrl Pts',(15.4999999999998,17.3247045256126,5.04949999999992));
#29006=CARTESIAN_POINT('Ctrl Pts',(14.7098797632094,16.8685283942095,5.00783333333325));
#29007=CARTESIAN_POINT('Ctrl Pts',(13.919759526419,16.4123522628064,4.96616666666658));
#29008=CARTESIAN_POINT('Ctrl Pts',(13.919759526419,15.5000000000001,4.92449999999992));
#29009=CARTESIAN_POINT('Ctrl Pts',(13.919759526419,14.5876477371939,4.88283333333325));
#29010=CARTESIAN_POINT('Ctrl Pts',(14.7098797632094,14.1314716057908,4.84116666666658));
#29011=CARTESIAN_POINT('Ctrl Pts',(15.4999999999999,13.6752954743877,4.79949999999991));
#29012=CARTESIAN_POINT('Ctrl Pts',(16.2901202367903,14.1314716057908,4.75783333333325));
#29013=CARTESIAN_POINT('Ctrl Pts',(17.0802404735807,14.5876477371939,4.71616666666658));
#29014=CARTESIAN_POINT('Ctrl Pts',(17.0802404735807,15.5000000000002,4.67449999999991));
#29015=CARTESIAN_POINT('Ctrl Pts',(17.0802404735807,16.4123522628064,4.63283333333324));
#29016=CARTESIAN_POINT('Ctrl Pts',(16.2901202367902,16.8685283942095,4.59116666666658));
#29017=CARTESIAN_POINT('Ctrl Pts',(15.4999999999998,17.3247045256126,4.54949999999991));
#29018=CARTESIAN_POINT('Ctrl Pts',(14.7098797632094,16.8685283942095,4.50783333333324));
#29019=CARTESIAN_POINT('Ctrl Pts',(13.919759526419,16.4123522628064,4.46616666666658));
#29020=CARTESIAN_POINT('Ctrl Pts',(13.919759526419,15.5000000000001,4.42449999999991));
#29021=CARTESIAN_POINT('Ctrl Pts',(13.919759526419,14.5876477371939,4.38283333333324));
#29022=CARTESIAN_POINT('Ctrl Pts',(14.7098797632094,14.1314716057908,4.34116666666657));
#29023=CARTESIAN_POINT('Ctrl Pts',(15.4999999999999,13.6752954743877,4.29949999999991));
#29024=CARTESIAN_POINT('Ctrl Pts',(16.2901202367903,14.1314716057908,4.25783333333324));
#29025=CARTESIAN_POINT('Ctrl Pts',(17.0802404735807,14.5876477371939,4.21616666666657));
#29026=CARTESIAN_POINT('Ctrl Pts',(17.0802404735807,15.5000000000002,4.17449999999991));
#29027=CARTESIAN_POINT('Ctrl Pts',(17.0802404735807,16.4123522628064,4.13283333333324));
#29028=CARTESIAN_POINT('Ctrl Pts',(16.2901202367902,16.8685283942095,4.09116666666657));
#29029=CARTESIAN_POINT('Ctrl Pts',(15.4999999999998,17.3247045256126,4.0494999999999));
#29030=CARTESIAN_POINT('Ctrl Pts',(14.7098797632094,16.8685283942095,4.00783333333324));
#29031=CARTESIAN_POINT('Ctrl Pts',(13.919759526419,16.4123522628064,3.96616666666657));
#29032=CARTESIAN_POINT('Ctrl Pts',(13.919759526419,15.5000000000001,3.9244999999999));
#29033=CARTESIAN_POINT('Ctrl Pts',(13.919759526419,14.5876477371939,3.88283333333323));
#29034=CARTESIAN_POINT('Ctrl Pts',(14.7098797632094,14.1314716057908,3.84116666666657));
#29035=CARTESIAN_POINT('Ctrl Pts',(15.4999999999999,13.6752954743877,3.7994999999999));
#29036=CARTESIAN_POINT('Ctrl Pts',(16.2901202367903,14.1314716057908,3.75783333333323));
#29037=CARTESIAN_POINT('Ctrl Pts',(17.0802404735807,14.5876477371939,3.71616666666657));
#29038=CARTESIAN_POINT('Ctrl Pts',(17.0802404735807,15.5000000000002,3.6744999999999));
#29039=CARTESIAN_POINT('Ctrl Pts',(17.0802404735807,16.4123522628064,3.63283333333323));
#29040=CARTESIAN_POINT('Ctrl Pts',(16.2901202367902,16.8685283942095,3.59116666666656));
#29041=CARTESIAN_POINT('Ctrl Pts',(15.4999999999998,17.3247045256126,3.5494999999999));
#29042=CARTESIAN_POINT('Ctrl Pts',(14.7098797632094,16.8685283942095,3.50783333333323));
#29043=CARTESIAN_POINT('Ctrl Pts',(13.919759526419,16.4123522628064,3.46616666666656));
#29044=CARTESIAN_POINT('Ctrl Pts',(13.919759526419,15.5000000000001,3.4244999999999));
#29045=CARTESIAN_POINT('Ctrl Pts',(13.919759526419,14.5876477371939,3.38283333333323));
#29046=CARTESIAN_POINT('Ctrl Pts',(14.7098797632094,14.1314716057908,3.34116666666656));
#29047=CARTESIAN_POINT('Ctrl Pts',(15.4999999999999,13.6752954743877,3.29949999999989));
#29048=CARTESIAN_POINT('Ctrl Pts',(16.2901202367903,14.1314716057908,3.25783333333323));
#29049=CARTESIAN_POINT('Ctrl Pts',(17.0802404735807,14.5876477371939,3.21616666666656));
#29050=CARTESIAN_POINT('Ctrl Pts',(17.0802404735807,15.5000000000002,3.17449999999989));
#29051=CARTESIAN_POINT('Ctrl Pts',(17.0802404735807,16.4123522628064,3.13283333333323));
#29052=CARTESIAN_POINT('Ctrl Pts',(16.2901202367902,16.8685283942095,3.09116666666656));
#29053=CARTESIAN_POINT('Ctrl Pts',(15.4999999999998,17.3247045256126,3.04949999999989));
#29054=CARTESIAN_POINT('Ctrl Pts',(14.7098797632094,16.8685283942095,3.00783333333322));
#29055=CARTESIAN_POINT('Ctrl Pts',(13.919759526419,16.4123522628064,2.96616666666656));
#29056=CARTESIAN_POINT('Ctrl Pts',(13.919759526419,15.5000000000001,2.92449999999989));
#29057=CARTESIAN_POINT('Ctrl Pts',(13.919759526419,14.5876477371939,2.88283333333322));
#29058=CARTESIAN_POINT('Ctrl Pts',(14.7098797632094,14.1314716057908,2.84116666666655));
#29059=CARTESIAN_POINT('Ctrl Pts',(15.4999999999999,13.6752954743877,2.79949999999989));
#29060=CARTESIAN_POINT('Ctrl Pts',(16.2901202367903,14.1314716057908,2.75783333333322));
#29061=CARTESIAN_POINT('Ctrl Pts',(17.0802404735807,14.5876477371939,2.71616666666655));
#29062=CARTESIAN_POINT('Ctrl Pts',(17.0802404735807,15.5000000000002,2.67449999999989));
#29063=CARTESIAN_POINT('Ctrl Pts',(17.0802404735807,16.4123522628064,2.63283333333322));
#29064=CARTESIAN_POINT('Ctrl Pts',(16.2901202367902,16.8685283942095,2.59116666666655));
#29065=CARTESIAN_POINT('Ctrl Pts',(15.4999999999998,17.3247045256126,2.54949999999988));
#29066=CARTESIAN_POINT('Ctrl Pts',(14.7098797632094,16.8685283942095,2.50783333333322));
#29067=CARTESIAN_POINT('Ctrl Pts',(13.919759526419,16.4123522628064,2.46616666666655));
#29068=CARTESIAN_POINT('Ctrl Pts',(13.919759526419,15.5000000000001,2.42449999999988));
#29069=CARTESIAN_POINT('Ctrl Pts',(13.919759526419,14.5876477371939,2.38283333333321));
#29070=CARTESIAN_POINT('Ctrl Pts',(14.7098797632094,14.1314716057908,2.34116666666655));
#29071=CARTESIAN_POINT('Ctrl Pts',(15.4999999999999,13.6752954743877,2.29949999999988));
#29072=CARTESIAN_POINT('Ctrl Pts',(16.2901202367903,14.1314716057908,2.25783333333321));
#29073=CARTESIAN_POINT('Ctrl Pts',(17.0802404735807,14.5876477371939,2.21616666666655));
#29074=CARTESIAN_POINT('Ctrl Pts',(17.0802404735807,15.5000000000002,2.17449999999988));
#29075=CARTESIAN_POINT('Ctrl Pts',(17.0802404735807,16.4123522628064,2.13283333333321));
#29076=CARTESIAN_POINT('Ctrl Pts',(16.2901202367902,16.8685283942095,2.09116666666655));
#29077=CARTESIAN_POINT('Ctrl Pts',(15.4999999999998,17.3247045256126,2.04949999999988));
#29078=CARTESIAN_POINT('Ctrl Pts',(14.7098797632094,16.8685283942095,2.00783333333321));
#29079=CARTESIAN_POINT('Ctrl Pts',(13.919759526419,16.4123522628064,1.96616666666654));
#29080=CARTESIAN_POINT('Ctrl Pts',(13.919759526419,15.5000000000001,1.92449999999988));
#29081=CARTESIAN_POINT('Ctrl Pts',(13.919759526419,14.5876477371939,1.88283333333321));
#29082=CARTESIAN_POINT('Ctrl Pts',(14.7098797632094,14.1314716057908,1.84116666666654));
#29083=CARTESIAN_POINT('Ctrl Pts',(15.4999999999999,13.6752954743877,1.79949999999987));
#29084=CARTESIAN_POINT('Ctrl Pts',(16.2901202367903,14.1314716057908,1.75783333333321));
#29085=CARTESIAN_POINT('Ctrl Pts',(17.0802404735807,14.5876477371939,1.71616666666654));
#29086=CARTESIAN_POINT('Ctrl Pts',(17.0802404735807,15.5000000000002,1.67449999999987));
#29087=CARTESIAN_POINT('Ctrl Pts',(17.0802404735807,16.4123522628064,1.63283333333321));
#29088=CARTESIAN_POINT('Ctrl Pts',(16.2901202367902,16.8685283942095,1.59116666666654));
#29089=CARTESIAN_POINT('Ctrl Pts',(15.4999999999998,17.3247045256126,1.54949999999987));
#29090=CARTESIAN_POINT('Ctrl Pts',(14.7098797632094,16.8685283942095,1.5078333333332));
#29091=CARTESIAN_POINT('Ctrl Pts',(13.919759526419,16.4123522628064,1.46616666666654));
#29092=CARTESIAN_POINT('Ctrl Pts',(13.919759526419,15.5000000000001,1.42449999999987));
#29093=CARTESIAN_POINT('Ctrl Pts',(13.919759526419,14.5876477371939,1.3828333333332));
#29094=CARTESIAN_POINT('Ctrl Pts',(14.7098797632094,14.1314716057908,1.34116666666653));
#29095=CARTESIAN_POINT('Ctrl Pts',(15.4999999999999,13.6752954743877,1.29949999999987));
#29096=CARTESIAN_POINT('Ctrl Pts',(16.2901202367903,14.1314716057908,1.2578333333332));
#29097=CARTESIAN_POINT('Ctrl Pts',(17.0802404735807,14.5876477371939,1.21616666666653));
#29098=CARTESIAN_POINT('Ctrl Pts',(17.0802404735807,15.5000000000002,1.17449999999986));
#29099=CARTESIAN_POINT('Ctrl Pts',(17.0802404735807,16.4123522628064,1.1328333333332));
#29100=CARTESIAN_POINT('Ctrl Pts',(16.2901202367902,16.8685283942095,1.09116666666653));
#29101=CARTESIAN_POINT('Ctrl Pts',(15.4999999999998,17.3247045256126,1.04949999999986));
#29102=CARTESIAN_POINT('Ctrl Pts',(14.7098797632094,16.8685283942095,1.0078333333332));
#29103=CARTESIAN_POINT('Ctrl Pts',(13.919759526419,16.4123522628064,0.96616666666653));
#29104=CARTESIAN_POINT('Ctrl Pts',(13.919759526419,15.5000000000001,0.924499999999863));
#29105=CARTESIAN_POINT('Ctrl Pts',(13.919759526419,14.5876477371939,0.882833333333196));
#29106=CARTESIAN_POINT('Ctrl Pts',(14.7098797632094,14.1314716057908,0.841166666666529));
#29107=CARTESIAN_POINT('Ctrl Pts',(15.4999999999999,13.6752954743877,0.799499999999861));
#29108=CARTESIAN_POINT('Ctrl Pts',(16.2901202367903,14.1314716057908,0.757833333333194));
#29109=CARTESIAN_POINT('Ctrl Pts',(17.0802404735807,14.5876477371939,0.716166666666527));
#29110=CARTESIAN_POINT('Ctrl Pts',(17.0802404735807,15.5000000000002,0.674499999999859));
#29111=CARTESIAN_POINT('Ctrl Pts',(17.0802404735807,16.4123522628064,0.632833333333192));
#29112=CARTESIAN_POINT('Ctrl Pts',(16.2901202367902,16.8685283942095,0.591166666666525));
#29113=CARTESIAN_POINT('Ctrl Pts',(15.4999999999998,17.3247045256126,0.549499999999857));
#29114=CARTESIAN_POINT('Ctrl Pts',(14.7098797632094,16.8685283942095,0.50783333333319));
#29115=CARTESIAN_POINT('Ctrl Pts',(13.919759526419,16.4123522628064,0.466166666666523));
#29116=CARTESIAN_POINT('Ctrl Pts',(13.919759526419,15.5000000000001,0.424499999999856));
#29117=CARTESIAN_POINT('Ctrl Pts',(13.919759526419,14.5876477371939,0.382833333333188));
#29118=CARTESIAN_POINT('Ctrl Pts',(14.7098797632094,14.1314716057908,0.341166666666521));
#29119=CARTESIAN_POINT('Ctrl Pts',(15.4999999999999,13.6752954743877,0.299499999999854));
#29120=CARTESIAN_POINT('Ctrl Pts',(16.2901202367903,14.1314716057908,0.257833333333186));
#29121=CARTESIAN_POINT('Ctrl Pts',(17.0802404735807,14.5876477371939,0.216166666666519));
#29122=CARTESIAN_POINT('Ctrl Pts',(17.0802404735807,15.5000000000002,0.174499999999852));
#29123=CARTESIAN_POINT('Ctrl Pts',(17.0802404735807,16.4123522628064,0.132833333333185));
#29124=CARTESIAN_POINT('Ctrl Pts',(16.2901202367902,16.8685283942095,0.0911666666665173));
#29125=CARTESIAN_POINT('Ctrl Pts',(15.4999999999998,17.3247045256126,0.04949999999985));
#29126=CARTESIAN_POINT('Ctrl Pts',(14.7098797632094,16.8685283942095,0.00783333333318273));
#29127=CARTESIAN_POINT('Ctrl Pts',(13.919759526419,16.4123522628064,-0.0338333333334846));
#29128=CARTESIAN_POINT('Ctrl Pts',(13.919759526419,15.5000000000001,-0.0755000000001518));
#29129=CARTESIAN_POINT('Ctrl Pts',(13.919759526419,14.5876477371939,-0.117166666666817));
#29130=CARTESIAN_POINT('Ctrl Pts',(14.7098797632094,14.1314716057908,-0.158833333333485));
#29131=CARTESIAN_POINT('Ctrl Pts',(15.4999999999999,13.6752954743877,-0.200500000000152));
#29132=CARTESIAN_POINT('Ctrl Pts',(16.2901202367903,14.1314716057908,-0.242166666666819));
#29133=CARTESIAN_POINT('Ctrl Pts',(17.0802404735807,14.5876477371939,-0.283833333333486));
#29134=CARTESIAN_POINT('Ctrl Pts',(17.0802404735807,15.5000000000002,-0.325500000000154));
#29135=CARTESIAN_POINT('Ctrl Pts',(17.0802404735807,16.4123522628064,-0.367166666666821));
#29136=CARTESIAN_POINT('Ctrl Pts',(16.2901202367902,16.8685283942095,-0.408833333333488));
#29137=CARTESIAN_POINT('Ctrl Pts',(15.4999999999998,17.3247045256126,-0.450500000000156));
#29138=CARTESIAN_POINT('Ctrl Pts',(14.7098797632094,16.8685283942095,-0.492166666666823));
#29139=CARTESIAN_POINT('Ctrl Pts',(13.919759526419,16.4123522628064,-0.53383333333349));
#29140=CARTESIAN_POINT('Ctrl Pts',(13.919759526419,15.5000000000001,-0.575500000000157));
#29141=CARTESIAN_POINT('Ctrl Pts',(13.919759526419,14.5876477371939,-0.617166666666825));
#29142=CARTESIAN_POINT('Ctrl Pts',(14.7098797632094,14.1314716057908,-0.658833333333492));
#29143=CARTESIAN_POINT('Ctrl Pts',(15.4999999999999,13.6752954743877,-0.700500000000159));
#29144=CARTESIAN_POINT('Ctrl Pts',(16.2901202367903,14.1314716057908,-0.742166666666827));
#29145=CARTESIAN_POINT('Ctrl Pts',(17.0802404735807,14.5876477371939,-0.783833333333494));
#29146=CARTESIAN_POINT('Ctrl Pts',(17.0802404735807,15.5000000000002,-0.825500000000161));
#29147=CARTESIAN_POINT('Ctrl Pts',(17.0802404735807,16.4123522628064,-0.867166666666829));
#29148=CARTESIAN_POINT('Ctrl Pts',(16.2901202367902,16.8685283942095,-0.908833333333496));
#29149=CARTESIAN_POINT('Ctrl Pts',(15.4999999999998,17.3247045256126,-0.950500000000163));
#29150=CARTESIAN_POINT('Ctrl Pts',(14.7098797632094,16.8685283942095,-0.99216666666683));
#29151=CARTESIAN_POINT('Ctrl Pts',(13.919759526419,16.4123522628064,-1.0338333333335));
#29152=CARTESIAN_POINT('Ctrl Pts',(13.919759526419,15.5000000000001,-1.07550000000016));
#29153=CARTESIAN_POINT('Ctrl Pts',(13.919759526419,14.5876477371939,-1.11716666666683));
#29154=CARTESIAN_POINT('Ctrl Pts',(14.7098797632094,14.1314716057908,-1.1588333333335));
#29155=CARTESIAN_POINT('Ctrl Pts',(15.4999999999999,13.6752954743877,-1.20050000000017));
#29156=CARTESIAN_POINT('Ctrl Pts',(16.2901202367903,14.1314716057908,-1.24216666666683));
#29157=CARTESIAN_POINT('Ctrl Pts',(17.0802404735807,14.5876477371939,-1.2838333333335));
#29158=CARTESIAN_POINT('Ctrl Pts',(17.0802404735807,15.5000000000002,-1.32550000000017));
#29159=CARTESIAN_POINT('Ctrl Pts',(17.0802404735807,16.4123522628064,-1.36716666666683));
#29160=CARTESIAN_POINT('Ctrl Pts',(16.2901202367902,16.8685283942095,-1.4088333333335));
#29161=CARTESIAN_POINT('Ctrl Pts',(15.4999999999998,17.3247045256126,-1.45050000000017));
#29162=CARTESIAN_POINT('Ctrl Pts',(14.7098797632094,16.8685283942095,-1.49216666666684));
#29163=CARTESIAN_POINT('Ctrl Pts',(13.919759526419,16.4123522628064,-1.5338333333335));
#29164=CARTESIAN_POINT('Ctrl Pts',(13.919759526419,15.5000000000001,-1.57550000000017));
#29165=CARTESIAN_POINT('Ctrl Pts',(13.919759526419,14.5876477371939,-1.61716666666684));
#29166=CARTESIAN_POINT('Ctrl Pts',(14.7098797632094,14.1314716057908,-1.65883333333351));
#29167=CARTESIAN_POINT('Ctrl Pts',(15.4999999999999,13.6752954743877,-1.70050000000017));
#29168=CARTESIAN_POINT('Ctrl Pts',(16.2901202367903,14.1314716057908,-1.74216666666684));
#29169=CARTESIAN_POINT('Ctrl Pts',(17.0802404735807,14.5876477371939,-1.78383333333351));
#29170=CARTESIAN_POINT('Ctrl Pts',(17.0802404735807,15.5000000000002,-1.82550000000017));
#29171=CARTESIAN_POINT('Ctrl Pts',(17.0802404735807,16.4123522628064,-1.86716666666684));
#29172=CARTESIAN_POINT('Ctrl Pts',(16.2901202367902,16.8685283942095,-1.90883333333351));
#29173=CARTESIAN_POINT('Ctrl Pts',(15.4999999999998,17.3247045256126,-1.95050000000018));
#29174=CARTESIAN_POINT('Ctrl Pts',(14.7098797632094,16.8685283942095,-1.99216666666684));
#29175=CARTESIAN_POINT('Ctrl Pts',(14.4189900731897,16.7005831533721,-2.00750661517905));
#29176=CARTESIAN_POINT('Ctrl Pts',(14.2215586016754,16.4288420454489,-2.02512262806106));
#29177=CARTESIAN_POINT('Ctrl Pts',(13.4352476007233,15.3465777998747,-2.09528198318209));
#29178=CARTESIAN_POINT('Ctrl Pts',(12.6489365997711,14.2643135543005,-2.16544133830312));
#29179=CARTESIAN_POINT('Ctrl Pts',(15.5,-17.0802317716412,11.1745050240672));
#29180=CARTESIAN_POINT('Ctrl Pts',(16.4123472387391,-17.0802317716412,11.1328383574005));
#29181=CARTESIAN_POINT('Ctrl Pts',(16.8685208581086,-16.2901158858206,11.0911716907338));
#29182=CARTESIAN_POINT('Ctrl Pts',(17.3246944774781,-15.5,11.0495050240672));
#29183=CARTESIAN_POINT('Ctrl Pts',(16.8685208581086,-14.7098841141794,11.0078383574005));
#29184=CARTESIAN_POINT('Ctrl Pts',(16.4123472387391,-13.9197682283588,10.9661716907338));
#29185=CARTESIAN_POINT('Ctrl Pts',(15.5,-13.9197682283588,10.9245050240672));
#29186=CARTESIAN_POINT('Ctrl Pts',(14.5876527612609,-13.9197682283588,10.8828383574005));
#29187=CARTESIAN_POINT('Ctrl Pts',(14.1314791418914,-14.7098841141794,10.8411716907338));
#29188=CARTESIAN_POINT('Ctrl Pts',(13.6753055225219,-15.5,10.7995050240672));
#29189=CARTESIAN_POINT('Ctrl Pts',(14.1314791418914,-16.2901158858206,10.7578383574005));
#29190=CARTESIAN_POINT('Ctrl Pts',(14.5876527612609,-17.0802317716412,10.7161716907338));
#29191=CARTESIAN_POINT('Ctrl Pts',(15.5,-17.0802317716412,10.6745050240672));
#29192=CARTESIAN_POINT('Ctrl Pts',(16.4123472387391,-17.0802317716412,10.6328383574005));
#29193=CARTESIAN_POINT('Ctrl Pts',(16.8685208581086,-16.2901158858206,10.5911716907338));
#29194=CARTESIAN_POINT('Ctrl Pts',(17.3246944774781,-15.5,10.5495050240672));
#29195=CARTESIAN_POINT('Ctrl Pts',(16.8685208581086,-14.7098841141794,10.5078383574005));
#29196=CARTESIAN_POINT('Ctrl Pts',(16.4123472387391,-13.9197682283588,10.4661716907338));
#29197=CARTESIAN_POINT('Ctrl Pts',(15.5,-13.9197682283588,10.4245050240672));
#29198=CARTESIAN_POINT('Ctrl Pts',(14.5876527612609,-13.9197682283588,10.3828383574005));
#29199=CARTESIAN_POINT('Ctrl Pts',(14.1314791418914,-14.7098841141794,10.3411716907338));
#29200=CARTESIAN_POINT('Ctrl Pts',(13.6753055225219,-15.5,10.2995050240672));
#29201=CARTESIAN_POINT('Ctrl Pts',(14.1314791418914,-16.2901158858206,10.2578383574005));
#29202=CARTESIAN_POINT('Ctrl Pts',(14.5876527612609,-17.0802317716412,10.2161716907338));
#29203=CARTESIAN_POINT('Ctrl Pts',(15.5,-17.0802317716412,10.1745050240672));
#29204=CARTESIAN_POINT('Ctrl Pts',(16.4123472387391,-17.0802317716412,10.1328383574005));
#29205=CARTESIAN_POINT('Ctrl Pts',(16.8685208581086,-16.2901158858206,10.0911716907338));
#29206=CARTESIAN_POINT('Ctrl Pts',(17.3246944774781,-15.5,10.0495050240672));
#29207=CARTESIAN_POINT('Ctrl Pts',(16.8685208581086,-14.7098841141794,10.0078383574005));
#29208=CARTESIAN_POINT('Ctrl Pts',(16.4123472387391,-13.9197682283588,9.96617169073382));
#29209=CARTESIAN_POINT('Ctrl Pts',(15.5,-13.9197682283588,9.92450502406715));
#29210=CARTESIAN_POINT('Ctrl Pts',(14.5876527612609,-13.9197682283588,9.88283835740048));
#29211=CARTESIAN_POINT('Ctrl Pts',(14.1314791418914,-14.7098841141794,9.84117169073382));
#29212=CARTESIAN_POINT('Ctrl Pts',(13.6753055225219,-15.5,9.79950502406715));
#29213=CARTESIAN_POINT('Ctrl Pts',(14.1314791418914,-16.2901158858206,9.75783835740048));
#29214=CARTESIAN_POINT('Ctrl Pts',(14.5876527612609,-17.0802317716412,9.71617169073381));
#29215=CARTESIAN_POINT('Ctrl Pts',(15.5,-17.0802317716412,9.67450502406715));
#29216=CARTESIAN_POINT('Ctrl Pts',(16.4123472387391,-17.0802317716412,9.63283835740048));
#29217=CARTESIAN_POINT('Ctrl Pts',(16.8685208581086,-16.2901158858206,9.59117169073381));
#29218=CARTESIAN_POINT('Ctrl Pts',(17.3246944774781,-15.5,9.54950502406714));
#29219=CARTESIAN_POINT('Ctrl Pts',(16.8685208581086,-14.7098841141794,9.50783835740048));
#29220=CARTESIAN_POINT('Ctrl Pts',(16.4123472387391,-13.9197682283588,9.46617169073381));
#29221=CARTESIAN_POINT('Ctrl Pts',(15.5,-13.9197682283588,9.42450502406714));
#29222=CARTESIAN_POINT('Ctrl Pts',(14.5876527612609,-13.9197682283588,9.38283835740048));
#29223=CARTESIAN_POINT('Ctrl Pts',(14.1314791418914,-14.7098841141794,9.34117169073381));
#29224=CARTESIAN_POINT('Ctrl Pts',(13.6753055225219,-15.5,9.29950502406714));
#29225=CARTESIAN_POINT('Ctrl Pts',(14.1314791418914,-16.2901158858206,9.25783835740048));
#29226=CARTESIAN_POINT('Ctrl Pts',(14.5876527612609,-17.0802317716412,9.21617169073381));
#29227=CARTESIAN_POINT('Ctrl Pts',(15.5,-17.0802317716412,9.17450502406714));
#29228=CARTESIAN_POINT('Ctrl Pts',(16.4123472387391,-17.0802317716412,9.13283835740047));
#29229=CARTESIAN_POINT('Ctrl Pts',(16.8685208581086,-16.2901158858206,9.09117169073381));
#29230=CARTESIAN_POINT('Ctrl Pts',(17.3246944774781,-15.5,9.04950502406714));
#29231=CARTESIAN_POINT('Ctrl Pts',(16.8685208581086,-14.7098841141794,9.00783835740047));
#29232=CARTESIAN_POINT('Ctrl Pts',(16.4123472387391,-13.9197682283588,8.9661716907338));
#29233=CARTESIAN_POINT('Ctrl Pts',(15.5,-13.9197682283588,8.92450502406714));
#29234=CARTESIAN_POINT('Ctrl Pts',(14.5876527612609,-13.9197682283588,8.88283835740047));
#29235=CARTESIAN_POINT('Ctrl Pts',(14.1314791418914,-14.7098841141794,8.8411716907338));
#29236=CARTESIAN_POINT('Ctrl Pts',(13.6753055225219,-15.5,8.79950502406713));
#29237=CARTESIAN_POINT('Ctrl Pts',(14.1314791418914,-16.2901158858206,8.75783835740047));
#29238=CARTESIAN_POINT('Ctrl Pts',(14.5876527612609,-17.0802317716412,8.7161716907338));
#29239=CARTESIAN_POINT('Ctrl Pts',(15.5,-17.0802317716412,8.67450502406713));
#29240=CARTESIAN_POINT('Ctrl Pts',(16.4123472387391,-17.0802317716412,8.63283835740047));
#29241=CARTESIAN_POINT('Ctrl Pts',(16.8685208581086,-16.2901158858206,8.5911716907338));
#29242=CARTESIAN_POINT('Ctrl Pts',(17.3246944774781,-15.5,8.54950502406713));
#29243=CARTESIAN_POINT('Ctrl Pts',(16.8685208581086,-14.7098841141794,8.50783835740046));
#29244=CARTESIAN_POINT('Ctrl Pts',(16.4123472387391,-13.9197682283588,8.4661716907338));
#29245=CARTESIAN_POINT('Ctrl Pts',(15.5,-13.9197682283588,8.42450502406713));
#29246=CARTESIAN_POINT('Ctrl Pts',(14.5876527612609,-13.9197682283588,8.38283835740046));
#29247=CARTESIAN_POINT('Ctrl Pts',(14.1314791418914,-14.7098841141794,8.3411716907338));
#29248=CARTESIAN_POINT('Ctrl Pts',(13.6753055225219,-15.5,8.29950502406713));
#29249=CARTESIAN_POINT('Ctrl Pts',(14.1314791418914,-16.2901158858206,8.25783835740046));
#29250=CARTESIAN_POINT('Ctrl Pts',(14.5876527612609,-17.0802317716412,8.21617169073379));
#29251=CARTESIAN_POINT('Ctrl Pts',(15.5,-17.0802317716412,8.17450502406713));
#29252=CARTESIAN_POINT('Ctrl Pts',(16.4123472387391,-17.0802317716412,8.13283835740046));
#29253=CARTESIAN_POINT('Ctrl Pts',(16.8685208581086,-16.2901158858206,8.09117169073379));
#29254=CARTESIAN_POINT('Ctrl Pts',(17.3246944774781,-15.5,8.04950502406713));
#29255=CARTESIAN_POINT('Ctrl Pts',(16.8685208581086,-14.7098841141794,8.00783835740046));
#29256=CARTESIAN_POINT('Ctrl Pts',(16.4123472387391,-13.9197682283588,7.96617169073379));
#29257=CARTESIAN_POINT('Ctrl Pts',(15.5,-13.9197682283588,7.92450502406712));
#29258=CARTESIAN_POINT('Ctrl Pts',(14.5876527612609,-13.9197682283588,7.88283835740046));
#29259=CARTESIAN_POINT('Ctrl Pts',(14.1314791418914,-14.7098841141794,7.84117169073379));
#29260=CARTESIAN_POINT('Ctrl Pts',(13.6753055225219,-15.5,7.79950502406712));
#29261=CARTESIAN_POINT('Ctrl Pts',(14.1314791418914,-16.2901158858206,7.75783835740046));
#29262=CARTESIAN_POINT('Ctrl Pts',(14.5876527612609,-17.0802317716412,7.71617169073378));
#29263=CARTESIAN_POINT('Ctrl Pts',(15.5,-17.0802317716412,7.67450502406712));
#29264=CARTESIAN_POINT('Ctrl Pts',(16.4123472387391,-17.0802317716412,7.63283835740045));
#29265=CARTESIAN_POINT('Ctrl Pts',(16.8685208581086,-16.2901158858206,7.59117169073379));
#29266=CARTESIAN_POINT('Ctrl Pts',(17.3246944774781,-15.5,7.54950502406712));
#29267=CARTESIAN_POINT('Ctrl Pts',(16.8685208581086,-14.7098841141794,7.50783835740045));
#29268=CARTESIAN_POINT('Ctrl Pts',(16.4123472387391,-13.9197682283588,7.46617169073379));
#29269=CARTESIAN_POINT('Ctrl Pts',(15.5,-13.9197682283588,7.42450502406712));
#29270=CARTESIAN_POINT('Ctrl Pts',(14.5876527612609,-13.9197682283588,7.38283835740045));
#29271=CARTESIAN_POINT('Ctrl Pts',(14.1314791418914,-14.7098841141794,7.34117169073378));
#29272=CARTESIAN_POINT('Ctrl Pts',(13.6753055225219,-15.5,7.29950502406711));
#29273=CARTESIAN_POINT('Ctrl Pts',(14.1314791418914,-16.2901158858206,7.25783835740045));
#29274=CARTESIAN_POINT('Ctrl Pts',(14.5876527612609,-17.0802317716412,7.21617169073378));
#29275=CARTESIAN_POINT('Ctrl Pts',(15.5,-17.0802317716412,7.17450502406711));
#29276=CARTESIAN_POINT('Ctrl Pts',(16.4123472387391,-17.0802317716412,7.13283835740044));
#29277=CARTESIAN_POINT('Ctrl Pts',(16.8685208581086,-16.2901158858206,7.09117169073378));
#29278=CARTESIAN_POINT('Ctrl Pts',(17.3246944774781,-15.5,7.04950502406711));
#29279=CARTESIAN_POINT('Ctrl Pts',(16.8685208581086,-14.7098841141794,7.00783835740045));
#29280=CARTESIAN_POINT('Ctrl Pts',(16.4123472387391,-13.9197682283588,6.96617169073378));
#29281=CARTESIAN_POINT('Ctrl Pts',(15.5,-13.9197682283588,6.92450502406711));
#29282=CARTESIAN_POINT('Ctrl Pts',(14.5876527612609,-13.9197682283588,6.88283835740044));
#29283=CARTESIAN_POINT('Ctrl Pts',(14.1314791418914,-14.7098841141794,6.84117169073378));
#29284=CARTESIAN_POINT('Ctrl Pts',(13.6753055225219,-15.5,6.79950502406711));
#29285=CARTESIAN_POINT('Ctrl Pts',(14.1314791418914,-16.2901158858206,6.75783835740044));
#29286=CARTESIAN_POINT('Ctrl Pts',(14.5876527612609,-17.0802317716412,6.71617169073377));
#29287=CARTESIAN_POINT('Ctrl Pts',(15.5,-17.0802317716412,6.67450502406711));
#29288=CARTESIAN_POINT('Ctrl Pts',(16.4123472387391,-17.0802317716412,6.63283835740044));
#29289=CARTESIAN_POINT('Ctrl Pts',(16.8685208581086,-16.2901158858206,6.59117169073377));
#29290=CARTESIAN_POINT('Ctrl Pts',(17.3246944774781,-15.5,6.54950502406711));
#29291=CARTESIAN_POINT('Ctrl Pts',(16.8685208581086,-14.7098841141794,6.50783835740044));
#29292=CARTESIAN_POINT('Ctrl Pts',(16.4123472387391,-13.9197682283588,6.46617169073377));
#29293=CARTESIAN_POINT('Ctrl Pts',(15.5,-13.9197682283588,6.4245050240671));
#29294=CARTESIAN_POINT('Ctrl Pts',(14.5876527612609,-13.9197682283588,6.38283835740044));
#29295=CARTESIAN_POINT('Ctrl Pts',(14.1314791418914,-14.7098841141794,6.34117169073377));
#29296=CARTESIAN_POINT('Ctrl Pts',(13.6753055225219,-15.5,6.2995050240671));
#29297=CARTESIAN_POINT('Ctrl Pts',(14.1314791418914,-16.2901158858206,6.25783835740044));
#29298=CARTESIAN_POINT('Ctrl Pts',(14.5876527612609,-17.0802317716412,6.21617169073377));
#29299=CARTESIAN_POINT('Ctrl Pts',(15.5,-17.0802317716412,6.1745050240671));
#29300=CARTESIAN_POINT('Ctrl Pts',(16.4123472387391,-17.0802317716412,6.13283835740043));
#29301=CARTESIAN_POINT('Ctrl Pts',(16.8685208581086,-16.2901158858206,6.09117169073377));
#29302=CARTESIAN_POINT('Ctrl Pts',(17.3246944774781,-15.5,6.0495050240671));
#29303=CARTESIAN_POINT('Ctrl Pts',(16.8685208581086,-14.7098841141794,6.00783835740043));
#29304=CARTESIAN_POINT('Ctrl Pts',(16.4123472387391,-13.9197682283588,5.96617169073376));
#29305=CARTESIAN_POINT('Ctrl Pts',(15.5,-13.9197682283588,5.9245050240671));
#29306=CARTESIAN_POINT('Ctrl Pts',(14.5876527612609,-13.9197682283588,5.88283835740043));
#29307=CARTESIAN_POINT('Ctrl Pts',(14.1314791418914,-14.7098841141794,5.84117169073376));
#29308=CARTESIAN_POINT('Ctrl Pts',(13.6753055225219,-15.5,5.79950502406709));
#29309=CARTESIAN_POINT('Ctrl Pts',(14.1314791418914,-16.2901158858206,5.75783835740043));
#29310=CARTESIAN_POINT('Ctrl Pts',(14.5876527612609,-17.0802317716412,5.71617169073376));
#29311=CARTESIAN_POINT('Ctrl Pts',(15.5,-17.0802317716412,5.67450502406709));
#29312=CARTESIAN_POINT('Ctrl Pts',(16.4123472387391,-17.0802317716412,5.63283835740043));
#29313=CARTESIAN_POINT('Ctrl Pts',(16.8685208581086,-16.2901158858206,5.59117169073376));
#29314=CARTESIAN_POINT('Ctrl Pts',(17.3246944774781,-15.5,5.54950502406709));
#29315=CARTESIAN_POINT('Ctrl Pts',(16.8685208581086,-14.7098841141794,5.50783835740043));
#29316=CARTESIAN_POINT('Ctrl Pts',(16.4123472387391,-13.9197682283588,5.46617169073376));
#29317=CARTESIAN_POINT('Ctrl Pts',(15.5,-13.9197682283588,5.42450502406709));
#29318=CARTESIAN_POINT('Ctrl Pts',(14.5876527612609,-13.9197682283588,5.38283835740042));
#29319=CARTESIAN_POINT('Ctrl Pts',(14.1314791418914,-14.7098841141794,5.34117169073376));
#29320=CARTESIAN_POINT('Ctrl Pts',(13.6753055225219,-15.5,5.29950502406709));
#29321=CARTESIAN_POINT('Ctrl Pts',(14.1314791418914,-16.2901158858206,5.25783835740042));
#29322=CARTESIAN_POINT('Ctrl Pts',(14.5876527612609,-17.0802317716412,5.21617169073375));
#29323=CARTESIAN_POINT('Ctrl Pts',(15.5,-17.0802317716412,5.17450502406709));
#29324=CARTESIAN_POINT('Ctrl Pts',(16.4123472387391,-17.0802317716412,5.13283835740042));
#29325=CARTESIAN_POINT('Ctrl Pts',(16.8685208581086,-16.2901158858206,5.09117169073375));
#29326=CARTESIAN_POINT('Ctrl Pts',(17.3246944774781,-15.5,5.04950502406708));
#29327=CARTESIAN_POINT('Ctrl Pts',(16.8685208581086,-14.7098841141794,5.00783835740042));
#29328=CARTESIAN_POINT('Ctrl Pts',(16.4123472387391,-13.9197682283588,4.96617169073375));
#29329=CARTESIAN_POINT('Ctrl Pts',(15.5,-13.9197682283588,4.92450502406708));
#29330=CARTESIAN_POINT('Ctrl Pts',(14.5876527612609,-13.9197682283588,4.88283835740042));
#29331=CARTESIAN_POINT('Ctrl Pts',(14.1314791418914,-14.7098841141794,4.84117169073375));
#29332=CARTESIAN_POINT('Ctrl Pts',(13.6753055225219,-15.5,4.79950502406708));
#29333=CARTESIAN_POINT('Ctrl Pts',(14.1314791418914,-16.2901158858206,4.75783835740041));
#29334=CARTESIAN_POINT('Ctrl Pts',(14.5876527612609,-17.0802317716412,4.71617169073375));
#29335=CARTESIAN_POINT('Ctrl Pts',(15.5,-17.0802317716412,4.67450502406708));
#29336=CARTESIAN_POINT('Ctrl Pts',(16.4123472387391,-17.0802317716412,4.63283835740041));
#29337=CARTESIAN_POINT('Ctrl Pts',(16.8685208581086,-16.2901158858206,4.59117169073375));
#29338=CARTESIAN_POINT('Ctrl Pts',(17.3246944774781,-15.5,4.54950502406708));
#29339=CARTESIAN_POINT('Ctrl Pts',(16.8685208581086,-14.7098841141794,4.50783835740041));
#29340=CARTESIAN_POINT('Ctrl Pts',(16.4123472387391,-13.9197682283588,4.46617169073374));
#29341=CARTESIAN_POINT('Ctrl Pts',(15.5,-13.9197682283588,4.42450502406708));
#29342=CARTESIAN_POINT('Ctrl Pts',(14.5876527612609,-13.9197682283588,4.38283835740041));
#29343=CARTESIAN_POINT('Ctrl Pts',(14.1314791418914,-14.7098841141794,4.34117169073374));
#29344=CARTESIAN_POINT('Ctrl Pts',(13.6753055225219,-15.5,4.29950502406708));
#29345=CARTESIAN_POINT('Ctrl Pts',(14.1314791418914,-16.2901158858206,4.25783835740041));
#29346=CARTESIAN_POINT('Ctrl Pts',(14.5876527612609,-17.0802317716412,4.21617169073374));
#29347=CARTESIAN_POINT('Ctrl Pts',(15.5,-17.0802317716412,4.17450502406707));
#29348=CARTESIAN_POINT('Ctrl Pts',(16.4123472387391,-17.0802317716412,4.13283835740041));
#29349=CARTESIAN_POINT('Ctrl Pts',(16.8685208581086,-16.2901158858206,4.09117169073374));
#29350=CARTESIAN_POINT('Ctrl Pts',(17.3246944774781,-15.5,4.04950502406707));
#29351=CARTESIAN_POINT('Ctrl Pts',(16.8685208581086,-14.7098841141794,4.0078383574004));
#29352=CARTESIAN_POINT('Ctrl Pts',(16.4123472387391,-13.9197682283588,3.96617169073374));
#29353=CARTESIAN_POINT('Ctrl Pts',(15.5,-13.9197682283588,3.92450502406707));
#29354=CARTESIAN_POINT('Ctrl Pts',(14.5876527612609,-13.9197682283588,3.8828383574004));
#29355=CARTESIAN_POINT('Ctrl Pts',(14.1314791418914,-14.7098841141794,3.84117169073374));
#29356=CARTESIAN_POINT('Ctrl Pts',(13.6753055225219,-15.5,3.79950502406707));
#29357=CARTESIAN_POINT('Ctrl Pts',(14.1314791418914,-16.2901158858206,3.7578383574004));
#29358=CARTESIAN_POINT('Ctrl Pts',(14.5876527612609,-17.0802317716412,3.71617169073373));
#29359=CARTESIAN_POINT('Ctrl Pts',(15.5,-17.0802317716412,3.67450502406707));
#29360=CARTESIAN_POINT('Ctrl Pts',(16.4123472387391,-17.0802317716412,3.6328383574004));
#29361=CARTESIAN_POINT('Ctrl Pts',(16.8685208581086,-16.2901158858206,3.59117169073373));
#29362=CARTESIAN_POINT('Ctrl Pts',(17.3246944774781,-15.5,3.54950502406707));
#29363=CARTESIAN_POINT('Ctrl Pts',(16.8685208581086,-14.7098841141794,3.5078383574004));
#29364=CARTESIAN_POINT('Ctrl Pts',(16.4123472387391,-13.9197682283588,3.46617169073373));
#29365=CARTESIAN_POINT('Ctrl Pts',(15.5,-13.9197682283588,3.42450502406706));
#29366=CARTESIAN_POINT('Ctrl Pts',(14.5876527612609,-13.9197682283588,3.3828383574004));
#29367=CARTESIAN_POINT('Ctrl Pts',(14.1314791418914,-14.7098841141794,3.34117169073373));
#29368=CARTESIAN_POINT('Ctrl Pts',(13.6753055225219,-15.5,3.29950502406706));
#29369=CARTESIAN_POINT('Ctrl Pts',(14.1314791418914,-16.2901158858206,3.2578383574004));
#29370=CARTESIAN_POINT('Ctrl Pts',(14.5876527612609,-17.0802317716412,3.21617169073373));
#29371=CARTESIAN_POINT('Ctrl Pts',(15.5,-17.0802317716412,3.17450502406706));
#29372=CARTESIAN_POINT('Ctrl Pts',(16.4123472387391,-17.0802317716412,3.13283835740039));
#29373=CARTESIAN_POINT('Ctrl Pts',(16.8685208581086,-16.2901158858206,3.09117169073373));
#29374=CARTESIAN_POINT('Ctrl Pts',(17.3246944774781,-15.5,3.04950502406706));
#29375=CARTESIAN_POINT('Ctrl Pts',(16.8685208581086,-14.7098841141794,3.00783835740039));
#29376=CARTESIAN_POINT('Ctrl Pts',(16.4123472387391,-13.9197682283588,2.96617169073372));
#29377=CARTESIAN_POINT('Ctrl Pts',(15.5,-13.9197682283588,2.92450502406706));
#29378=CARTESIAN_POINT('Ctrl Pts',(14.5876527612609,-13.9197682283588,2.88283835740039));
#29379=CARTESIAN_POINT('Ctrl Pts',(14.1314791418914,-14.7098841141794,2.84117169073372));
#29380=CARTESIAN_POINT('Ctrl Pts',(13.6753055225219,-15.5,2.79950502406705));
#29381=CARTESIAN_POINT('Ctrl Pts',(14.1314791418914,-16.2901158858206,2.75783835740039));
#29382=CARTESIAN_POINT('Ctrl Pts',(14.5876527612609,-17.0802317716412,2.71617169073372));
#29383=CARTESIAN_POINT('Ctrl Pts',(15.5,-17.0802317716412,2.67450502406705));
#29384=CARTESIAN_POINT('Ctrl Pts',(16.4123472387391,-17.0802317716412,2.63283835740039));
#29385=CARTESIAN_POINT('Ctrl Pts',(16.8685208581086,-16.2901158858206,2.59117169073372));
#29386=CARTESIAN_POINT('Ctrl Pts',(17.3246944774781,-15.5,2.54950502406705));
#29387=CARTESIAN_POINT('Ctrl Pts',(16.8685208581086,-14.7098841141794,2.50783835740038));
#29388=CARTESIAN_POINT('Ctrl Pts',(16.4123472387391,-13.9197682283588,2.46617169073372));
#29389=CARTESIAN_POINT('Ctrl Pts',(15.5,-13.9197682283588,2.42450502406705));
#29390=CARTESIAN_POINT('Ctrl Pts',(14.5876527612609,-13.9197682283588,2.38283835740038));
#29391=CARTESIAN_POINT('Ctrl Pts',(14.1314791418914,-14.7098841141794,2.34117169073371));
#29392=CARTESIAN_POINT('Ctrl Pts',(13.6753055225219,-15.5,2.29950502406705));
#29393=CARTESIAN_POINT('Ctrl Pts',(14.1314791418914,-16.2901158858206,2.25783835740038));
#29394=CARTESIAN_POINT('Ctrl Pts',(14.5876527612609,-17.0802317716412,2.21617169073371));
#29395=CARTESIAN_POINT('Ctrl Pts',(15.5,-17.0802317716412,2.17450502406705));
#29396=CARTESIAN_POINT('Ctrl Pts',(16.4123472387391,-17.0802317716412,2.13283835740038));
#29397=CARTESIAN_POINT('Ctrl Pts',(16.8685208581086,-16.2901158858206,2.09117169073371));
#29398=CARTESIAN_POINT('Ctrl Pts',(17.3246944774781,-15.5,2.04950502406705));
#29399=CARTESIAN_POINT('Ctrl Pts',(16.8685208581086,-14.7098841141794,2.00783835740038));
#29400=CARTESIAN_POINT('Ctrl Pts',(16.4123472387391,-13.9197682283588,1.96617169073371));
#29401=CARTESIAN_POINT('Ctrl Pts',(15.5,-13.9197682283588,1.92450502406704));
#29402=CARTESIAN_POINT('Ctrl Pts',(14.5876527612609,-13.9197682283588,1.88283835740038));
#29403=CARTESIAN_POINT('Ctrl Pts',(14.1314791418914,-14.7098841141794,1.84117169073371));
#29404=CARTESIAN_POINT('Ctrl Pts',(13.6753055225219,-15.5,1.79950502406704));
#29405=CARTESIAN_POINT('Ctrl Pts',(14.1314791418914,-16.2901158858206,1.75783835740037));
#29406=CARTESIAN_POINT('Ctrl Pts',(14.5876527612609,-17.0802317716412,1.71617169073371));
#29407=CARTESIAN_POINT('Ctrl Pts',(15.5,-17.0802317716412,1.67450502406704));
#29408=CARTESIAN_POINT('Ctrl Pts',(16.4123472387391,-17.0802317716412,1.63283835740037));
#29409=CARTESIAN_POINT('Ctrl Pts',(16.8685208581086,-16.2901158858206,1.59117169073371));
#29410=CARTESIAN_POINT('Ctrl Pts',(17.3246944774781,-15.5,1.54950502406704));
#29411=CARTESIAN_POINT('Ctrl Pts',(16.8685208581086,-14.7098841141794,1.50783835740037));
#29412=CARTESIAN_POINT('Ctrl Pts',(16.4123472387391,-13.9197682283588,1.4661716907337));
#29413=CARTESIAN_POINT('Ctrl Pts',(15.5,-13.9197682283588,1.42450502406704));
#29414=CARTESIAN_POINT('Ctrl Pts',(14.5876527612609,-13.9197682283588,1.38283835740037));
#29415=CARTESIAN_POINT('Ctrl Pts',(14.1314791418914,-14.7098841141794,1.3411716907337));
#29416=CARTESIAN_POINT('Ctrl Pts',(13.6753055225219,-15.5,1.29950502406703));
#29417=CARTESIAN_POINT('Ctrl Pts',(14.1314791418914,-16.2901158858206,1.25783835740037));
#29418=CARTESIAN_POINT('Ctrl Pts',(14.5876527612609,-17.0802317716412,1.2161716907337));
#29419=CARTESIAN_POINT('Ctrl Pts',(15.5,-17.0802317716412,1.17450502406703));
#29420=CARTESIAN_POINT('Ctrl Pts',(16.4123472387391,-17.0802317716412,1.13283835740037));
#29421=CARTESIAN_POINT('Ctrl Pts',(16.8685208581086,-16.2901158858206,1.0911716907337));
#29422=CARTESIAN_POINT('Ctrl Pts',(17.3246944774781,-15.5,1.04950502406703));
#29423=CARTESIAN_POINT('Ctrl Pts',(16.8685208581086,-14.7098841141794,1.00783835740037));
#29424=CARTESIAN_POINT('Ctrl Pts',(16.4123472387391,-13.9197682283588,0.966171690733698));
#29425=CARTESIAN_POINT('Ctrl Pts',(15.5,-13.9197682283588,0.924505024067031));
#29426=CARTESIAN_POINT('Ctrl Pts',(14.5876527612609,-13.9197682283588,0.882838357400363));
#29427=CARTESIAN_POINT('Ctrl Pts',(14.1314791418914,-14.7098841141794,0.841171690733696));
#29428=CARTESIAN_POINT('Ctrl Pts',(13.6753055225219,-15.5,0.799505024067029));
#29429=CARTESIAN_POINT('Ctrl Pts',(14.1314791418914,-16.2901158858206,0.757838357400362));
#29430=CARTESIAN_POINT('Ctrl Pts',(14.5876527612609,-17.0802317716412,0.716171690733694));
#29431=CARTESIAN_POINT('Ctrl Pts',(15.5,-17.0802317716412,0.674505024067027));
#29432=CARTESIAN_POINT('Ctrl Pts',(16.4123472387391,-17.0802317716412,0.632838357400359));
#29433=CARTESIAN_POINT('Ctrl Pts',(16.8685208581086,-16.2901158858206,0.591171690733692));
#29434=CARTESIAN_POINT('Ctrl Pts',(17.3246944774781,-15.5,0.549505024067025));
#29435=CARTESIAN_POINT('Ctrl Pts',(16.8685208581086,-14.7098841141794,0.507838357400358));
#29436=CARTESIAN_POINT('Ctrl Pts',(16.4123472387391,-13.9197682283588,0.46617169073369));
#29437=CARTESIAN_POINT('Ctrl Pts',(15.5,-13.9197682283588,0.424505024067023));
#29438=CARTESIAN_POINT('Ctrl Pts',(14.5876527612609,-13.9197682283588,0.382838357400356));
#29439=CARTESIAN_POINT('Ctrl Pts',(14.1314791418914,-14.7098841141794,0.341171690733689));
#29440=CARTESIAN_POINT('Ctrl Pts',(13.6753055225219,-15.5,0.299505024067021));
#29441=CARTESIAN_POINT('Ctrl Pts',(14.1314791418914,-16.2901158858206,0.257838357400354));
#29442=CARTESIAN_POINT('Ctrl Pts',(14.5876527612609,-17.0802317716412,0.216171690733687));
#29443=CARTESIAN_POINT('Ctrl Pts',(15.5,-17.0802317716412,0.174505024067019));
#29444=CARTESIAN_POINT('Ctrl Pts',(16.4123472387391,-17.0802317716412,0.132838357400352));
#29445=CARTESIAN_POINT('Ctrl Pts',(16.8685208581086,-16.2901158858206,0.0911716907336849));
#29446=CARTESIAN_POINT('Ctrl Pts',(17.3246944774781,-15.5,0.0495050240670176));
#29447=CARTESIAN_POINT('Ctrl Pts',(16.8685208581086,-14.7098841141794,0.00783835740035031));
#29448=CARTESIAN_POINT('Ctrl Pts',(16.4123472387391,-13.9197682283588,-0.033828309266317));
#29449=CARTESIAN_POINT('Ctrl Pts',(15.5,-13.9197682283588,-0.0754949759329843));
#29450=CARTESIAN_POINT('Ctrl Pts',(14.5876527612609,-13.9197682283588,-0.11716164259965));
#29451=CARTESIAN_POINT('Ctrl Pts',(14.1314791418914,-14.7098841141794,-0.158828309266317));
#29452=CARTESIAN_POINT('Ctrl Pts',(13.6753055225219,-15.5,-0.200494975932984));
#29453=CARTESIAN_POINT('Ctrl Pts',(14.1314791418914,-16.2901158858206,-0.242161642599652));
#29454=CARTESIAN_POINT('Ctrl Pts',(14.5876527612609,-17.0802317716412,-0.283828309266319));
#29455=CARTESIAN_POINT('Ctrl Pts',(15.5,-17.0802317716412,-0.325494975932986));
#29456=CARTESIAN_POINT('Ctrl Pts',(16.4123472387391,-17.0802317716412,-0.367161642599654));
#29457=CARTESIAN_POINT('Ctrl Pts',(16.8685208581086,-16.2901158858206,-0.408828309266321));
#29458=CARTESIAN_POINT('Ctrl Pts',(17.3246944774781,-15.5,-0.450494975932988));
#29459=CARTESIAN_POINT('Ctrl Pts',(16.8685208581086,-14.7098841141794,-0.492161642599655));
#29460=CARTESIAN_POINT('Ctrl Pts',(16.4123472387391,-13.9197682283588,-0.533828309266323));
#29461=CARTESIAN_POINT('Ctrl Pts',(15.5,-13.9197682283588,-0.57549497593299));
#29462=CARTESIAN_POINT('Ctrl Pts',(14.5876527612609,-13.9197682283588,-0.617161642599657));
#29463=CARTESIAN_POINT('Ctrl Pts',(14.1314791418914,-14.7098841141794,-0.658828309266325));
#29464=CARTESIAN_POINT('Ctrl Pts',(13.6753055225219,-15.5,-0.700494975932992));
#29465=CARTESIAN_POINT('Ctrl Pts',(14.1314791418914,-16.2901158858206,-0.742161642599659));
#29466=CARTESIAN_POINT('Ctrl Pts',(14.5876527612609,-17.0802317716412,-0.783828309266326));
#29467=CARTESIAN_POINT('Ctrl Pts',(15.5,-17.0802317716412,-0.825494975932993));
#29468=CARTESIAN_POINT('Ctrl Pts',(16.4123472387391,-17.0802317716412,-0.867161642599661));
#29469=CARTESIAN_POINT('Ctrl Pts',(16.8685208581086,-16.2901158858206,-0.908828309266328));
#29470=CARTESIAN_POINT('Ctrl Pts',(17.3246944774781,-15.5,-0.950494975932995));
#29471=CARTESIAN_POINT('Ctrl Pts',(16.8685208581086,-14.7098841141794,-0.992161642599663));
#29472=CARTESIAN_POINT('Ctrl Pts',(16.4123472387391,-13.9197682283588,-1.03382830926633));
#29473=CARTESIAN_POINT('Ctrl Pts',(15.5,-13.9197682283588,-1.075494975933));
#29474=CARTESIAN_POINT('Ctrl Pts',(14.5876527612609,-13.9197682283588,-1.11716164259966));
#29475=CARTESIAN_POINT('Ctrl Pts',(14.1314791418914,-14.7098841141794,-1.15882830926633));
#29476=CARTESIAN_POINT('Ctrl Pts',(13.6753055225219,-15.5,-1.200494975933));
#29477=CARTESIAN_POINT('Ctrl Pts',(14.1314791418914,-16.2901158858206,-1.24216164259967));
#29478=CARTESIAN_POINT('Ctrl Pts',(14.5876527612609,-17.0802317716412,-1.28382830926633));
#29479=CARTESIAN_POINT('Ctrl Pts',(15.5,-17.0802317716412,-1.325494975933));
#29480=CARTESIAN_POINT('Ctrl Pts',(16.4123472387391,-17.0802317716412,-1.36716164259967));
#29481=CARTESIAN_POINT('Ctrl Pts',(16.8685208581086,-16.2901158858206,-1.40882830926633));
#29482=CARTESIAN_POINT('Ctrl Pts',(17.3246944774781,-15.5,-1.450494975933));
#29483=CARTESIAN_POINT('Ctrl Pts',(16.8685208581086,-14.7098841141794,-1.49216164259967));
#29484=CARTESIAN_POINT('Ctrl Pts',(16.4123472387391,-13.9197682283588,-1.53382830926634));
#29485=CARTESIAN_POINT('Ctrl Pts',(15.5,-13.9197682283588,-1.575494975933));
#29486=CARTESIAN_POINT('Ctrl Pts',(14.5876527612609,-13.9197682283588,-1.61716164259967));
#29487=CARTESIAN_POINT('Ctrl Pts',(14.1314791418914,-14.7098841141794,-1.65882830926634));
#29488=CARTESIAN_POINT('Ctrl Pts',(13.6753055225219,-15.5,-1.70049497593301));
#29489=CARTESIAN_POINT('Ctrl Pts',(14.1314791418914,-16.2901158858206,-1.74216164259967));
#29490=CARTESIAN_POINT('Ctrl Pts',(14.5876527612609,-17.0802317716412,-1.78382830926634));
#29491=CARTESIAN_POINT('Ctrl Pts',(15.5,-17.0802317716412,-1.82549497593301));
#29492=CARTESIAN_POINT('Ctrl Pts',(16.4123472387391,-17.0802317716412,-1.86716164259967));
#29493=CARTESIAN_POINT('Ctrl Pts',(16.8685208581086,-16.2901158858206,-1.90882830926634));
#29494=CARTESIAN_POINT('Ctrl Pts',(17.3246944774781,-15.5,-1.95049497593301));
#29495=CARTESIAN_POINT('Ctrl Pts',(16.8685208581086,-14.7098841141794,-1.99216164259968));
#29496=CARTESIAN_POINT('Ctrl Pts',(16.7005726719216,-14.4189893226644,-2.00750194461187));
#29497=CARTESIAN_POINT('Ctrl Pts',(16.4288249477777,-14.2215569357652,-2.02511838079831));
#29498=CARTESIAN_POINT('Ctrl Pts',(15.5,-17.4320632938683,10.971375));
#29499=CARTESIAN_POINT('Ctrl Pts',(16.6154772628062,-17.4320632938683,10.9297083333333));
#29500=CARTESIAN_POINT('Ctrl Pts',(17.1732158942094,-16.4660316469341,10.8880416666667));
#29501=CARTESIAN_POINT('Ctrl Pts',(17.7309545256125,-15.5,10.846375));
#29502=CARTESIAN_POINT('Ctrl Pts',(17.1732158942094,-14.5339683530659,10.8047083333333));
#29503=CARTESIAN_POINT('Ctrl Pts',(16.6154772628062,-13.5679367061317,10.7630416666667));
#29504=CARTESIAN_POINT('Ctrl Pts',(15.5,-13.5679367061317,10.721375));
#29505=CARTESIAN_POINT('Ctrl Pts',(14.3845227371938,-13.5679367061317,10.6797083333333));
#29506=CARTESIAN_POINT('Ctrl Pts',(13.8267841057906,-14.5339683530659,10.6380416666667));
#29507=CARTESIAN_POINT('Ctrl Pts',(13.2690454743875,-15.5,10.596375));
#29508=CARTESIAN_POINT('Ctrl Pts',(13.8267841057906,-16.4660316469341,10.5547083333333));
#29509=CARTESIAN_POINT('Ctrl Pts',(14.3845227371938,-17.4320632938683,10.5130416666667));
#29510=CARTESIAN_POINT('Ctrl Pts',(15.5,-17.4320632938683,10.471375));
#29511=CARTESIAN_POINT('Ctrl Pts',(16.6154772628062,-17.4320632938683,10.4297083333333));
#29512=CARTESIAN_POINT('Ctrl Pts',(17.1732158942094,-16.4660316469341,10.3880416666667));
#29513=CARTESIAN_POINT('Ctrl Pts',(17.7309545256125,-15.5,10.346375));
#29514=CARTESIAN_POINT('Ctrl Pts',(17.1732158942094,-14.5339683530659,10.3047083333333));
#29515=CARTESIAN_POINT('Ctrl Pts',(16.6154772628062,-13.5679367061317,10.2630416666667));
#29516=CARTESIAN_POINT('Ctrl Pts',(15.5,-13.5679367061317,10.221375));
#29517=CARTESIAN_POINT('Ctrl Pts',(14.3845227371938,-13.5679367061317,10.1797083333333));
#29518=CARTESIAN_POINT('Ctrl Pts',(13.8267841057906,-14.5339683530659,10.1380416666667));
#29519=CARTESIAN_POINT('Ctrl Pts',(13.2690454743875,-15.5,10.096375));
#29520=CARTESIAN_POINT('Ctrl Pts',(13.8267841057906,-16.4660316469341,10.0547083333333));
#29521=CARTESIAN_POINT('Ctrl Pts',(14.3845227371938,-17.4320632938683,10.0130416666666));
#29522=CARTESIAN_POINT('Ctrl Pts',(15.5,-17.4320632938683,9.97137499999998));
#29523=CARTESIAN_POINT('Ctrl Pts',(16.6154772628062,-17.4320632938683,9.92970833333332));
#29524=CARTESIAN_POINT('Ctrl Pts',(17.1732158942094,-16.4660316469341,9.88804166666665));
#29525=CARTESIAN_POINT('Ctrl Pts',(17.7309545256125,-15.5,9.84637499999998));
#29526=CARTESIAN_POINT('Ctrl Pts',(17.1732158942094,-14.5339683530659,9.80470833333331));
#29527=CARTESIAN_POINT('Ctrl Pts',(16.6154772628062,-13.5679367061317,9.76304166666665));
#29528=CARTESIAN_POINT('Ctrl Pts',(15.5,-13.5679367061317,9.72137499999998));
#29529=CARTESIAN_POINT('Ctrl Pts',(14.3845227371938,-13.5679367061317,9.67970833333331));
#29530=CARTESIAN_POINT('Ctrl Pts',(13.8267841057906,-14.5339683530659,9.63804166666664));
#29531=CARTESIAN_POINT('Ctrl Pts',(13.2690454743875,-15.5,9.59637499999998));
#29532=CARTESIAN_POINT('Ctrl Pts',(13.8267841057906,-16.4660316469341,9.55470833333331));
#29533=CARTESIAN_POINT('Ctrl Pts',(14.3845227371938,-17.4320632938683,9.51304166666664));
#29534=CARTESIAN_POINT('Ctrl Pts',(15.5,-17.4320632938683,9.47137499999998));
#29535=CARTESIAN_POINT('Ctrl Pts',(16.6154772628062,-17.4320632938683,9.42970833333331));
#29536=CARTESIAN_POINT('Ctrl Pts',(17.1732158942094,-16.4660316469341,9.38804166666664));
#29537=CARTESIAN_POINT('Ctrl Pts',(17.7309545256125,-15.5,9.34637499999997));
#29538=CARTESIAN_POINT('Ctrl Pts',(17.1732158942094,-14.5339683530659,9.30470833333331));
#29539=CARTESIAN_POINT('Ctrl Pts',(16.6154772628062,-13.5679367061317,9.26304166666664));
#29540=CARTESIAN_POINT('Ctrl Pts',(15.5,-13.5679367061317,9.22137499999997));
#29541=CARTESIAN_POINT('Ctrl Pts',(14.3845227371938,-13.5679367061317,9.1797083333333));
#29542=CARTESIAN_POINT('Ctrl Pts',(13.8267841057906,-14.5339683530659,9.13804166666664));
#29543=CARTESIAN_POINT('Ctrl Pts',(13.2690454743875,-15.5,9.09637499999997));
#29544=CARTESIAN_POINT('Ctrl Pts',(13.8267841057906,-16.4660316469341,9.0547083333333));
#29545=CARTESIAN_POINT('Ctrl Pts',(14.3845227371938,-17.4320632938683,9.01304166666664));
#29546=CARTESIAN_POINT('Ctrl Pts',(15.5,-17.4320632938683,8.97137499999997));
#29547=CARTESIAN_POINT('Ctrl Pts',(16.6154772628062,-17.4320632938683,8.9297083333333));
#29548=CARTESIAN_POINT('Ctrl Pts',(17.1732158942094,-16.4660316469341,8.88804166666663));
#29549=CARTESIAN_POINT('Ctrl Pts',(17.7309545256125,-15.5,8.84637499999997));
#29550=CARTESIAN_POINT('Ctrl Pts',(17.1732158942094,-14.5339683530659,8.8047083333333));
#29551=CARTESIAN_POINT('Ctrl Pts',(16.6154772628062,-13.5679367061317,8.76304166666663));
#29552=CARTESIAN_POINT('Ctrl Pts',(15.5,-13.5679367061317,8.72137499999997));
#29553=CARTESIAN_POINT('Ctrl Pts',(14.3845227371938,-13.5679367061317,8.6797083333333));
#29554=CARTESIAN_POINT('Ctrl Pts',(13.8267841057906,-14.5339683530659,8.63804166666663));
#29555=CARTESIAN_POINT('Ctrl Pts',(13.2690454743875,-15.5,8.59637499999996));
#29556=CARTESIAN_POINT('Ctrl Pts',(13.8267841057906,-16.4660316469341,8.5547083333333));
#29557=CARTESIAN_POINT('Ctrl Pts',(14.3845227371938,-17.4320632938683,8.51304166666663));
#29558=CARTESIAN_POINT('Ctrl Pts',(15.5,-17.4320632938683,8.47137499999996));
#29559=CARTESIAN_POINT('Ctrl Pts',(16.6154772628062,-17.4320632938683,8.42970833333329));
#29560=CARTESIAN_POINT('Ctrl Pts',(17.1732158942094,-16.4660316469341,8.38804166666663));
#29561=CARTESIAN_POINT('Ctrl Pts',(17.7309545256125,-15.5,8.34637499999996));
#29562=CARTESIAN_POINT('Ctrl Pts',(17.1732158942094,-14.5339683530659,8.30470833333329));
#29563=CARTESIAN_POINT('Ctrl Pts',(16.6154772628062,-13.5679367061317,8.26304166666663));
#29564=CARTESIAN_POINT('Ctrl Pts',(15.5,-13.5679367061317,8.22137499999996));
#29565=CARTESIAN_POINT('Ctrl Pts',(14.3845227371938,-13.5679367061317,8.17970833333329));
#29566=CARTESIAN_POINT('Ctrl Pts',(13.8267841057906,-14.5339683530659,8.13804166666662));
#29567=CARTESIAN_POINT('Ctrl Pts',(13.2690454743875,-15.5,8.09637499999996));
#29568=CARTESIAN_POINT('Ctrl Pts',(13.8267841057906,-16.4660316469341,8.05470833333329));
#29569=CARTESIAN_POINT('Ctrl Pts',(14.3845227371938,-17.4320632938683,8.01304166666662));
#29570=CARTESIAN_POINT('Ctrl Pts',(15.5,-17.4320632938683,7.97137499999995));
#29571=CARTESIAN_POINT('Ctrl Pts',(16.6154772628062,-17.4320632938683,7.92970833333329));
#29572=CARTESIAN_POINT('Ctrl Pts',(17.1732158942094,-16.4660316469341,7.88804166666662));
#29573=CARTESIAN_POINT('Ctrl Pts',(17.7309545256125,-15.5,7.84637499999995));
#29574=CARTESIAN_POINT('Ctrl Pts',(17.1732158942094,-14.5339683530659,7.80470833333329));
#29575=CARTESIAN_POINT('Ctrl Pts',(16.6154772628062,-13.5679367061317,7.76304166666662));
#29576=CARTESIAN_POINT('Ctrl Pts',(15.5,-13.5679367061317,7.72137499999995));
#29577=CARTESIAN_POINT('Ctrl Pts',(14.3845227371938,-13.5679367061317,7.67970833333329));
#29578=CARTESIAN_POINT('Ctrl Pts',(13.8267841057906,-14.5339683530659,7.63804166666662));
#29579=CARTESIAN_POINT('Ctrl Pts',(13.2690454743875,-15.5,7.59637499999995));
#29580=CARTESIAN_POINT('Ctrl Pts',(13.8267841057906,-16.4660316469341,7.55470833333328));
#29581=CARTESIAN_POINT('Ctrl Pts',(14.3845227371938,-17.4320632938683,7.51304166666662));
#29582=CARTESIAN_POINT('Ctrl Pts',(15.5,-17.4320632938683,7.47137499999995));
#29583=CARTESIAN_POINT('Ctrl Pts',(16.6154772628062,-17.4320632938683,7.42970833333328));
#29584=CARTESIAN_POINT('Ctrl Pts',(17.1732158942094,-16.4660316469341,7.38804166666661));
#29585=CARTESIAN_POINT('Ctrl Pts',(17.7309545256125,-15.5,7.34637499999995));
#29586=CARTESIAN_POINT('Ctrl Pts',(17.1732158942094,-14.5339683530659,7.30470833333328));
#29587=CARTESIAN_POINT('Ctrl Pts',(16.6154772628062,-13.5679367061317,7.26304166666661));
#29588=CARTESIAN_POINT('Ctrl Pts',(15.5,-13.5679367061317,7.22137499999994));
#29589=CARTESIAN_POINT('Ctrl Pts',(14.3845227371938,-13.5679367061317,7.17970833333328));
#29590=CARTESIAN_POINT('Ctrl Pts',(13.8267841057906,-14.5339683530659,7.13804166666661));
#29591=CARTESIAN_POINT('Ctrl Pts',(13.2690454743875,-15.5,7.09637499999995));
#29592=CARTESIAN_POINT('Ctrl Pts',(13.8267841057906,-16.4660316469341,7.05470833333328));
#29593=CARTESIAN_POINT('Ctrl Pts',(14.3845227371938,-17.4320632938683,7.01304166666661));
#29594=CARTESIAN_POINT('Ctrl Pts',(15.5,-17.4320632938683,6.97137499999994));
#29595=CARTESIAN_POINT('Ctrl Pts',(16.6154772628062,-17.4320632938683,6.92970833333328));
#29596=CARTESIAN_POINT('Ctrl Pts',(17.1732158942094,-16.4660316469341,6.88804166666661));
#29597=CARTESIAN_POINT('Ctrl Pts',(17.7309545256125,-15.5,6.84637499999994));
#29598=CARTESIAN_POINT('Ctrl Pts',(17.1732158942094,-14.5339683530659,6.80470833333327));
#29599=CARTESIAN_POINT('Ctrl Pts',(16.6154772628062,-13.5679367061317,6.76304166666661));
#29600=CARTESIAN_POINT('Ctrl Pts',(15.5,-13.5679367061317,6.72137499999994));
#29601=CARTESIAN_POINT('Ctrl Pts',(14.3845227371938,-13.5679367061317,6.67970833333327));
#29602=CARTESIAN_POINT('Ctrl Pts',(13.8267841057906,-14.5339683530659,6.6380416666666));
#29603=CARTESIAN_POINT('Ctrl Pts',(13.2690454743875,-15.5,6.59637499999994));
#29604=CARTESIAN_POINT('Ctrl Pts',(13.8267841057906,-16.4660316469341,6.55470833333327));
#29605=CARTESIAN_POINT('Ctrl Pts',(14.3845227371938,-17.4320632938683,6.5130416666666));
#29606=CARTESIAN_POINT('Ctrl Pts',(15.5,-17.4320632938683,6.47137499999994));
#29607=CARTESIAN_POINT('Ctrl Pts',(16.6154772628062,-17.4320632938683,6.42970833333327));
#29608=CARTESIAN_POINT('Ctrl Pts',(17.1732158942094,-16.4660316469341,6.3880416666666));
#29609=CARTESIAN_POINT('Ctrl Pts',(17.7309545256125,-15.5,6.34637499999993));
#29610=CARTESIAN_POINT('Ctrl Pts',(17.1732158942094,-14.5339683530659,6.30470833333327));
#29611=CARTESIAN_POINT('Ctrl Pts',(16.6154772628062,-13.5679367061317,6.2630416666666));
#29612=CARTESIAN_POINT('Ctrl Pts',(15.5,-13.5679367061317,6.22137499999993));
#29613=CARTESIAN_POINT('Ctrl Pts',(14.3845227371938,-13.5679367061317,6.17970833333327));
#29614=CARTESIAN_POINT('Ctrl Pts',(13.8267841057906,-14.5339683530659,6.1380416666666));
#29615=CARTESIAN_POINT('Ctrl Pts',(13.2690454743875,-15.5,6.09637499999993));
#29616=CARTESIAN_POINT('Ctrl Pts',(13.8267841057906,-16.4660316469341,6.05470833333326));
#29617=CARTESIAN_POINT('Ctrl Pts',(14.3845227371938,-17.4320632938683,6.0130416666666));
#29618=CARTESIAN_POINT('Ctrl Pts',(15.5,-17.4320632938683,5.97137499999993));
#29619=CARTESIAN_POINT('Ctrl Pts',(16.6154772628062,-17.4320632938683,5.92970833333326));
#29620=CARTESIAN_POINT('Ctrl Pts',(17.1732158942094,-16.4660316469341,5.8880416666666));
#29621=CARTESIAN_POINT('Ctrl Pts',(17.7309545256125,-15.5,5.84637499999993));
#29622=CARTESIAN_POINT('Ctrl Pts',(17.1732158942094,-14.5339683530659,5.80470833333326));
#29623=CARTESIAN_POINT('Ctrl Pts',(16.6154772628062,-13.5679367061317,5.76304166666659));
#29624=CARTESIAN_POINT('Ctrl Pts',(15.5,-13.5679367061317,5.72137499999993));
#29625=CARTESIAN_POINT('Ctrl Pts',(14.3845227371938,-13.5679367061317,5.67970833333326));
#29626=CARTESIAN_POINT('Ctrl Pts',(13.8267841057906,-14.5339683530659,5.63804166666659));
#29627=CARTESIAN_POINT('Ctrl Pts',(13.2690454743875,-15.5,5.59637499999992));
#29628=CARTESIAN_POINT('Ctrl Pts',(13.8267841057906,-16.4660316469341,5.55470833333326));
#29629=CARTESIAN_POINT('Ctrl Pts',(14.3845227371938,-17.4320632938683,5.51304166666659));
#29630=CARTESIAN_POINT('Ctrl Pts',(15.5,-17.4320632938683,5.47137499999992));
#29631=CARTESIAN_POINT('Ctrl Pts',(16.6154772628062,-17.4320632938683,5.42970833333325));
#29632=CARTESIAN_POINT('Ctrl Pts',(17.1732158942094,-16.4660316469341,5.38804166666659));
#29633=CARTESIAN_POINT('Ctrl Pts',(17.7309545256125,-15.5,5.34637499999992));
#29634=CARTESIAN_POINT('Ctrl Pts',(17.1732158942094,-14.5339683530659,5.30470833333325));
#29635=CARTESIAN_POINT('Ctrl Pts',(16.6154772628062,-13.5679367061317,5.26304166666659));
#29636=CARTESIAN_POINT('Ctrl Pts',(15.5,-13.5679367061317,5.22137499999992));
#29637=CARTESIAN_POINT('Ctrl Pts',(14.3845227371938,-13.5679367061317,5.17970833333325));
#29638=CARTESIAN_POINT('Ctrl Pts',(13.8267841057906,-14.5339683530659,5.13804166666659));
#29639=CARTESIAN_POINT('Ctrl Pts',(13.2690454743875,-15.5,5.09637499999992));
#29640=CARTESIAN_POINT('Ctrl Pts',(13.8267841057906,-16.4660316469341,5.05470833333325));
#29641=CARTESIAN_POINT('Ctrl Pts',(14.3845227371938,-17.4320632938683,5.01304166666658));
#29642=CARTESIAN_POINT('Ctrl Pts',(15.5,-17.4320632938683,4.97137499999991));
#29643=CARTESIAN_POINT('Ctrl Pts',(16.6154772628062,-17.4320632938683,4.92970833333325));
#29644=CARTESIAN_POINT('Ctrl Pts',(17.1732158942094,-16.4660316469341,4.88804166666658));
#29645=CARTESIAN_POINT('Ctrl Pts',(17.7309545256125,-15.5,4.84637499999991));
#29646=CARTESIAN_POINT('Ctrl Pts',(17.1732158942094,-14.5339683530659,4.80470833333325));
#29647=CARTESIAN_POINT('Ctrl Pts',(16.6154772628062,-13.5679367061317,4.76304166666658));
#29648=CARTESIAN_POINT('Ctrl Pts',(15.5,-13.5679367061317,4.72137499999991));
#29649=CARTESIAN_POINT('Ctrl Pts',(14.3845227371938,-13.5679367061317,4.67970833333325));
#29650=CARTESIAN_POINT('Ctrl Pts',(13.8267841057906,-14.5339683530659,4.63804166666658));
#29651=CARTESIAN_POINT('Ctrl Pts',(13.2690454743875,-15.5,4.59637499999991));
#29652=CARTESIAN_POINT('Ctrl Pts',(13.8267841057906,-16.4660316469341,4.55470833333324));
#29653=CARTESIAN_POINT('Ctrl Pts',(14.3845227371938,-17.4320632938683,4.51304166666658));
#29654=CARTESIAN_POINT('Ctrl Pts',(15.5,-17.4320632938683,4.47137499999991));
#29655=CARTESIAN_POINT('Ctrl Pts',(16.6154772628062,-17.4320632938683,4.42970833333324));
#29656=CARTESIAN_POINT('Ctrl Pts',(17.1732158942094,-16.4660316469341,4.38804166666657));
#29657=CARTESIAN_POINT('Ctrl Pts',(17.7309545256125,-15.5,4.34637499999991));
#29658=CARTESIAN_POINT('Ctrl Pts',(17.1732158942094,-14.5339683530659,4.30470833333324));
#29659=CARTESIAN_POINT('Ctrl Pts',(16.6154772628062,-13.5679367061317,4.26304166666657));
#29660=CARTESIAN_POINT('Ctrl Pts',(15.5,-13.5679367061317,4.22137499999991));
#29661=CARTESIAN_POINT('Ctrl Pts',(14.3845227371938,-13.5679367061317,4.17970833333324));
#29662=CARTESIAN_POINT('Ctrl Pts',(13.8267841057906,-14.5339683530659,4.13804166666657));
#29663=CARTESIAN_POINT('Ctrl Pts',(13.2690454743875,-15.5,4.0963749999999));
#29664=CARTESIAN_POINT('Ctrl Pts',(13.8267841057906,-16.4660316469341,4.05470833333324));
#29665=CARTESIAN_POINT('Ctrl Pts',(14.3845227371938,-17.4320632938683,4.01304166666657));
#29666=CARTESIAN_POINT('Ctrl Pts',(15.5,-17.4320632938683,3.9713749999999));
#29667=CARTESIAN_POINT('Ctrl Pts',(16.6154772628062,-17.4320632938683,3.92970833333323));
#29668=CARTESIAN_POINT('Ctrl Pts',(17.1732158942094,-16.4660316469341,3.88804166666657));
#29669=CARTESIAN_POINT('Ctrl Pts',(17.7309545256125,-15.5,3.8463749999999));
#29670=CARTESIAN_POINT('Ctrl Pts',(17.1732158942094,-14.5339683530659,3.80470833333323));
#29671=CARTESIAN_POINT('Ctrl Pts',(16.6154772628062,-13.5679367061317,3.76304166666656));
#29672=CARTESIAN_POINT('Ctrl Pts',(15.5,-13.5679367061317,3.7213749999999));
#29673=CARTESIAN_POINT('Ctrl Pts',(14.3845227371938,-13.5679367061317,3.67970833333323));
#29674=CARTESIAN_POINT('Ctrl Pts',(13.8267841057906,-14.5339683530659,3.63804166666656));
#29675=CARTESIAN_POINT('Ctrl Pts',(13.2690454743875,-15.5,3.5963749999999));
#29676=CARTESIAN_POINT('Ctrl Pts',(13.8267841057906,-16.4660316469341,3.55470833333323));
#29677=CARTESIAN_POINT('Ctrl Pts',(14.3845227371938,-17.4320632938683,3.51304166666656));
#29678=CARTESIAN_POINT('Ctrl Pts',(15.5,-17.4320632938683,3.4713749999999));
#29679=CARTESIAN_POINT('Ctrl Pts',(16.6154772628062,-17.4320632938683,3.42970833333323));
#29680=CARTESIAN_POINT('Ctrl Pts',(17.1732158942094,-16.4660316469341,3.38804166666656));
#29681=CARTESIAN_POINT('Ctrl Pts',(17.7309545256125,-15.5,3.34637499999989));
#29682=CARTESIAN_POINT('Ctrl Pts',(17.1732158942094,-14.5339683530659,3.30470833333323));
#29683=CARTESIAN_POINT('Ctrl Pts',(16.6154772628062,-13.5679367061317,3.26304166666656));
#29684=CARTESIAN_POINT('Ctrl Pts',(15.5,-13.5679367061317,3.22137499999989));
#29685=CARTESIAN_POINT('Ctrl Pts',(14.3845227371938,-13.5679367061317,3.17970833333322));
#29686=CARTESIAN_POINT('Ctrl Pts',(13.8267841057906,-14.5339683530659,3.13804166666656));
#29687=CARTESIAN_POINT('Ctrl Pts',(13.2690454743875,-15.5,3.09637499999989));
#29688=CARTESIAN_POINT('Ctrl Pts',(13.8267841057906,-16.4660316469341,3.05470833333322));
#29689=CARTESIAN_POINT('Ctrl Pts',(14.3845227371938,-17.4320632938683,3.01304166666656));
#29690=CARTESIAN_POINT('Ctrl Pts',(15.5,-17.4320632938683,2.97137499999989));
#29691=CARTESIAN_POINT('Ctrl Pts',(16.6154772628062,-17.4320632938683,2.92970833333322));
#29692=CARTESIAN_POINT('Ctrl Pts',(17.1732158942094,-16.4660316469341,2.88804166666655));
#29693=CARTESIAN_POINT('Ctrl Pts',(17.7309545256125,-15.5,2.84637499999989));
#29694=CARTESIAN_POINT('Ctrl Pts',(17.1732158942094,-14.5339683530659,2.80470833333322));
#29695=CARTESIAN_POINT('Ctrl Pts',(16.6154772628062,-13.5679367061317,2.76304166666655));
#29696=CARTESIAN_POINT('Ctrl Pts',(15.5,-13.5679367061317,2.72137499999989));
#29697=CARTESIAN_POINT('Ctrl Pts',(14.3845227371938,-13.5679367061317,2.67970833333322));
#29698=CARTESIAN_POINT('Ctrl Pts',(13.8267841057906,-14.5339683530659,2.63804166666655));
#29699=CARTESIAN_POINT('Ctrl Pts',(13.2690454743875,-15.5,2.59637499999988));
#29700=CARTESIAN_POINT('Ctrl Pts',(13.8267841057906,-16.4660316469341,2.55470833333322));
#29701=CARTESIAN_POINT('Ctrl Pts',(14.3845227371938,-17.4320632938683,2.51304166666655));
#29702=CARTESIAN_POINT('Ctrl Pts',(15.5,-17.4320632938683,2.47137499999988));
#29703=CARTESIAN_POINT('Ctrl Pts',(16.6154772628062,-17.4320632938683,2.42970833333321));
#29704=CARTESIAN_POINT('Ctrl Pts',(17.1732158942094,-16.4660316469341,2.38804166666655));
#29705=CARTESIAN_POINT('Ctrl Pts',(17.7309545256125,-15.5,2.34637499999988));
#29706=CARTESIAN_POINT('Ctrl Pts',(17.1732158942094,-14.5339683530659,2.30470833333321));
#29707=CARTESIAN_POINT('Ctrl Pts',(16.6154772628062,-13.5679367061317,2.26304166666655));
#29708=CARTESIAN_POINT('Ctrl Pts',(15.5,-13.5679367061317,2.22137499999988));
#29709=CARTESIAN_POINT('Ctrl Pts',(14.3845227371938,-13.5679367061317,2.17970833333321));
#29710=CARTESIAN_POINT('Ctrl Pts',(13.8267841057906,-14.5339683530659,2.13804166666654));
#29711=CARTESIAN_POINT('Ctrl Pts',(13.2690454743875,-15.5,2.09637499999988));
#29712=CARTESIAN_POINT('Ctrl Pts',(13.8267841057906,-16.4660316469341,2.05470833333321));
#29713=CARTESIAN_POINT('Ctrl Pts',(14.3845227371938,-17.4320632938683,2.01304166666654));
#29714=CARTESIAN_POINT('Ctrl Pts',(15.5,-17.4320632938683,1.97137499999988));
#29715=CARTESIAN_POINT('Ctrl Pts',(16.6154772628062,-17.4320632938683,1.92970833333321));
#29716=CARTESIAN_POINT('Ctrl Pts',(17.1732158942094,-16.4660316469341,1.88804166666654));
#29717=CARTESIAN_POINT('Ctrl Pts',(17.7309545256125,-15.5,1.84637499999987));
#29718=CARTESIAN_POINT('Ctrl Pts',(17.1732158942094,-14.5339683530659,1.80470833333321));
#29719=CARTESIAN_POINT('Ctrl Pts',(16.6154772628062,-13.5679367061317,1.76304166666654));
#29720=CARTESIAN_POINT('Ctrl Pts',(15.5,-13.5679367061317,1.72137499999987));
#29721=CARTESIAN_POINT('Ctrl Pts',(14.3845227371938,-13.5679367061317,1.67970833333321));
#29722=CARTESIAN_POINT('Ctrl Pts',(13.8267841057906,-14.5339683530659,1.63804166666654));
#29723=CARTESIAN_POINT('Ctrl Pts',(13.2690454743875,-15.5,1.59637499999987));
#29724=CARTESIAN_POINT('Ctrl Pts',(13.8267841057906,-16.4660316469341,1.5547083333332));
#29725=CARTESIAN_POINT('Ctrl Pts',(14.3845227371938,-17.4320632938683,1.51304166666654));
#29726=CARTESIAN_POINT('Ctrl Pts',(15.5,-17.4320632938683,1.47137499999987));
#29727=CARTESIAN_POINT('Ctrl Pts',(16.6154772628062,-17.4320632938683,1.4297083333332));
#29728=CARTESIAN_POINT('Ctrl Pts',(17.1732158942094,-16.4660316469341,1.38804166666653));
#29729=CARTESIAN_POINT('Ctrl Pts',(17.7309545256125,-15.5,1.34637499999987));
#29730=CARTESIAN_POINT('Ctrl Pts',(17.1732158942094,-14.5339683530659,1.3047083333332));
#29731=CARTESIAN_POINT('Ctrl Pts',(16.6154772628062,-13.5679367061317,1.26304166666653));
#29732=CARTESIAN_POINT('Ctrl Pts',(15.5,-13.5679367061317,1.22137499999987));
#29733=CARTESIAN_POINT('Ctrl Pts',(14.3845227371938,-13.5679367061317,1.1797083333332));
#29734=CARTESIAN_POINT('Ctrl Pts',(13.8267841057906,-14.5339683530659,1.13804166666653));
#29735=CARTESIAN_POINT('Ctrl Pts',(13.2690454743875,-15.5,1.09637499999986));
#29736=CARTESIAN_POINT('Ctrl Pts',(13.8267841057906,-16.4660316469341,1.0547083333332));
#29737=CARTESIAN_POINT('Ctrl Pts',(14.3845227371938,-17.4320632938683,1.01304166666653));
#29738=CARTESIAN_POINT('Ctrl Pts',(15.5,-17.4320632938683,0.971374999999861));
#29739=CARTESIAN_POINT('Ctrl Pts',(16.6154772628062,-17.4320632938683,0.929708333333194));
#29740=CARTESIAN_POINT('Ctrl Pts',(17.1732158942094,-16.4660316469341,0.888041666666528));
#29741=CARTESIAN_POINT('Ctrl Pts',(17.7309545256125,-15.5,0.846374999999861));
#29742=CARTESIAN_POINT('Ctrl Pts',(17.1732158942094,-14.5339683530659,0.804708333333194));
#29743=CARTESIAN_POINT('Ctrl Pts',(16.6154772628062,-13.5679367061317,0.763041666666526));
#29744=CARTESIAN_POINT('Ctrl Pts',(15.5,-13.5679367061317,0.721374999999859));
#29745=CARTESIAN_POINT('Ctrl Pts',(14.3845227371938,-13.5679367061317,0.679708333333192));
#29746=CARTESIAN_POINT('Ctrl Pts',(13.8267841057906,-14.5339683530659,0.638041666666525));
#29747=CARTESIAN_POINT('Ctrl Pts',(13.2690454743875,-15.5,0.596374999999858));
#29748=CARTESIAN_POINT('Ctrl Pts',(13.8267841057906,-16.4660316469341,0.55470833333319));
#29749=CARTESIAN_POINT('Ctrl Pts',(14.3845227371938,-17.4320632938683,0.513041666666523));
#29750=CARTESIAN_POINT('Ctrl Pts',(15.5,-17.4320632938683,0.471374999999856));
#29751=CARTESIAN_POINT('Ctrl Pts',(16.6154772628062,-17.4320632938683,0.429708333333188));
#29752=CARTESIAN_POINT('Ctrl Pts',(17.1732158942094,-16.4660316469341,0.388041666666521));
#29753=CARTESIAN_POINT('Ctrl Pts',(17.7309545256125,-15.5,0.346374999999854));
#29754=CARTESIAN_POINT('Ctrl Pts',(17.1732158942094,-14.5339683530659,0.304708333333186));
#29755=CARTESIAN_POINT('Ctrl Pts',(16.6154772628062,-13.5679367061317,0.263041666666519));
#29756=CARTESIAN_POINT('Ctrl Pts',(15.5,-13.5679367061317,0.221374999999852));
#29757=CARTESIAN_POINT('Ctrl Pts',(14.3845227371938,-13.5679367061317,0.179708333333185));
#29758=CARTESIAN_POINT('Ctrl Pts',(13.8267841057906,-14.5339683530659,0.138041666666517));
#29759=CARTESIAN_POINT('Ctrl Pts',(13.2690454743875,-15.5,0.0963749999998501));
#29760=CARTESIAN_POINT('Ctrl Pts',(13.8267841057906,-16.4660316469341,0.0547083333331828));
#29761=CARTESIAN_POINT('Ctrl Pts',(14.3845227371938,-17.4320632938683,0.0130416666665155));
#29762=CARTESIAN_POINT('Ctrl Pts',(15.5,-17.4320632938683,-0.0286250000001518));
#29763=CARTESIAN_POINT('Ctrl Pts',(16.6154772628062,-17.4320632938683,-0.0702916666668191));
#29764=CARTESIAN_POINT('Ctrl Pts',(17.1732158942094,-16.4660316469341,-0.111958333333486));
#29765=CARTESIAN_POINT('Ctrl Pts',(17.7309545256125,-15.5,-0.153625000000154));
#29766=CARTESIAN_POINT('Ctrl Pts',(17.1732158942094,-14.5339683530659,-0.195291666666821));
#29767=CARTESIAN_POINT('Ctrl Pts',(16.6154772628062,-13.5679367061317,-0.236958333333488));
#29768=CARTESIAN_POINT('Ctrl Pts',(15.5,-13.5679367061317,-0.278625000000155));
#29769=CARTESIAN_POINT('Ctrl Pts',(14.3845227371938,-13.5679367061317,-0.320291666666821));
#29770=CARTESIAN_POINT('Ctrl Pts',(13.8267841057906,-14.5339683530659,-0.361958333333488));
#29771=CARTESIAN_POINT('Ctrl Pts',(13.2690454743875,-15.5,-0.403625000000156));
#29772=CARTESIAN_POINT('Ctrl Pts',(13.8267841057906,-16.4660316469341,-0.445291666666823));
#29773=CARTESIAN_POINT('Ctrl Pts',(14.3845227371938,-17.4320632938683,-0.48695833333349));
#29774=CARTESIAN_POINT('Ctrl Pts',(15.5,-17.4320632938683,-0.528625000000157));
#29775=CARTESIAN_POINT('Ctrl Pts',(16.6154772628062,-17.4320632938683,-0.570291666666825));
#29776=CARTESIAN_POINT('Ctrl Pts',(17.1732158942094,-16.4660316469341,-0.611958333333492));
#29777=CARTESIAN_POINT('Ctrl Pts',(17.7309545256125,-15.5,-0.653625000000159));
#29778=CARTESIAN_POINT('Ctrl Pts',(17.1732158942094,-14.5339683530659,-0.695291666666827));
#29779=CARTESIAN_POINT('Ctrl Pts',(16.6154772628062,-13.5679367061317,-0.736958333333494));
#29780=CARTESIAN_POINT('Ctrl Pts',(15.5,-13.5679367061317,-0.778625000000161));
#29781=CARTESIAN_POINT('Ctrl Pts',(14.3845227371938,-13.5679367061317,-0.820291666666829));
#29782=CARTESIAN_POINT('Ctrl Pts',(13.8267841057906,-14.5339683530659,-0.861958333333496));
#29783=CARTESIAN_POINT('Ctrl Pts',(13.2690454743875,-15.5,-0.903625000000163));
#29784=CARTESIAN_POINT('Ctrl Pts',(13.8267841057906,-16.4660316469341,-0.94529166666683));
#29785=CARTESIAN_POINT('Ctrl Pts',(14.3845227371938,-17.4320632938683,-0.986958333333498));
#29786=CARTESIAN_POINT('Ctrl Pts',(15.5,-17.4320632938683,-1.02862500000016));
#29787=CARTESIAN_POINT('Ctrl Pts',(16.6154772628062,-17.4320632938683,-1.07029166666683));
#29788=CARTESIAN_POINT('Ctrl Pts',(17.1732158942094,-16.4660316469341,-1.1119583333335));
#29789=CARTESIAN_POINT('Ctrl Pts',(17.7309545256125,-15.5,-1.15362500000017));
#29790=CARTESIAN_POINT('Ctrl Pts',(17.1732158942094,-14.5339683530659,-1.19529166666683));
#29791=CARTESIAN_POINT('Ctrl Pts',(16.6154772628062,-13.5679367061317,-1.2369583333335));
#29792=CARTESIAN_POINT('Ctrl Pts',(15.5,-13.5679367061317,-1.27862500000017));
#29793=CARTESIAN_POINT('Ctrl Pts',(14.3845227371938,-13.5679367061317,-1.32029166666684));
#29794=CARTESIAN_POINT('Ctrl Pts',(13.8267841057906,-14.5339683530659,-1.3619583333335));
#29795=CARTESIAN_POINT('Ctrl Pts',(13.2690454743875,-15.5,-1.40362500000017));
#29796=CARTESIAN_POINT('Ctrl Pts',(13.8267841057906,-16.4660316469341,-1.44529166666684));
#29797=CARTESIAN_POINT('Ctrl Pts',(14.3845227371938,-17.4320632938683,-1.4869583333335));
#29798=CARTESIAN_POINT('Ctrl Pts',(15.5,-17.4320632938683,-1.52862500000017));
#29799=CARTESIAN_POINT('Ctrl Pts',(16.6154772628062,-17.4320632938683,-1.57029166666684));
#29800=CARTESIAN_POINT('Ctrl Pts',(17.1732158942094,-16.4660316469341,-1.61195833333351));
#29801=CARTESIAN_POINT('Ctrl Pts',(17.7309545256125,-15.5,-1.65362500000017));
#29802=CARTESIAN_POINT('Ctrl Pts',(17.1732158942094,-14.5339683530659,-1.69529166666684));
#29803=CARTESIAN_POINT('Ctrl Pts',(16.6154772628062,-13.5679367061317,-1.73695833333351));
#29804=CARTESIAN_POINT('Ctrl Pts',(15.5,-13.5679367061317,-1.77862500000017));
#29805=CARTESIAN_POINT('Ctrl Pts',(14.3845227371938,-13.5679367061317,-1.82029166666684));
#29806=CARTESIAN_POINT('Ctrl Pts',(13.8267841057906,-14.5339683530659,-1.86195833333351));
#29807=CARTESIAN_POINT('Ctrl Pts',(13.2690454743875,-15.5,-1.90362500000018));
#29808=CARTESIAN_POINT('Ctrl Pts',(13.8267841057906,-16.4660316469341,-1.94529166666684));
#29809=CARTESIAN_POINT('Ctrl Pts',(14.3845227371938,-17.4320632938683,-1.98695833333351));
#29810=CARTESIAN_POINT('Ctrl Pts',(15.5,-17.4320632938683,-2.02862500000018));
#29811=CARTESIAN_POINT('Ctrl Pts',(16.6154772628062,-17.4320632938683,-2.07029166666685));
#29812=CARTESIAN_POINT('Ctrl Pts',(17.1732158942094,-16.4660316469341,-2.11195833333351));
#29813=CARTESIAN_POINT('Ctrl Pts',(17.7309545256125,-15.5,-2.15362500000018));
#29814=CARTESIAN_POINT('Ctrl Pts',(17.1732158942094,-14.5339683530659,-2.19529166666685));
#29815=CARTESIAN_POINT('Ctrl Pts',(16.9678747970191,-14.1783071398504,-2.21063196867905));
#29816=CARTESIAN_POINT('Ctrl Pts',(16.6356236599184,-13.9369173167914,-2.22824840486548));
#29817=CARTESIAN_POINT('',(16.4288320706156,-14.2215513317122,-2.02512305032214));
#29818=CARTESIAN_POINT('Ctrl Pts',(15.2436450846258,-13.9406917842497,10.4122404735808));
#29819=CARTESIAN_POINT('Ctrl Pts',(14.5054990725557,-14.0620451873462,10.3753299573543));
#29820=CARTESIAN_POINT('Ctrl Pts',(14.1314716057906,-14.7098797632096,10.3411666666667));
#29821=CARTESIAN_POINT('Ctrl Pts',(13.6752954743875,-15.5,10.2995));
#29822=CARTESIAN_POINT('Ctrl Pts',(14.1314716057906,-16.2901202367904,10.2578333333333));
#29823=CARTESIAN_POINT('Ctrl Pts',(14.5876477371938,-17.0802404735808,10.2161666666667));
#29824=CARTESIAN_POINT('Ctrl Pts',(15.5,-17.0802404735808,10.1745));
#29825=CARTESIAN_POINT('Ctrl Pts',(16.4123522628062,-17.0802404735808,10.1328333333333));
#29826=CARTESIAN_POINT('Ctrl Pts',(16.8685283942094,-16.2901202367904,10.0911666666667));
#29827=CARTESIAN_POINT('Ctrl Pts',(17.3247045256125,-15.5,10.0495));
#29828=CARTESIAN_POINT('Ctrl Pts',(16.8685283942094,-14.7098797632096,10.0078333333333));
#29829=CARTESIAN_POINT('Ctrl Pts',(16.4123522628062,-13.9197595264192,9.96616666666665));
#29830=CARTESIAN_POINT('Ctrl Pts',(15.5,-13.9197595264192,9.92449999999998));
#29831=CARTESIAN_POINT('Ctrl Pts',(14.5876477371938,-13.9197595264192,9.88283333333331));
#29832=CARTESIAN_POINT('Ctrl Pts',(14.1314716057906,-14.7098797632096,9.84116666666665));
#29833=CARTESIAN_POINT('Ctrl Pts',(13.6752954743875,-15.5,9.79949999999998));
#29834=CARTESIAN_POINT('Ctrl Pts',(14.1314716057906,-16.2901202367904,9.75783333333331));
#29835=CARTESIAN_POINT('Ctrl Pts',(14.5876477371938,-17.0802404735808,9.71616666666665));
#29836=CARTESIAN_POINT('Ctrl Pts',(15.5,-17.0802404735808,9.67449999999998));
#29837=CARTESIAN_POINT('Ctrl Pts',(16.4123522628062,-17.0802404735808,9.63283333333331));
#29838=CARTESIAN_POINT('Ctrl Pts',(16.8685283942094,-16.2901202367904,9.59116666666664));
#29839=CARTESIAN_POINT('Ctrl Pts',(17.3247045256125,-15.5,9.54949999999998));
#29840=CARTESIAN_POINT('Ctrl Pts',(16.8685283942094,-14.7098797632096,9.50783333333331));
#29841=CARTESIAN_POINT('Ctrl Pts',(16.4123522628062,-13.9197595264192,9.46616666666664));
#29842=CARTESIAN_POINT('Ctrl Pts',(15.5,-13.9197595264192,9.42449999999998));
#29843=CARTESIAN_POINT('Ctrl Pts',(14.5876477371938,-13.9197595264192,9.38283333333331));
#29844=CARTESIAN_POINT('Ctrl Pts',(14.1314716057906,-14.7098797632096,9.34116666666664));
#29845=CARTESIAN_POINT('Ctrl Pts',(13.6752954743875,-15.5,9.29949999999997));
#29846=CARTESIAN_POINT('Ctrl Pts',(14.1314716057906,-16.2901202367904,9.25783333333331));
#29847=CARTESIAN_POINT('Ctrl Pts',(14.5876477371938,-17.0802404735808,9.21616666666664));
#29848=CARTESIAN_POINT('Ctrl Pts',(15.5,-17.0802404735808,9.17449999999997));
#29849=CARTESIAN_POINT('Ctrl Pts',(16.4123522628062,-17.0802404735808,9.13283333333331));
#29850=CARTESIAN_POINT('Ctrl Pts',(16.8685283942094,-16.2901202367904,9.09116666666664));
#29851=CARTESIAN_POINT('Ctrl Pts',(17.3247045256125,-15.5,9.04949999999997));
#29852=CARTESIAN_POINT('Ctrl Pts',(16.8685283942094,-14.7098797632096,9.0078333333333));
#29853=CARTESIAN_POINT('Ctrl Pts',(16.4123522628062,-13.9197595264192,8.96616666666664));
#29854=CARTESIAN_POINT('Ctrl Pts',(15.5,-13.9197595264192,8.92449999999997));
#29855=CARTESIAN_POINT('Ctrl Pts',(14.5876477371938,-13.9197595264192,8.8828333333333));
#29856=CARTESIAN_POINT('Ctrl Pts',(14.1314716057906,-14.7098797632096,8.84116666666664));
#29857=CARTESIAN_POINT('Ctrl Pts',(13.6752954743875,-15.5,8.79949999999997));
#29858=CARTESIAN_POINT('Ctrl Pts',(14.1314716057906,-16.2901202367904,8.7578333333333));
#29859=CARTESIAN_POINT('Ctrl Pts',(14.5876477371938,-17.0802404735808,8.71616666666663));
#29860=CARTESIAN_POINT('Ctrl Pts',(15.5,-17.0802404735808,8.67449999999997));
#29861=CARTESIAN_POINT('Ctrl Pts',(16.4123522628062,-17.0802404735808,8.6328333333333));
#29862=CARTESIAN_POINT('Ctrl Pts',(16.8685283942094,-16.2901202367904,8.59116666666663));
#29863=CARTESIAN_POINT('Ctrl Pts',(17.3247045256125,-15.5,8.54949999999996));
#29864=CARTESIAN_POINT('Ctrl Pts',(16.8685283942094,-14.7098797632096,8.50783333333329));
#29865=CARTESIAN_POINT('Ctrl Pts',(16.4123522628062,-13.9197595264192,8.46616666666663));
#29866=CARTESIAN_POINT('Ctrl Pts',(15.5,-13.9197595264192,8.42449999999996));
#29867=CARTESIAN_POINT('Ctrl Pts',(14.5876477371938,-13.9197595264192,8.38283333333329));
#29868=CARTESIAN_POINT('Ctrl Pts',(14.1314716057906,-14.7098797632096,8.34116666666663));
#29869=CARTESIAN_POINT('Ctrl Pts',(13.6752954743875,-15.5,8.29949999999996));
#29870=CARTESIAN_POINT('Ctrl Pts',(14.1314716057906,-16.2901202367904,8.25783333333329));
#29871=CARTESIAN_POINT('Ctrl Pts',(14.5876477371938,-17.0802404735808,8.21616666666663));
#29872=CARTESIAN_POINT('Ctrl Pts',(15.5,-17.0802404735808,8.17449999999996));
#29873=CARTESIAN_POINT('Ctrl Pts',(16.4123522628062,-17.0802404735808,8.13283333333329));
#29874=CARTESIAN_POINT('Ctrl Pts',(16.8685283942094,-16.2901202367904,8.09116666666663));
#29875=CARTESIAN_POINT('Ctrl Pts',(17.3247045256125,-15.5,8.04949999999996));
#29876=CARTESIAN_POINT('Ctrl Pts',(16.8685283942094,-14.7098797632096,8.00783333333329));
#29877=CARTESIAN_POINT('Ctrl Pts',(16.4123522628062,-13.9197595264192,7.96616666666662));
#29878=CARTESIAN_POINT('Ctrl Pts',(15.5,-13.9197595264192,7.92449999999996));
#29879=CARTESIAN_POINT('Ctrl Pts',(14.5876477371938,-13.9197595264192,7.88283333333329));
#29880=CARTESIAN_POINT('Ctrl Pts',(14.1314716057906,-14.7098797632096,7.84116666666662));
#29881=CARTESIAN_POINT('Ctrl Pts',(13.6752954743875,-15.5,7.79949999999995));
#29882=CARTESIAN_POINT('Ctrl Pts',(14.1314716057906,-16.2901202367904,7.75783333333329));
#29883=CARTESIAN_POINT('Ctrl Pts',(14.5876477371938,-17.0802404735808,7.71616666666662));
#29884=CARTESIAN_POINT('Ctrl Pts',(15.5,-17.0802404735808,7.67449999999995));
#29885=CARTESIAN_POINT('Ctrl Pts',(16.4123522628062,-17.0802404735808,7.63283333333328));
#29886=CARTESIAN_POINT('Ctrl Pts',(16.8685283942094,-16.2901202367904,7.59116666666662));
#29887=CARTESIAN_POINT('Ctrl Pts',(17.3247045256125,-15.5,7.54949999999995));
#29888=CARTESIAN_POINT('Ctrl Pts',(16.8685283942094,-14.7098797632096,7.50783333333328));
#29889=CARTESIAN_POINT('Ctrl Pts',(16.4123522628062,-13.9197595264192,7.46616666666662));
#29890=CARTESIAN_POINT('Ctrl Pts',(15.5,-13.9197595264192,7.42449999999995));
#29891=CARTESIAN_POINT('Ctrl Pts',(14.5876477371938,-13.9197595264192,7.38283333333328));
#29892=CARTESIAN_POINT('Ctrl Pts',(14.1314716057906,-14.7098797632096,7.34116666666661));
#29893=CARTESIAN_POINT('Ctrl Pts',(13.6752954743875,-15.5,7.29949999999995));
#29894=CARTESIAN_POINT('Ctrl Pts',(14.1314716057906,-16.2901202367904,7.25783333333328));
#29895=CARTESIAN_POINT('Ctrl Pts',(14.5876477371938,-17.0802404735808,7.21616666666661));
#29896=CARTESIAN_POINT('Ctrl Pts',(15.5,-17.0802404735808,7.17449999999995));
#29897=CARTESIAN_POINT('Ctrl Pts',(16.4123522628062,-17.0802404735808,7.13283333333328));
#29898=CARTESIAN_POINT('Ctrl Pts',(16.8685283942094,-16.2901202367904,7.09116666666661));
#29899=CARTESIAN_POINT('Ctrl Pts',(17.3247045256125,-15.5,7.04949999999994));
#29900=CARTESIAN_POINT('Ctrl Pts',(16.8685283942094,-14.7098797632096,7.00783333333328));
#29901=CARTESIAN_POINT('Ctrl Pts',(16.4123522628062,-13.9197595264192,6.96616666666661));
#29902=CARTESIAN_POINT('Ctrl Pts',(15.5,-13.9197595264192,6.92449999999994));
#29903=CARTESIAN_POINT('Ctrl Pts',(14.5876477371938,-13.9197595264192,6.88283333333327));
#29904=CARTESIAN_POINT('Ctrl Pts',(14.1314716057906,-14.7098797632096,6.84116666666661));
#29905=CARTESIAN_POINT('Ctrl Pts',(13.6752954743875,-15.5,6.79949999999994));
#29906=CARTESIAN_POINT('Ctrl Pts',(14.1314716057906,-16.2901202367904,6.75783333333327));
#29907=CARTESIAN_POINT('Ctrl Pts',(14.5876477371938,-17.0802404735808,6.71616666666661));
#29908=CARTESIAN_POINT('Ctrl Pts',(15.5,-17.0802404735808,6.67449999999994));
#29909=CARTESIAN_POINT('Ctrl Pts',(16.4123522628062,-17.0802404735808,6.63283333333327));
#29910=CARTESIAN_POINT('Ctrl Pts',(16.8685283942094,-16.2901202367904,6.59116666666661));
#29911=CARTESIAN_POINT('Ctrl Pts',(17.3247045256125,-15.5,6.54949999999994));
#29912=CARTESIAN_POINT('Ctrl Pts',(16.8685283942094,-14.7098797632096,6.50783333333327));
#29913=CARTESIAN_POINT('Ctrl Pts',(16.4123522628062,-13.9197595264192,6.4661666666666));
#29914=CARTESIAN_POINT('Ctrl Pts',(15.5,-13.9197595264192,6.42449999999994));
#29915=CARTESIAN_POINT('Ctrl Pts',(14.5876477371938,-13.9197595264192,6.38283333333327));
#29916=CARTESIAN_POINT('Ctrl Pts',(14.1314716057906,-14.7098797632096,6.3411666666666));
#29917=CARTESIAN_POINT('Ctrl Pts',(13.6752954743875,-15.5,6.29949999999993));
#29918=CARTESIAN_POINT('Ctrl Pts',(14.1314716057906,-16.2901202367904,6.25783333333327));
#29919=CARTESIAN_POINT('Ctrl Pts',(14.5876477371938,-17.0802404735808,6.2161666666666));
#29920=CARTESIAN_POINT('Ctrl Pts',(15.5,-17.0802404735808,6.17449999999993));
#29921=CARTESIAN_POINT('Ctrl Pts',(16.4123522628062,-17.0802404735808,6.13283333333326));
#29922=CARTESIAN_POINT('Ctrl Pts',(16.8685283942094,-16.2901202367904,6.0911666666666));
#29923=CARTESIAN_POINT('Ctrl Pts',(17.3247045256125,-15.5,6.04949999999993));
#29924=CARTESIAN_POINT('Ctrl Pts',(16.8685283942094,-14.7098797632096,6.00783333333326));
#29925=CARTESIAN_POINT('Ctrl Pts',(16.4123522628062,-13.9197595264192,5.9661666666666));
#29926=CARTESIAN_POINT('Ctrl Pts',(15.5,-13.9197595264192,5.92449999999993));
#29927=CARTESIAN_POINT('Ctrl Pts',(14.5876477371938,-13.9197595264192,5.88283333333326));
#29928=CARTESIAN_POINT('Ctrl Pts',(14.1314716057906,-14.7098797632096,5.8411666666666));
#29929=CARTESIAN_POINT('Ctrl Pts',(13.6752954743875,-15.5,5.79949999999993));
#29930=CARTESIAN_POINT('Ctrl Pts',(14.1314716057906,-16.2901202367904,5.75783333333326));
#29931=CARTESIAN_POINT('Ctrl Pts',(14.5876477371938,-17.0802404735808,5.71616666666659));
#29932=CARTESIAN_POINT('Ctrl Pts',(15.5,-17.0802404735808,5.67449999999993));
#29933=CARTESIAN_POINT('Ctrl Pts',(16.4123522628062,-17.0802404735808,5.63283333333326));
#29934=CARTESIAN_POINT('Ctrl Pts',(16.8685283942094,-16.2901202367904,5.59116666666659));
#29935=CARTESIAN_POINT('Ctrl Pts',(17.3247045256125,-15.5,5.54949999999992));
#29936=CARTESIAN_POINT('Ctrl Pts',(16.8685283942094,-14.7098797632096,5.50783333333326));
#29937=CARTESIAN_POINT('Ctrl Pts',(16.4123522628062,-13.9197595264192,5.46616666666659));
#29938=CARTESIAN_POINT('Ctrl Pts',(15.5,-13.9197595264192,5.42449999999992));
#29939=CARTESIAN_POINT('Ctrl Pts',(14.5876477371938,-13.9197595264192,5.38283333333326));
#29940=CARTESIAN_POINT('Ctrl Pts',(14.1314716057906,-14.7098797632096,5.34116666666659));
#29941=CARTESIAN_POINT('Ctrl Pts',(13.6752954743875,-15.5,5.29949999999992));
#29942=CARTESIAN_POINT('Ctrl Pts',(14.1314716057906,-16.2901202367904,5.25783333333325));
#29943=CARTESIAN_POINT('Ctrl Pts',(14.5876477371938,-17.0802404735808,5.21616666666659));
#29944=CARTESIAN_POINT('Ctrl Pts',(15.5,-17.0802404735808,5.17449999999992));
#29945=CARTESIAN_POINT('Ctrl Pts',(16.4123522628062,-17.0802404735808,5.13283333333325));
#29946=CARTESIAN_POINT('Ctrl Pts',(16.8685283942094,-16.2901202367904,5.09116666666658));
#29947=CARTESIAN_POINT('Ctrl Pts',(17.3247045256125,-15.5,5.04949999999992));
#29948=CARTESIAN_POINT('Ctrl Pts',(16.8685283942094,-14.7098797632096,5.00783333333325));
#29949=CARTESIAN_POINT('Ctrl Pts',(16.4123522628062,-13.9197595264192,4.96616666666658));
#29950=CARTESIAN_POINT('Ctrl Pts',(15.5,-13.9197595264192,4.92449999999992));
#29951=CARTESIAN_POINT('Ctrl Pts',(14.5876477371938,-13.9197595264192,4.88283333333325));
#29952=CARTESIAN_POINT('Ctrl Pts',(14.1314716057906,-14.7098797632096,4.84116666666658));
#29953=CARTESIAN_POINT('Ctrl Pts',(13.6752954743875,-15.5,4.79949999999991));
#29954=CARTESIAN_POINT('Ctrl Pts',(14.1314716057906,-16.2901202367904,4.75783333333325));
#29955=CARTESIAN_POINT('Ctrl Pts',(14.5876477371938,-17.0802404735808,4.71616666666658));
#29956=CARTESIAN_POINT('Ctrl Pts',(15.5,-17.0802404735808,4.67449999999991));
#29957=CARTESIAN_POINT('Ctrl Pts',(16.4123522628062,-17.0802404735808,4.63283333333325));
#29958=CARTESIAN_POINT('Ctrl Pts',(16.8685283942094,-16.2901202367904,4.59116666666658));
#29959=CARTESIAN_POINT('Ctrl Pts',(17.3247045256125,-15.5,4.54949999999991));
#29960=CARTESIAN_POINT('Ctrl Pts',(16.8685283942094,-14.7098797632096,4.50783333333324));
#29961=CARTESIAN_POINT('Ctrl Pts',(16.4123522628062,-13.9197595264192,4.46616666666658));
#29962=CARTESIAN_POINT('Ctrl Pts',(15.5,-13.9197595264192,4.42449999999991));
#29963=CARTESIAN_POINT('Ctrl Pts',(14.5876477371938,-13.9197595264192,4.38283333333324));
#29964=CARTESIAN_POINT('Ctrl Pts',(14.1314716057906,-14.7098797632096,4.34116666666657));
#29965=CARTESIAN_POINT('Ctrl Pts',(13.6752954743875,-15.5,4.29949999999991));
#29966=CARTESIAN_POINT('Ctrl Pts',(14.1314716057906,-16.2901202367904,4.25783333333324));
#29967=CARTESIAN_POINT('Ctrl Pts',(14.5876477371938,-17.0802404735808,4.21616666666657));
#29968=CARTESIAN_POINT('Ctrl Pts',(15.5,-17.0802404735808,4.17449999999991));
#29969=CARTESIAN_POINT('Ctrl Pts',(16.4123522628062,-17.0802404735808,4.13283333333324));
#29970=CARTESIAN_POINT('Ctrl Pts',(16.8685283942094,-16.2901202367904,4.09116666666657));
#29971=CARTESIAN_POINT('Ctrl Pts',(17.3247045256125,-15.5,4.0494999999999));
#29972=CARTESIAN_POINT('Ctrl Pts',(16.8685283942094,-14.7098797632096,4.00783333333324));
#29973=CARTESIAN_POINT('Ctrl Pts',(16.4123522628062,-13.9197595264192,3.96616666666657));
#29974=CARTESIAN_POINT('Ctrl Pts',(15.5,-13.9197595264192,3.9244999999999));
#29975=CARTESIAN_POINT('Ctrl Pts',(14.5876477371938,-13.9197595264192,3.88283333333323));
#29976=CARTESIAN_POINT('Ctrl Pts',(14.1314716057906,-14.7098797632096,3.84116666666657));
#29977=CARTESIAN_POINT('Ctrl Pts',(13.6752954743875,-15.5,3.7994999999999));
#29978=CARTESIAN_POINT('Ctrl Pts',(14.1314716057906,-16.2901202367904,3.75783333333323));
#29979=CARTESIAN_POINT('Ctrl Pts',(14.5876477371938,-17.0802404735808,3.71616666666657));
#29980=CARTESIAN_POINT('Ctrl Pts',(15.5,-17.0802404735808,3.6744999999999));
#29981=CARTESIAN_POINT('Ctrl Pts',(16.4123522628062,-17.0802404735808,3.63283333333323));
#29982=CARTESIAN_POINT('Ctrl Pts',(16.8685283942094,-16.2901202367904,3.59116666666656));
#29983=CARTESIAN_POINT('Ctrl Pts',(17.3247045256125,-15.5,3.5494999999999));
#29984=CARTESIAN_POINT('Ctrl Pts',(16.8685283942094,-14.7098797632096,3.50783333333323));
#29985=CARTESIAN_POINT('Ctrl Pts',(16.4123522628062,-13.9197595264192,3.46616666666656));
#29986=CARTESIAN_POINT('Ctrl Pts',(15.5,-13.9197595264192,3.4244999999999));
#29987=CARTESIAN_POINT('Ctrl Pts',(14.5876477371938,-13.9197595264192,3.38283333333323));
#29988=CARTESIAN_POINT('Ctrl Pts',(14.1314716057906,-14.7098797632096,3.34116666666656));
#29989=CARTESIAN_POINT('Ctrl Pts',(13.6752954743875,-15.5,3.29949999999989));
#29990=CARTESIAN_POINT('Ctrl Pts',(14.1314716057906,-16.2901202367904,3.25783333333323));
#29991=CARTESIAN_POINT('Ctrl Pts',(14.5876477371938,-17.0802404735808,3.21616666666656));
#29992=CARTESIAN_POINT('Ctrl Pts',(15.5,-17.0802404735808,3.17449999999989));
#29993=CARTESIAN_POINT('Ctrl Pts',(16.4123522628062,-17.0802404735808,3.13283333333323));
#29994=CARTESIAN_POINT('Ctrl Pts',(16.8685283942094,-16.2901202367904,3.09116666666656));
#29995=CARTESIAN_POINT('Ctrl Pts',(17.3247045256125,-15.5,3.04949999999989));
#29996=CARTESIAN_POINT('Ctrl Pts',(16.8685283942094,-14.7098797632096,3.00783333333322));
#29997=CARTESIAN_POINT('Ctrl Pts',(16.4123522628062,-13.9197595264192,2.96616666666656));
#29998=CARTESIAN_POINT('Ctrl Pts',(15.5,-13.9197595264192,2.92449999999989));
#29999=CARTESIAN_POINT('Ctrl Pts',(14.5876477371938,-13.9197595264192,2.88283333333322));
#30000=CARTESIAN_POINT('Ctrl Pts',(14.1314716057906,-14.7098797632096,2.84116666666655));
#30001=CARTESIAN_POINT('Ctrl Pts',(13.6752954743875,-15.5,2.79949999999989));
#30002=CARTESIAN_POINT('Ctrl Pts',(14.1314716057906,-16.2901202367904,2.75783333333322));
#30003=CARTESIAN_POINT('Ctrl Pts',(14.5876477371938,-17.0802404735808,2.71616666666655));
#30004=CARTESIAN_POINT('Ctrl Pts',(15.5,-17.0802404735808,2.67449999999989));
#30005=CARTESIAN_POINT('Ctrl Pts',(16.4123522628062,-17.0802404735808,2.63283333333322));
#30006=CARTESIAN_POINT('Ctrl Pts',(16.8685283942094,-16.2901202367904,2.59116666666655));
#30007=CARTESIAN_POINT('Ctrl Pts',(17.3247045256125,-15.5,2.54949999999988));
#30008=CARTESIAN_POINT('Ctrl Pts',(16.8685283942094,-14.7098797632096,2.50783333333322));
#30009=CARTESIAN_POINT('Ctrl Pts',(16.4123522628062,-13.9197595264192,2.46616666666655));
#30010=CARTESIAN_POINT('Ctrl Pts',(15.5,-13.9197595264192,2.42449999999988));
#30011=CARTESIAN_POINT('Ctrl Pts',(14.5876477371938,-13.9197595264192,2.38283333333321));
#30012=CARTESIAN_POINT('Ctrl Pts',(14.1314716057906,-14.7098797632096,2.34116666666655));
#30013=CARTESIAN_POINT('Ctrl Pts',(13.6752954743875,-15.5,2.29949999999988));
#30014=CARTESIAN_POINT('Ctrl Pts',(14.1314716057906,-16.2901202367904,2.25783333333321));
#30015=CARTESIAN_POINT('Ctrl Pts',(14.5876477371938,-17.0802404735808,2.21616666666655));
#30016=CARTESIAN_POINT('Ctrl Pts',(15.5,-17.0802404735808,2.17449999999988));
#30017=CARTESIAN_POINT('Ctrl Pts',(16.4123522628062,-17.0802404735808,2.13283333333321));
#30018=CARTESIAN_POINT('Ctrl Pts',(16.8685283942094,-16.2901202367904,2.09116666666655));
#30019=CARTESIAN_POINT('Ctrl Pts',(17.3247045256125,-15.5,2.04949999999988));
#30020=CARTESIAN_POINT('Ctrl Pts',(16.8685283942094,-14.7098797632096,2.00783333333321));
#30021=CARTESIAN_POINT('Ctrl Pts',(16.4123522628062,-13.9197595264192,1.96616666666654));
#30022=CARTESIAN_POINT('Ctrl Pts',(15.5,-13.9197595264192,1.92449999999988));
#30023=CARTESIAN_POINT('Ctrl Pts',(14.5876477371938,-13.9197595264192,1.88283333333321));
#30024=CARTESIAN_POINT('Ctrl Pts',(14.1314716057906,-14.7098797632096,1.84116666666654));
#30025=CARTESIAN_POINT('Ctrl Pts',(13.6752954743875,-15.5,1.79949999999987));
#30026=CARTESIAN_POINT('Ctrl Pts',(14.1314716057906,-16.2901202367904,1.75783333333321));
#30027=CARTESIAN_POINT('Ctrl Pts',(14.5876477371938,-17.0802404735808,1.71616666666654));
#30028=CARTESIAN_POINT('Ctrl Pts',(15.5,-17.0802404735808,1.67449999999987));
#30029=CARTESIAN_POINT('Ctrl Pts',(16.4123522628062,-17.0802404735808,1.63283333333321));
#30030=CARTESIAN_POINT('Ctrl Pts',(16.8685283942094,-16.2901202367904,1.59116666666654));
#30031=CARTESIAN_POINT('Ctrl Pts',(17.3247045256125,-15.5,1.54949999999987));
#30032=CARTESIAN_POINT('Ctrl Pts',(16.8685283942094,-14.7098797632096,1.5078333333332));
#30033=CARTESIAN_POINT('Ctrl Pts',(16.4123522628062,-13.9197595264192,1.46616666666654));
#30034=CARTESIAN_POINT('Ctrl Pts',(15.5,-13.9197595264192,1.42449999999987));
#30035=CARTESIAN_POINT('Ctrl Pts',(14.5876477371938,-13.9197595264192,1.3828333333332));
#30036=CARTESIAN_POINT('Ctrl Pts',(14.1314716057906,-14.7098797632096,1.34116666666653));
#30037=CARTESIAN_POINT('Ctrl Pts',(13.6752954743875,-15.5,1.29949999999987));
#30038=CARTESIAN_POINT('Ctrl Pts',(14.1314716057906,-16.2901202367904,1.2578333333332));
#30039=CARTESIAN_POINT('Ctrl Pts',(14.5876477371938,-17.0802404735808,1.21616666666653));
#30040=CARTESIAN_POINT('Ctrl Pts',(15.5,-17.0802404735808,1.17449999999986));
#30041=CARTESIAN_POINT('Ctrl Pts',(16.4123522628062,-17.0802404735808,1.1328333333332));
#30042=CARTESIAN_POINT('Ctrl Pts',(16.8685283942094,-16.2901202367904,1.09116666666653));
#30043=CARTESIAN_POINT('Ctrl Pts',(17.3247045256125,-15.5,1.04949999999987));
#30044=CARTESIAN_POINT('Ctrl Pts',(16.8685283942094,-14.7098797632096,1.0078333333332));
#30045=CARTESIAN_POINT('Ctrl Pts',(16.4123522628062,-13.9197595264192,0.96616666666653));
#30046=CARTESIAN_POINT('Ctrl Pts',(15.5,-13.9197595264192,0.924499999999863));
#30047=CARTESIAN_POINT('Ctrl Pts',(14.5876477371938,-13.9197595264192,0.882833333333196));
#30048=CARTESIAN_POINT('Ctrl Pts',(14.1314716057906,-14.7098797632096,0.841166666666529));
#30049=CARTESIAN_POINT('Ctrl Pts',(13.6752954743875,-15.5,0.799499999999861));
#30050=CARTESIAN_POINT('Ctrl Pts',(14.1314716057906,-16.2901202367904,0.757833333333194));
#30051=CARTESIAN_POINT('Ctrl Pts',(14.5876477371938,-17.0802404735808,0.716166666666527));
#30052=CARTESIAN_POINT('Ctrl Pts',(15.5,-17.0802404735808,0.674499999999859));
#30053=CARTESIAN_POINT('Ctrl Pts',(16.4123522628062,-17.0802404735808,0.632833333333192));
#30054=CARTESIAN_POINT('Ctrl Pts',(16.8685283942094,-16.2901202367904,0.591166666666525));
#30055=CARTESIAN_POINT('Ctrl Pts',(17.3247045256125,-15.5,0.549499999999857));
#30056=CARTESIAN_POINT('Ctrl Pts',(16.8685283942094,-14.7098797632096,0.50783333333319));
#30057=CARTESIAN_POINT('Ctrl Pts',(16.4123522628062,-13.9197595264192,0.466166666666523));
#30058=CARTESIAN_POINT('Ctrl Pts',(15.5,-13.9197595264192,0.424499999999856));
#30059=CARTESIAN_POINT('Ctrl Pts',(14.5876477371938,-13.9197595264192,0.382833333333188));
#30060=CARTESIAN_POINT('Ctrl Pts',(14.1314716057906,-14.7098797632096,0.341166666666521));
#30061=CARTESIAN_POINT('Ctrl Pts',(13.6752954743875,-15.5,0.299499999999854));
#30062=CARTESIAN_POINT('Ctrl Pts',(14.1314716057906,-16.2901202367904,0.257833333333186));
#30063=CARTESIAN_POINT('Ctrl Pts',(14.5876477371938,-17.0802404735808,0.216166666666519));
#30064=CARTESIAN_POINT('Ctrl Pts',(15.5,-17.0802404735808,0.174499999999852));
#30065=CARTESIAN_POINT('Ctrl Pts',(16.4123522628062,-17.0802404735808,0.132833333333185));
#30066=CARTESIAN_POINT('Ctrl Pts',(16.8685283942094,-16.2901202367904,0.0911666666665173));
#30067=CARTESIAN_POINT('Ctrl Pts',(17.3247045256125,-15.5,0.04949999999985));
#30068=CARTESIAN_POINT('Ctrl Pts',(16.8685283942094,-14.7098797632096,0.00783333333318273));
#30069=CARTESIAN_POINT('Ctrl Pts',(16.4123522628062,-13.9197595264192,-0.0338333333334846));
#30070=CARTESIAN_POINT('Ctrl Pts',(15.5,-13.9197595264192,-0.0755000000001518));
#30071=CARTESIAN_POINT('Ctrl Pts',(14.5876477371938,-13.9197595264192,-0.117166666666817));
#30072=CARTESIAN_POINT('Ctrl Pts',(14.1314716057906,-14.7098797632096,-0.158833333333485));
#30073=CARTESIAN_POINT('Ctrl Pts',(13.6752954743875,-15.5,-0.200500000000152));
#30074=CARTESIAN_POINT('Ctrl Pts',(14.1314716057906,-16.2901202367904,-0.242166666666819));
#30075=CARTESIAN_POINT('Ctrl Pts',(14.5876477371938,-17.0802404735808,-0.283833333333487));
#30076=CARTESIAN_POINT('Ctrl Pts',(15.5,-17.0802404735808,-0.325500000000154));
#30077=CARTESIAN_POINT('Ctrl Pts',(16.4123522628062,-17.0802404735808,-0.367166666666821));
#30078=CARTESIAN_POINT('Ctrl Pts',(16.8685283942094,-16.2901202367904,-0.408833333333488));
#30079=CARTESIAN_POINT('Ctrl Pts',(17.3247045256125,-15.5,-0.450500000000156));
#30080=CARTESIAN_POINT('Ctrl Pts',(16.8685283942094,-14.7098797632096,-0.492166666666823));
#30081=CARTESIAN_POINT('Ctrl Pts',(16.4123522628062,-13.9197595264192,-0.53383333333349));
#30082=CARTESIAN_POINT('Ctrl Pts',(15.5,-13.9197595264192,-0.575500000000157));
#30083=CARTESIAN_POINT('Ctrl Pts',(14.5876477371938,-13.9197595264192,-0.617166666666825));
#30084=CARTESIAN_POINT('Ctrl Pts',(14.1314716057906,-14.7098797632096,-0.658833333333492));
#30085=CARTESIAN_POINT('Ctrl Pts',(13.6752954743875,-15.5,-0.700500000000159));
#30086=CARTESIAN_POINT('Ctrl Pts',(14.1314716057906,-16.2901202367904,-0.742166666666827));
#30087=CARTESIAN_POINT('Ctrl Pts',(14.5876477371938,-17.0802404735808,-0.783833333333494));
#30088=CARTESIAN_POINT('Ctrl Pts',(15.5,-17.0802404735808,-0.825500000000161));
#30089=CARTESIAN_POINT('Ctrl Pts',(16.4123522628062,-17.0802404735808,-0.867166666666829));
#30090=CARTESIAN_POINT('Ctrl Pts',(16.8685283942094,-16.2901202367904,-0.908833333333496));
#30091=CARTESIAN_POINT('Ctrl Pts',(17.3247045256125,-15.5,-0.950500000000163));
#30092=CARTESIAN_POINT('Ctrl Pts',(16.8685283942094,-14.7098797632096,-0.99216666666683));
#30093=CARTESIAN_POINT('Ctrl Pts',(16.4123522628062,-13.9197595264192,-1.0338333333335));
#30094=CARTESIAN_POINT('Ctrl Pts',(15.5,-13.9197595264192,-1.07550000000016));
#30095=CARTESIAN_POINT('Ctrl Pts',(14.5876477371938,-13.9197595264192,-1.11716666666683));
#30096=CARTESIAN_POINT('Ctrl Pts',(14.1314716057906,-14.7098797632096,-1.1588333333335));
#30097=CARTESIAN_POINT('Ctrl Pts',(13.6752954743875,-15.5,-1.20050000000017));
#30098=CARTESIAN_POINT('Ctrl Pts',(14.1314716057906,-16.2901202367904,-1.24216666666683));
#30099=CARTESIAN_POINT('Ctrl Pts',(14.5876477371938,-17.0802404735808,-1.2838333333335));
#30100=CARTESIAN_POINT('Ctrl Pts',(15.5,-17.0802404735808,-1.32550000000017));
#30101=CARTESIAN_POINT('Ctrl Pts',(16.4123522628062,-17.0802404735808,-1.36716666666683));
#30102=CARTESIAN_POINT('Ctrl Pts',(16.8685283942094,-16.2901202367904,-1.4088333333335));
#30103=CARTESIAN_POINT('Ctrl Pts',(17.3247045256125,-15.5,-1.45050000000017));
#30104=CARTESIAN_POINT('Ctrl Pts',(16.8685283942094,-14.7098797632096,-1.49216666666684));
#30105=CARTESIAN_POINT('Ctrl Pts',(16.4123522628062,-13.9197595264192,-1.5338333333335));
#30106=CARTESIAN_POINT('Ctrl Pts',(15.5,-13.9197595264192,-1.57550000000017));
#30107=CARTESIAN_POINT('Ctrl Pts',(14.5876477371938,-13.9197595264192,-1.61716666666684));
#30108=CARTESIAN_POINT('Ctrl Pts',(14.1314716057906,-14.7098797632096,-1.65883333333351));
#30109=CARTESIAN_POINT('Ctrl Pts',(13.6752954743875,-15.5,-1.70050000000017));
#30110=CARTESIAN_POINT('Ctrl Pts',(14.1314716057906,-16.2901202367904,-1.74216666666684));
#30111=CARTESIAN_POINT('Ctrl Pts',(14.5876477371938,-17.0802404735808,-1.78383333333351));
#30112=CARTESIAN_POINT('Ctrl Pts',(15.5,-17.0802404735808,-1.82550000000017));
#30113=CARTESIAN_POINT('Ctrl Pts',(16.4123522628062,-17.0802404735808,-1.86716666666684));
#30114=CARTESIAN_POINT('Ctrl Pts',(16.8685283942094,-16.2901202367904,-1.90883333333351));
#30115=CARTESIAN_POINT('Ctrl Pts',(17.3247045256125,-15.5,-1.95050000000018));
#30116=CARTESIAN_POINT('Ctrl Pts',(16.8685283942094,-14.7098797632096,-1.99216666666684));
#30117=CARTESIAN_POINT('Ctrl Pts',(16.7005831533691,-14.4189900731849,-2.00750661517932));
#30118=CARTESIAN_POINT('Ctrl Pts',(16.4288360540161,-14.2215542486879,-2.02512301646327));
#30119=CARTESIAN_POINT('',(16.6356236599184,-13.9369173167914,-2.22824840486548));
#30120=CARTESIAN_POINT('Ctrl Pts',(15.5,-17.4320632938683,11.440125));
#30121=CARTESIAN_POINT('Ctrl Pts',(16.6154772628062,-17.4320632938683,11.3984583333333));
#30122=CARTESIAN_POINT('Ctrl Pts',(17.1732158942094,-16.4660316469341,11.3567916666667));
#30123=CARTESIAN_POINT('Ctrl Pts',(17.7309545256125,-15.5,11.315125));
#30124=CARTESIAN_POINT('Ctrl Pts',(17.1732158942094,-14.5339683530659,11.2734583333333));
#30125=CARTESIAN_POINT('Ctrl Pts',(16.6154772628062,-13.5679367061317,11.2317916666667));
#30126=CARTESIAN_POINT('Ctrl Pts',(15.5,-13.5679367061317,11.190125));
#30127=CARTESIAN_POINT('Ctrl Pts',(14.3845227371938,-13.5679367061317,11.1484583333333));
#30128=CARTESIAN_POINT('Ctrl Pts',(13.8267841057906,-14.5339683530659,11.1067916666667));
#30129=CARTESIAN_POINT('Ctrl Pts',(13.2690454743875,-15.5,11.065125));
#30130=CARTESIAN_POINT('Ctrl Pts',(13.8267841057906,-16.4660316469341,11.0234583333333));
#30131=CARTESIAN_POINT('Ctrl Pts',(14.3845227371938,-17.4320632938683,10.9817916666667));
#30132=CARTESIAN_POINT('Ctrl Pts',(15.5,-17.4320632938683,10.940125));
#30133=CARTESIAN_POINT('Ctrl Pts',(16.6154772628062,-17.4320632938683,10.8984583333333));
#30134=CARTESIAN_POINT('Ctrl Pts',(17.1732158942094,-16.4660316469341,10.8567916666667));
#30135=CARTESIAN_POINT('Ctrl Pts',(17.7309545256125,-15.5,10.815125));
#30136=CARTESIAN_POINT('Ctrl Pts',(17.1732158942094,-14.5339683530659,10.7734583333333));
#30137=CARTESIAN_POINT('Ctrl Pts',(16.6154772628062,-13.5679367061317,10.7317916666667));
#30138=CARTESIAN_POINT('Ctrl Pts',(15.5,-13.5679367061317,10.690125));
#30139=CARTESIAN_POINT('Ctrl Pts',(14.3845227371938,-13.5679367061317,10.6484583333333));
#30140=CARTESIAN_POINT('Ctrl Pts',(13.8267841057906,-14.5339683530659,10.6067916666667));
#30141=CARTESIAN_POINT('Ctrl Pts',(13.2690454743875,-15.5,10.565125));
#30142=CARTESIAN_POINT('Ctrl Pts',(13.8267841057906,-16.4660316469341,10.5234583333333));
#30143=CARTESIAN_POINT('Ctrl Pts',(14.3845227371938,-17.4320632938683,10.4817916666667));
#30144=CARTESIAN_POINT('Ctrl Pts',(15.5,-17.4320632938683,10.440125));
#30145=CARTESIAN_POINT('Ctrl Pts',(16.6154772628062,-17.4320632938683,10.3984583333333));
#30146=CARTESIAN_POINT('Ctrl Pts',(17.1732158942094,-16.4660316469341,10.3567916666667));
#30147=CARTESIAN_POINT('Ctrl Pts',(17.7309545256125,-15.5,10.315125));
#30148=CARTESIAN_POINT('Ctrl Pts',(17.1732158942094,-14.5339683530659,10.2734583333333));
#30149=CARTESIAN_POINT('Ctrl Pts',(16.6154772628062,-13.5679367061317,10.2317916666667));
#30150=CARTESIAN_POINT('Ctrl Pts',(15.5,-13.5679367061317,10.190125));
#30151=CARTESIAN_POINT('Ctrl Pts',(14.3845227371938,-13.5679367061317,10.1484583333333));
#30152=CARTESIAN_POINT('Ctrl Pts',(13.8267841057906,-14.5339683530659,10.1067916666666));
#30153=CARTESIAN_POINT('Ctrl Pts',(13.2690454743875,-15.5,10.065125));
#30154=CARTESIAN_POINT('Ctrl Pts',(13.8267841057906,-16.4660316469341,10.0234583333333));
#30155=CARTESIAN_POINT('Ctrl Pts',(14.3845227371938,-17.4320632938683,9.98179166666664));
#30156=CARTESIAN_POINT('Ctrl Pts',(15.5,-17.4320632938683,9.94012499999998));
#30157=CARTESIAN_POINT('Ctrl Pts',(16.6154772628062,-17.4320632938683,9.89845833333331));
#30158=CARTESIAN_POINT('Ctrl Pts',(17.1732158942094,-16.4660316469341,9.85679166666664));
#30159=CARTESIAN_POINT('Ctrl Pts',(17.7309545256125,-15.5,9.81512499999998));
#30160=CARTESIAN_POINT('Ctrl Pts',(17.1732158942094,-14.5339683530659,9.77345833333331));
#30161=CARTESIAN_POINT('Ctrl Pts',(16.6154772628062,-13.5679367061317,9.73179166666664));
#30162=CARTESIAN_POINT('Ctrl Pts',(15.5,-13.5679367061317,9.69012499999998));
#30163=CARTESIAN_POINT('Ctrl Pts',(14.3845227371938,-13.5679367061317,9.64845833333331));
#30164=CARTESIAN_POINT('Ctrl Pts',(13.8267841057906,-14.5339683530659,9.60679166666664));
#30165=CARTESIAN_POINT('Ctrl Pts',(13.2690454743875,-15.5,9.56512499999998));
#30166=CARTESIAN_POINT('Ctrl Pts',(13.8267841057906,-16.4660316469341,9.52345833333331));
#30167=CARTESIAN_POINT('Ctrl Pts',(14.3845227371938,-17.4320632938683,9.48179166666664));
#30168=CARTESIAN_POINT('Ctrl Pts',(15.5,-17.4320632938683,9.44012499999997));
#30169=CARTESIAN_POINT('Ctrl Pts',(16.6154772628062,-17.4320632938683,9.39845833333331));
#30170=CARTESIAN_POINT('Ctrl Pts',(17.1732158942094,-16.4660316469341,9.35679166666664));
#30171=CARTESIAN_POINT('Ctrl Pts',(17.7309545256125,-15.5,9.31512499999997));
#30172=CARTESIAN_POINT('Ctrl Pts',(17.1732158942094,-14.5339683530659,9.2734583333333));
#30173=CARTESIAN_POINT('Ctrl Pts',(16.6154772628062,-13.5679367061317,9.23179166666664));
#30174=CARTESIAN_POINT('Ctrl Pts',(15.5,-13.5679367061317,9.19012499999997));
#30175=CARTESIAN_POINT('Ctrl Pts',(14.3845227371938,-13.5679367061317,9.1484583333333));
#30176=CARTESIAN_POINT('Ctrl Pts',(13.8267841057906,-14.5339683530659,9.10679166666664));
#30177=CARTESIAN_POINT('Ctrl Pts',(13.2690454743875,-15.5,9.06512499999997));
#30178=CARTESIAN_POINT('Ctrl Pts',(13.8267841057906,-16.4660316469341,9.0234583333333));
#30179=CARTESIAN_POINT('Ctrl Pts',(14.3845227371938,-17.4320632938683,8.98179166666663));
#30180=CARTESIAN_POINT('Ctrl Pts',(15.5,-17.4320632938683,8.94012499999997));
#30181=CARTESIAN_POINT('Ctrl Pts',(16.6154772628062,-17.4320632938683,8.8984583333333));
#30182=CARTESIAN_POINT('Ctrl Pts',(17.1732158942094,-16.4660316469341,8.85679166666663));
#30183=CARTESIAN_POINT('Ctrl Pts',(17.7309545256125,-15.5,8.81512499999996));
#30184=CARTESIAN_POINT('Ctrl Pts',(17.1732158942094,-14.5339683530659,8.7734583333333));
#30185=CARTESIAN_POINT('Ctrl Pts',(16.6154772628062,-13.5679367061317,8.73179166666663));
#30186=CARTESIAN_POINT('Ctrl Pts',(15.5,-13.5679367061317,8.69012499999996));
#30187=CARTESIAN_POINT('Ctrl Pts',(14.3845227371938,-13.5679367061317,8.64845833333329));
#30188=CARTESIAN_POINT('Ctrl Pts',(13.8267841057906,-14.5339683530659,8.60679166666663));
#30189=CARTESIAN_POINT('Ctrl Pts',(13.2690454743875,-15.5,8.56512499999996));
#30190=CARTESIAN_POINT('Ctrl Pts',(13.8267841057906,-16.4660316469341,8.52345833333329));
#30191=CARTESIAN_POINT('Ctrl Pts',(14.3845227371938,-17.4320632938683,8.48179166666663));
#30192=CARTESIAN_POINT('Ctrl Pts',(15.5,-17.4320632938683,8.44012499999996));
#30193=CARTESIAN_POINT('Ctrl Pts',(16.6154772628062,-17.4320632938683,8.39845833333329));
#30194=CARTESIAN_POINT('Ctrl Pts',(17.1732158942094,-16.4660316469341,8.35679166666662));
#30195=CARTESIAN_POINT('Ctrl Pts',(17.7309545256125,-15.5,8.31512499999996));
#30196=CARTESIAN_POINT('Ctrl Pts',(17.1732158942094,-14.5339683530659,8.27345833333329));
#30197=CARTESIAN_POINT('Ctrl Pts',(16.6154772628062,-13.5679367061317,8.23179166666662));
#30198=CARTESIAN_POINT('Ctrl Pts',(15.5,-13.5679367061317,8.19012499999996));
#30199=CARTESIAN_POINT('Ctrl Pts',(14.3845227371938,-13.5679367061317,8.14845833333329));
#30200=CARTESIAN_POINT('Ctrl Pts',(13.8267841057906,-14.5339683530659,8.10679166666662));
#30201=CARTESIAN_POINT('Ctrl Pts',(13.2690454743875,-15.5,8.06512499999995));
#30202=CARTESIAN_POINT('Ctrl Pts',(13.8267841057906,-16.4660316469341,8.02345833333329));
#30203=CARTESIAN_POINT('Ctrl Pts',(14.3845227371938,-17.4320632938683,7.98179166666662));
#30204=CARTESIAN_POINT('Ctrl Pts',(15.5,-17.4320632938683,7.94012499999995));
#30205=CARTESIAN_POINT('Ctrl Pts',(16.6154772628062,-17.4320632938683,7.89845833333329));
#30206=CARTESIAN_POINT('Ctrl Pts',(17.1732158942094,-16.4660316469341,7.85679166666662));
#30207=CARTESIAN_POINT('Ctrl Pts',(17.7309545256125,-15.5,7.81512499999995));
#30208=CARTESIAN_POINT('Ctrl Pts',(17.1732158942094,-14.5339683530659,7.77345833333328));
#30209=CARTESIAN_POINT('Ctrl Pts',(16.6154772628062,-13.5679367061317,7.73179166666662));
#30210=CARTESIAN_POINT('Ctrl Pts',(15.5,-13.5679367061317,7.69012499999995));
#30211=CARTESIAN_POINT('Ctrl Pts',(14.3845227371938,-13.5679367061317,7.64845833333328));
#30212=CARTESIAN_POINT('Ctrl Pts',(13.8267841057906,-14.5339683530659,7.60679166666661));
#30213=CARTESIAN_POINT('Ctrl Pts',(13.2690454743875,-15.5,7.56512499999995));
#30214=CARTESIAN_POINT('Ctrl Pts',(13.8267841057906,-16.4660316469341,7.52345833333328));
#30215=CARTESIAN_POINT('Ctrl Pts',(14.3845227371938,-17.4320632938683,7.48179166666661));
#30216=CARTESIAN_POINT('Ctrl Pts',(15.5,-17.4320632938683,7.44012499999995));
#30217=CARTESIAN_POINT('Ctrl Pts',(16.6154772628062,-17.4320632938683,7.39845833333328));
#30218=CARTESIAN_POINT('Ctrl Pts',(17.1732158942094,-16.4660316469341,7.35679166666661));
#30219=CARTESIAN_POINT('Ctrl Pts',(17.7309545256125,-15.5,7.31512499999995));
#30220=CARTESIAN_POINT('Ctrl Pts',(17.1732158942094,-14.5339683530659,7.27345833333328));
#30221=CARTESIAN_POINT('Ctrl Pts',(16.6154772628062,-13.5679367061317,7.23179166666661));
#30222=CARTESIAN_POINT('Ctrl Pts',(15.5,-13.5679367061317,7.19012499999994));
#30223=CARTESIAN_POINT('Ctrl Pts',(14.3845227371938,-13.5679367061317,7.14845833333328));
#30224=CARTESIAN_POINT('Ctrl Pts',(13.8267841057906,-14.5339683530659,7.10679166666661));
#30225=CARTESIAN_POINT('Ctrl Pts',(13.2690454743875,-15.5,7.06512499999994));
#30226=CARTESIAN_POINT('Ctrl Pts',(13.8267841057906,-16.4660316469341,7.02345833333327));
#30227=CARTESIAN_POINT('Ctrl Pts',(14.3845227371938,-17.4320632938683,6.98179166666661));
#30228=CARTESIAN_POINT('Ctrl Pts',(15.5,-17.4320632938683,6.94012499999994));
#30229=CARTESIAN_POINT('Ctrl Pts',(16.6154772628062,-17.4320632938683,6.89845833333327));
#30230=CARTESIAN_POINT('Ctrl Pts',(17.1732158942094,-16.4660316469341,6.8567916666666));
#30231=CARTESIAN_POINT('Ctrl Pts',(17.7309545256125,-15.5,6.81512499999994));
#30232=CARTESIAN_POINT('Ctrl Pts',(17.1732158942094,-14.5339683530659,6.77345833333327));
#30233=CARTESIAN_POINT('Ctrl Pts',(16.6154772628062,-13.5679367061317,6.7317916666666));
#30234=CARTESIAN_POINT('Ctrl Pts',(15.5,-13.5679367061317,6.69012499999994));
#30235=CARTESIAN_POINT('Ctrl Pts',(14.3845227371938,-13.5679367061317,6.64845833333327));
#30236=CARTESIAN_POINT('Ctrl Pts',(13.8267841057906,-14.5339683530659,6.6067916666666));
#30237=CARTESIAN_POINT('Ctrl Pts',(13.2690454743875,-15.5,6.56512499999993));
#30238=CARTESIAN_POINT('Ctrl Pts',(13.8267841057906,-16.4660316469341,6.52345833333327));
#30239=CARTESIAN_POINT('Ctrl Pts',(14.3845227371938,-17.4320632938683,6.4817916666666));
#30240=CARTESIAN_POINT('Ctrl Pts',(15.5,-17.4320632938683,6.44012499999993));
#30241=CARTESIAN_POINT('Ctrl Pts',(16.6154772628062,-17.4320632938683,6.39845833333327));
#30242=CARTESIAN_POINT('Ctrl Pts',(17.1732158942094,-16.4660316469341,6.3567916666666));
#30243=CARTESIAN_POINT('Ctrl Pts',(17.7309545256125,-15.5,6.31512499999993));
#30244=CARTESIAN_POINT('Ctrl Pts',(17.1732158942094,-14.5339683530659,6.27345833333326));
#30245=CARTESIAN_POINT('Ctrl Pts',(16.6154772628062,-13.5679367061317,6.2317916666666));
#30246=CARTESIAN_POINT('Ctrl Pts',(15.5,-13.5679367061317,6.19012499999993));
#30247=CARTESIAN_POINT('Ctrl Pts',(14.3845227371938,-13.5679367061317,6.14845833333326));
#30248=CARTESIAN_POINT('Ctrl Pts',(13.8267841057906,-14.5339683530659,6.10679166666659));
#30249=CARTESIAN_POINT('Ctrl Pts',(13.2690454743875,-15.5,6.06512499999993));
#30250=CARTESIAN_POINT('Ctrl Pts',(13.8267841057906,-16.4660316469341,6.02345833333326));
#30251=CARTESIAN_POINT('Ctrl Pts',(14.3845227371938,-17.4320632938683,5.98179166666659));
#30252=CARTESIAN_POINT('Ctrl Pts',(15.5,-17.4320632938683,5.94012499999993));
#30253=CARTESIAN_POINT('Ctrl Pts',(16.6154772628062,-17.4320632938683,5.89845833333326));
#30254=CARTESIAN_POINT('Ctrl Pts',(17.1732158942094,-16.4660316469341,5.85679166666659));
#30255=CARTESIAN_POINT('Ctrl Pts',(17.7309545256125,-15.5,5.81512499999992));
#30256=CARTESIAN_POINT('Ctrl Pts',(17.1732158942094,-14.5339683530659,5.77345833333326));
#30257=CARTESIAN_POINT('Ctrl Pts',(16.6154772628062,-13.5679367061317,5.73179166666659));
#30258=CARTESIAN_POINT('Ctrl Pts',(15.5,-13.5679367061317,5.69012499999992));
#30259=CARTESIAN_POINT('Ctrl Pts',(14.3845227371938,-13.5679367061317,5.64845833333326));
#30260=CARTESIAN_POINT('Ctrl Pts',(13.8267841057906,-14.5339683530659,5.60679166666659));
#30261=CARTESIAN_POINT('Ctrl Pts',(13.2690454743875,-15.5,5.56512499999992));
#30262=CARTESIAN_POINT('Ctrl Pts',(13.8267841057906,-16.4660316469341,5.52345833333325));
#30263=CARTESIAN_POINT('Ctrl Pts',(14.3845227371938,-17.4320632938683,5.48179166666659));
#30264=CARTESIAN_POINT('Ctrl Pts',(15.5,-17.4320632938683,5.44012499999992));
#30265=CARTESIAN_POINT('Ctrl Pts',(16.6154772628062,-17.4320632938683,5.39845833333325));
#30266=CARTESIAN_POINT('Ctrl Pts',(17.1732158942094,-16.4660316469341,5.35679166666658));
#30267=CARTESIAN_POINT('Ctrl Pts',(17.7309545256125,-15.5,5.31512499999992));
#30268=CARTESIAN_POINT('Ctrl Pts',(17.1732158942094,-14.5339683530659,5.27345833333325));
#30269=CARTESIAN_POINT('Ctrl Pts',(16.6154772628062,-13.5679367061317,5.23179166666658));
#30270=CARTESIAN_POINT('Ctrl Pts',(15.5,-13.5679367061317,5.19012499999992));
#30271=CARTESIAN_POINT('Ctrl Pts',(14.3845227371938,-13.5679367061317,5.14845833333325));
#30272=CARTESIAN_POINT('Ctrl Pts',(13.8267841057906,-14.5339683530659,5.10679166666658));
#30273=CARTESIAN_POINT('Ctrl Pts',(13.2690454743875,-15.5,5.06512499999991));
#30274=CARTESIAN_POINT('Ctrl Pts',(13.8267841057906,-16.4660316469341,5.02345833333325));
#30275=CARTESIAN_POINT('Ctrl Pts',(14.3845227371938,-17.4320632938683,4.98179166666658));
#30276=CARTESIAN_POINT('Ctrl Pts',(15.5,-17.4320632938683,4.94012499999991));
#30277=CARTESIAN_POINT('Ctrl Pts',(16.6154772628062,-17.4320632938683,4.89845833333325));
#30278=CARTESIAN_POINT('Ctrl Pts',(17.1732158942094,-16.4660316469341,4.85679166666658));
#30279=CARTESIAN_POINT('Ctrl Pts',(17.7309545256125,-15.5,4.81512499999991));
#30280=CARTESIAN_POINT('Ctrl Pts',(17.1732158942094,-14.5339683530659,4.77345833333324));
#30281=CARTESIAN_POINT('Ctrl Pts',(16.6154772628062,-13.5679367061317,4.73179166666658));
#30282=CARTESIAN_POINT('Ctrl Pts',(15.5,-13.5679367061317,4.69012499999991));
#30283=CARTESIAN_POINT('Ctrl Pts',(14.3845227371938,-13.5679367061317,4.64845833333324));
#30284=CARTESIAN_POINT('Ctrl Pts',(13.8267841057906,-14.5339683530659,4.60679166666657));
#30285=CARTESIAN_POINT('Ctrl Pts',(13.2690454743875,-15.5,4.56512499999991));
#30286=CARTESIAN_POINT('Ctrl Pts',(13.8267841057906,-16.4660316469341,4.52345833333324));
#30287=CARTESIAN_POINT('Ctrl Pts',(14.3845227371938,-17.4320632938683,4.48179166666657));
#30288=CARTESIAN_POINT('Ctrl Pts',(15.5,-17.4320632938683,4.44012499999991));
#30289=CARTESIAN_POINT('Ctrl Pts',(16.6154772628062,-17.4320632938683,4.39845833333324));
#30290=CARTESIAN_POINT('Ctrl Pts',(17.1732158942094,-16.4660316469341,4.35679166666657));
#30291=CARTESIAN_POINT('Ctrl Pts',(17.7309545256125,-15.5,4.31512499999991));
#30292=CARTESIAN_POINT('Ctrl Pts',(17.1732158942094,-14.5339683530659,4.27345833333324));
#30293=CARTESIAN_POINT('Ctrl Pts',(16.6154772628062,-13.5679367061317,4.23179166666657));
#30294=CARTESIAN_POINT('Ctrl Pts',(15.5,-13.5679367061317,4.1901249999999));
#30295=CARTESIAN_POINT('Ctrl Pts',(14.3845227371938,-13.5679367061317,4.14845833333324));
#30296=CARTESIAN_POINT('Ctrl Pts',(13.8267841057906,-14.5339683530659,4.10679166666657));
#30297=CARTESIAN_POINT('Ctrl Pts',(13.2690454743875,-15.5,4.0651249999999));
#30298=CARTESIAN_POINT('Ctrl Pts',(13.8267841057906,-16.4660316469341,4.02345833333323));
#30299=CARTESIAN_POINT('Ctrl Pts',(14.3845227371938,-17.4320632938683,3.98179166666657));
#30300=CARTESIAN_POINT('Ctrl Pts',(15.5,-17.4320632938683,3.9401249999999));
#30301=CARTESIAN_POINT('Ctrl Pts',(16.6154772628062,-17.4320632938683,3.89845833333323));
#30302=CARTESIAN_POINT('Ctrl Pts',(17.1732158942094,-16.4660316469341,3.85679166666657));
#30303=CARTESIAN_POINT('Ctrl Pts',(17.7309545256125,-15.5,3.8151249999999));
#30304=CARTESIAN_POINT('Ctrl Pts',(17.1732158942094,-14.5339683530659,3.77345833333323));
#30305=CARTESIAN_POINT('Ctrl Pts',(16.6154772628062,-13.5679367061317,3.73179166666656));
#30306=CARTESIAN_POINT('Ctrl Pts',(15.5,-13.5679367061317,3.6901249999999));
#30307=CARTESIAN_POINT('Ctrl Pts',(14.3845227371938,-13.5679367061317,3.64845833333323));
#30308=CARTESIAN_POINT('Ctrl Pts',(13.8267841057906,-14.5339683530659,3.60679166666656));
#30309=CARTESIAN_POINT('Ctrl Pts',(13.2690454743875,-15.5,3.5651249999999));
#30310=CARTESIAN_POINT('Ctrl Pts',(13.8267841057906,-16.4660316469341,3.52345833333323));
#30311=CARTESIAN_POINT('Ctrl Pts',(14.3845227371938,-17.4320632938683,3.48179166666656));
#30312=CARTESIAN_POINT('Ctrl Pts',(15.5,-17.4320632938683,3.44012499999989));
#30313=CARTESIAN_POINT('Ctrl Pts',(16.6154772628062,-17.4320632938683,3.39845833333323));
#30314=CARTESIAN_POINT('Ctrl Pts',(17.1732158942094,-16.4660316469341,3.35679166666656));
#30315=CARTESIAN_POINT('Ctrl Pts',(17.7309545256125,-15.5,3.31512499999989));
#30316=CARTESIAN_POINT('Ctrl Pts',(17.1732158942094,-14.5339683530659,3.27345833333322));
#30317=CARTESIAN_POINT('Ctrl Pts',(16.6154772628062,-13.5679367061317,3.23179166666656));
#30318=CARTESIAN_POINT('Ctrl Pts',(15.5,-13.5679367061317,3.19012499999989));
#30319=CARTESIAN_POINT('Ctrl Pts',(14.3845227371938,-13.5679367061317,3.14845833333322));
#30320=CARTESIAN_POINT('Ctrl Pts',(13.8267841057906,-14.5339683530659,3.10679166666655));
#30321=CARTESIAN_POINT('Ctrl Pts',(13.2690454743875,-15.5,3.06512499999989));
#30322=CARTESIAN_POINT('Ctrl Pts',(13.8267841057906,-16.4660316469341,3.02345833333322));
#30323=CARTESIAN_POINT('Ctrl Pts',(14.3845227371938,-17.4320632938683,2.98179166666655));
#30324=CARTESIAN_POINT('Ctrl Pts',(15.5,-17.4320632938683,2.94012499999989));
#30325=CARTESIAN_POINT('Ctrl Pts',(16.6154772628062,-17.4320632938683,2.89845833333322));
#30326=CARTESIAN_POINT('Ctrl Pts',(17.1732158942094,-16.4660316469341,2.85679166666655));
#30327=CARTESIAN_POINT('Ctrl Pts',(17.7309545256125,-15.5,2.81512499999988));
#30328=CARTESIAN_POINT('Ctrl Pts',(17.1732158942094,-14.5339683530659,2.77345833333322));
#30329=CARTESIAN_POINT('Ctrl Pts',(16.6154772628062,-13.5679367061317,2.73179166666655));
#30330=CARTESIAN_POINT('Ctrl Pts',(15.5,-13.5679367061317,2.69012499999988));
#30331=CARTESIAN_POINT('Ctrl Pts',(14.3845227371938,-13.5679367061317,2.64845833333321));
#30332=CARTESIAN_POINT('Ctrl Pts',(13.8267841057906,-14.5339683530659,2.60679166666655));
#30333=CARTESIAN_POINT('Ctrl Pts',(13.2690454743875,-15.5,2.56512499999988));
#30334=CARTESIAN_POINT('Ctrl Pts',(13.8267841057906,-16.4660316469341,2.52345833333321));
#30335=CARTESIAN_POINT('Ctrl Pts',(14.3845227371938,-17.4320632938683,2.48179166666655));
#30336=CARTESIAN_POINT('Ctrl Pts',(15.5,-17.4320632938683,2.44012499999988));
#30337=CARTESIAN_POINT('Ctrl Pts',(16.6154772628062,-17.4320632938683,2.39845833333321));
#30338=CARTESIAN_POINT('Ctrl Pts',(17.1732158942094,-16.4660316469341,2.35679166666655));
#30339=CARTESIAN_POINT('Ctrl Pts',(17.7309545256125,-15.5,2.31512499999988));
#30340=CARTESIAN_POINT('Ctrl Pts',(17.1732158942094,-14.5339683530659,2.27345833333321));
#30341=CARTESIAN_POINT('Ctrl Pts',(16.6154772628062,-13.5679367061317,2.23179166666654));
#30342=CARTESIAN_POINT('Ctrl Pts',(15.5,-13.5679367061317,2.19012499999988));
#30343=CARTESIAN_POINT('Ctrl Pts',(14.3845227371938,-13.5679367061317,2.14845833333321));
#30344=CARTESIAN_POINT('Ctrl Pts',(13.8267841057906,-14.5339683530659,2.10679166666654));
#30345=CARTESIAN_POINT('Ctrl Pts',(13.2690454743875,-15.5,2.06512499999987));
#30346=CARTESIAN_POINT('Ctrl Pts',(13.8267841057906,-16.4660316469341,2.02345833333321));
#30347=CARTESIAN_POINT('Ctrl Pts',(14.3845227371938,-17.4320632938683,1.98179166666654));
#30348=CARTESIAN_POINT('Ctrl Pts',(15.5,-17.4320632938683,1.94012499999987));
#30349=CARTESIAN_POINT('Ctrl Pts',(16.6154772628062,-17.4320632938683,1.89845833333321));
#30350=CARTESIAN_POINT('Ctrl Pts',(17.1732158942094,-16.4660316469341,1.85679166666654));
#30351=CARTESIAN_POINT('Ctrl Pts',(17.7309545256125,-15.5,1.81512499999987));
#30352=CARTESIAN_POINT('Ctrl Pts',(17.1732158942094,-14.5339683530659,1.7734583333332));
#30353=CARTESIAN_POINT('Ctrl Pts',(16.6154772628062,-13.5679367061317,1.73179166666654));
#30354=CARTESIAN_POINT('Ctrl Pts',(15.5,-13.5679367061317,1.69012499999987));
#30355=CARTESIAN_POINT('Ctrl Pts',(14.3845227371938,-13.5679367061317,1.6484583333332));
#30356=CARTESIAN_POINT('Ctrl Pts',(13.8267841057906,-14.5339683530659,1.60679166666653));
#30357=CARTESIAN_POINT('Ctrl Pts',(13.2690454743875,-15.5,1.56512499999987));
#30358=CARTESIAN_POINT('Ctrl Pts',(13.8267841057906,-16.4660316469341,1.5234583333332));
#30359=CARTESIAN_POINT('Ctrl Pts',(14.3845227371938,-17.4320632938683,1.48179166666653));
#30360=CARTESIAN_POINT('Ctrl Pts',(15.5,-17.4320632938683,1.44012499999987));
#30361=CARTESIAN_POINT('Ctrl Pts',(16.6154772628062,-17.4320632938683,1.3984583333332));
#30362=CARTESIAN_POINT('Ctrl Pts',(17.1732158942094,-16.4660316469341,1.35679166666653));
#30363=CARTESIAN_POINT('Ctrl Pts',(17.7309545256125,-15.5,1.31512499999987));
#30364=CARTESIAN_POINT('Ctrl Pts',(17.1732158942094,-14.5339683530659,1.2734583333332));
#30365=CARTESIAN_POINT('Ctrl Pts',(16.6154772628062,-13.5679367061317,1.23179166666653));
#30366=CARTESIAN_POINT('Ctrl Pts',(15.5,-13.5679367061317,1.19012499999986));
#30367=CARTESIAN_POINT('Ctrl Pts',(14.3845227371938,-13.5679367061317,1.1484583333332));
#30368=CARTESIAN_POINT('Ctrl Pts',(13.8267841057906,-14.5339683530659,1.10679166666653));
#30369=CARTESIAN_POINT('Ctrl Pts',(13.2690454743875,-15.5,1.06512499999986));
#30370=CARTESIAN_POINT('Ctrl Pts',(13.8267841057906,-16.4660316469341,1.02345833333319));
#30371=CARTESIAN_POINT('Ctrl Pts',(14.3845227371938,-17.4320632938683,0.981791666666527));
#30372=CARTESIAN_POINT('Ctrl Pts',(15.5,-17.4320632938683,0.94012499999986));
#30373=CARTESIAN_POINT('Ctrl Pts',(16.6154772628062,-17.4320632938683,0.898458333333192));
#30374=CARTESIAN_POINT('Ctrl Pts',(17.1732158942094,-16.4660316469341,0.856791666666525));
#30375=CARTESIAN_POINT('Ctrl Pts',(17.7309545256125,-15.5,0.815124999999858));
#30376=CARTESIAN_POINT('Ctrl Pts',(17.1732158942094,-14.5339683530659,0.77345833333319));
#30377=CARTESIAN_POINT('Ctrl Pts',(16.6154772628062,-13.5679367061317,0.731791666666523));
#30378=CARTESIAN_POINT('Ctrl Pts',(15.5,-13.5679367061317,0.690124999999856));
#30379=CARTESIAN_POINT('Ctrl Pts',(14.3845227371938,-13.5679367061317,0.648458333333188));
#30380=CARTESIAN_POINT('Ctrl Pts',(13.8267841057906,-14.5339683530659,0.606791666666521));
#30381=CARTESIAN_POINT('Ctrl Pts',(13.2690454743875,-15.5,0.565124999999854));
#30382=CARTESIAN_POINT('Ctrl Pts',(13.8267841057906,-16.4660316469341,0.523458333333187));
#30383=CARTESIAN_POINT('Ctrl Pts',(14.3845227371938,-17.4320632938683,0.481791666666519));
#30384=CARTESIAN_POINT('Ctrl Pts',(15.5,-17.4320632938683,0.440124999999852));
#30385=CARTESIAN_POINT('Ctrl Pts',(16.6154772628062,-17.4320632938683,0.398458333333185));
#30386=CARTESIAN_POINT('Ctrl Pts',(17.1732158942094,-16.4660316469341,0.356791666666518));
#30387=CARTESIAN_POINT('Ctrl Pts',(17.7309545256125,-15.5,0.31512499999985));
#30388=CARTESIAN_POINT('Ctrl Pts',(17.1732158942094,-14.5339683530659,0.273458333333183));
#30389=CARTESIAN_POINT('Ctrl Pts',(16.6154772628062,-13.5679367061317,0.231791666666516));
#30390=CARTESIAN_POINT('Ctrl Pts',(15.5,-13.5679367061317,0.190124999999848));
#30391=CARTESIAN_POINT('Ctrl Pts',(14.3845227371938,-13.5679367061317,0.148458333333183));
#30392=CARTESIAN_POINT('Ctrl Pts',(13.8267841057906,-14.5339683530659,0.106791666666516));
#30393=CARTESIAN_POINT('Ctrl Pts',(13.2690454743875,-15.5,0.0651249999998483));
#30394=CARTESIAN_POINT('Ctrl Pts',(13.8267841057906,-16.4660316469341,0.023458333333181));
#30395=CARTESIAN_POINT('Ctrl Pts',(14.3845227371938,-17.4320632938683,-0.0182083333334863));
#30396=CARTESIAN_POINT('Ctrl Pts',(15.5,-17.4320632938683,-0.0598750000001536));
#30397=CARTESIAN_POINT('Ctrl Pts',(16.6154772628062,-17.4320632938683,-0.101541666666821));
#30398=CARTESIAN_POINT('Ctrl Pts',(17.1732158942094,-16.4660316469341,-0.143208333333488));
#30399=CARTESIAN_POINT('Ctrl Pts',(17.7309545256125,-15.5,-0.184875000000155));
#30400=CARTESIAN_POINT('Ctrl Pts',(17.1732158942094,-14.5339683530659,-0.226541666666823));
#30401=CARTESIAN_POINT('Ctrl Pts',(16.6154772628062,-13.5679367061317,-0.26820833333349));
#30402=CARTESIAN_POINT('Ctrl Pts',(15.5,-13.5679367061317,-0.309875000000157));
#30403=CARTESIAN_POINT('Ctrl Pts',(14.3845227371938,-13.5679367061317,-0.351541666666825));
#30404=CARTESIAN_POINT('Ctrl Pts',(13.8267841057906,-14.5339683530659,-0.393208333333492));
#30405=CARTESIAN_POINT('Ctrl Pts',(13.2690454743875,-15.5,-0.434875000000159));
#30406=CARTESIAN_POINT('Ctrl Pts',(13.8267841057906,-16.4660316469341,-0.476541666666826));
#30407=CARTESIAN_POINT('Ctrl Pts',(14.3845227371938,-17.4320632938683,-0.518208333333494));
#30408=CARTESIAN_POINT('Ctrl Pts',(15.5,-17.4320632938683,-0.559875000000161));
#30409=CARTESIAN_POINT('Ctrl Pts',(16.6154772628062,-17.4320632938683,-0.601541666666828));
#30410=CARTESIAN_POINT('Ctrl Pts',(17.1732158942094,-16.4660316469341,-0.643208333333495));
#30411=CARTESIAN_POINT('Ctrl Pts',(17.7309545256125,-15.5,-0.684875000000163));
#30412=CARTESIAN_POINT('Ctrl Pts',(17.1732158942094,-14.5339683530659,-0.72654166666683));
#30413=CARTESIAN_POINT('Ctrl Pts',(16.6154772628062,-13.5679367061317,-0.768208333333497));
#30414=CARTESIAN_POINT('Ctrl Pts',(15.5,-13.5679367061317,-0.809875000000165));
#30415=CARTESIAN_POINT('Ctrl Pts',(14.3845227371938,-13.5679367061317,-0.851541666666832));
#30416=CARTESIAN_POINT('Ctrl Pts',(13.8267841057906,-14.5339683530659,-0.893208333333499));
#30417=CARTESIAN_POINT('Ctrl Pts',(13.2690454743875,-15.5,-0.934875000000167));
#30418=CARTESIAN_POINT('Ctrl Pts',(13.8267841057906,-16.4660316469341,-0.976541666666834));
#30419=CARTESIAN_POINT('Ctrl Pts',(14.3845227371938,-17.4320632938683,-1.0182083333335));
#30420=CARTESIAN_POINT('Ctrl Pts',(15.5,-17.4320632938683,-1.05987500000017));
#30421=CARTESIAN_POINT('Ctrl Pts',(16.6154772628062,-17.4320632938683,-1.10154166666683));
#30422=CARTESIAN_POINT('Ctrl Pts',(17.1732158942094,-16.4660316469341,-1.1432083333335));
#30423=CARTESIAN_POINT('Ctrl Pts',(17.7309545256125,-15.5,-1.18487500000017));
#30424=CARTESIAN_POINT('Ctrl Pts',(17.1732158942094,-14.5339683530659,-1.22654166666684));
#30425=CARTESIAN_POINT('Ctrl Pts',(16.6154772628062,-13.5679367061317,-1.2682083333335));
#30426=CARTESIAN_POINT('Ctrl Pts',(15.5,-13.5679367061317,-1.30987500000017));
#30427=CARTESIAN_POINT('Ctrl Pts',(14.3845227371938,-13.5679367061317,-1.35154166666684));
#30428=CARTESIAN_POINT('Ctrl Pts',(13.8267841057906,-14.5339683530659,-1.3932083333335));
#30429=CARTESIAN_POINT('Ctrl Pts',(13.2690454743875,-15.5,-1.43487500000017));
#30430=CARTESIAN_POINT('Ctrl Pts',(13.8267841057906,-16.4660316469341,-1.47654166666684));
#30431=CARTESIAN_POINT('Ctrl Pts',(14.3845227371938,-17.4320632938683,-1.51820833333351));
#30432=CARTESIAN_POINT('Ctrl Pts',(15.5,-17.4320632938683,-1.55987500000017));
#30433=CARTESIAN_POINT('Ctrl Pts',(16.6154772628062,-17.4320632938683,-1.60154166666684));
#30434=CARTESIAN_POINT('Ctrl Pts',(17.1732158942094,-16.4660316469341,-1.64320833333351));
#30435=CARTESIAN_POINT('Ctrl Pts',(17.7309545256125,-15.5,-1.68487500000018));
#30436=CARTESIAN_POINT('Ctrl Pts',(17.1732158942094,-14.5339683530659,-1.72654166666684));
#30437=CARTESIAN_POINT('Ctrl Pts',(16.9678753992805,-14.1783081829978,-1.74188192368624));
#30438=CARTESIAN_POINT('Ctrl Pts',(16.6356255246375,-13.9369186715641,-1.75949830599533));
#30439=CARTESIAN_POINT('Ctrl Pts',(15.5,-17.080235786987,11.2369972941938));
#30440=CARTESIAN_POINT('Ctrl Pts',(16.412349557,-17.080235786987,11.1953306275271));
#30441=CARTESIAN_POINT('Ctrl Pts',(16.8685243355001,-16.2901178934935,11.1536639608605));
#30442=CARTESIAN_POINT('Ctrl Pts',(17.3246991140001,-15.5,11.1119972941938));
#30443=CARTESIAN_POINT('Ctrl Pts',(16.8685243355001,-14.7098821065065,11.0703306275271));
#30444=CARTESIAN_POINT('Ctrl Pts',(16.412349557,-13.919764213013,11.0286639608605));
#30445=CARTESIAN_POINT('Ctrl Pts',(15.5,-13.919764213013,10.9869972941938));
#30446=CARTESIAN_POINT('Ctrl Pts',(14.587650443,-13.919764213013,10.9453306275271));
#30447=CARTESIAN_POINT('Ctrl Pts',(14.1314756644999,-14.7098821065065,10.9036639608605));
#30448=CARTESIAN_POINT('Ctrl Pts',(13.6753008859999,-15.5,10.8619972941938));
#30449=CARTESIAN_POINT('Ctrl Pts',(14.1314756644999,-16.2901178934935,10.8203306275271));
#30450=CARTESIAN_POINT('Ctrl Pts',(14.587650443,-17.080235786987,10.7786639608605));
#30451=CARTESIAN_POINT('Ctrl Pts',(15.5,-17.080235786987,10.7369972941938));
#30452=CARTESIAN_POINT('Ctrl Pts',(16.412349557,-17.080235786987,10.6953306275271));
#30453=CARTESIAN_POINT('Ctrl Pts',(16.8685243355001,-16.2901178934935,10.6536639608605));
#30454=CARTESIAN_POINT('Ctrl Pts',(17.3246991140001,-15.5,10.6119972941938));
#30455=CARTESIAN_POINT('Ctrl Pts',(16.8685243355001,-14.7098821065065,10.5703306275271));
#30456=CARTESIAN_POINT('Ctrl Pts',(16.412349557,-13.919764213013,10.5286639608605));
#30457=CARTESIAN_POINT('Ctrl Pts',(15.5,-13.919764213013,10.4869972941938));
#30458=CARTESIAN_POINT('Ctrl Pts',(14.587650443,-13.919764213013,10.4453306275271));
#30459=CARTESIAN_POINT('Ctrl Pts',(14.1314756644999,-14.7098821065065,10.4036639608605));
#30460=CARTESIAN_POINT('Ctrl Pts',(13.6753008859999,-15.5,10.3619972941938));
#30461=CARTESIAN_POINT('Ctrl Pts',(14.1314756644999,-16.2901178934935,10.3203306275271));
#30462=CARTESIAN_POINT('Ctrl Pts',(14.587650443,-17.080235786987,10.2786639608605));
#30463=CARTESIAN_POINT('Ctrl Pts',(15.5,-17.080235786987,10.2369972941938));
#30464=CARTESIAN_POINT('Ctrl Pts',(16.412349557,-17.080235786987,10.1953306275271));
#30465=CARTESIAN_POINT('Ctrl Pts',(16.8685243355001,-16.2901178934935,10.1536639608605));
#30466=CARTESIAN_POINT('Ctrl Pts',(17.3246991140001,-15.5,10.1119972941938));
#30467=CARTESIAN_POINT('Ctrl Pts',(16.8685243355001,-14.7098821065065,10.0703306275271));
#30468=CARTESIAN_POINT('Ctrl Pts',(16.412349557,-13.919764213013,10.0286639608605));
#30469=CARTESIAN_POINT('Ctrl Pts',(15.5,-13.919764213013,9.98699729419378));
#30470=CARTESIAN_POINT('Ctrl Pts',(14.587650443,-13.919764213013,9.94533062752712));
#30471=CARTESIAN_POINT('Ctrl Pts',(14.1314756644999,-14.7098821065065,9.90366396086045));
#30472=CARTESIAN_POINT('Ctrl Pts',(13.6753008859999,-15.5,9.86199729419378));
#30473=CARTESIAN_POINT('Ctrl Pts',(14.1314756644999,-16.2901178934935,9.82033062752711));
#30474=CARTESIAN_POINT('Ctrl Pts',(14.587650443,-17.080235786987,9.77866396086045));
#30475=CARTESIAN_POINT('Ctrl Pts',(15.5,-17.080235786987,9.73699729419378));
#30476=CARTESIAN_POINT('Ctrl Pts',(16.412349557,-17.080235786987,9.69533062752711));
#30477=CARTESIAN_POINT('Ctrl Pts',(16.8685243355001,-16.2901178934935,9.65366396086044));
#30478=CARTESIAN_POINT('Ctrl Pts',(17.3246991140001,-15.5,9.61199729419378));
#30479=CARTESIAN_POINT('Ctrl Pts',(16.8685243355001,-14.7098821065065,9.57033062752711));
#30480=CARTESIAN_POINT('Ctrl Pts',(16.412349557,-13.919764213013,9.52866396086044));
#30481=CARTESIAN_POINT('Ctrl Pts',(15.5,-13.919764213013,9.48699729419378));
#30482=CARTESIAN_POINT('Ctrl Pts',(14.587650443,-13.919764213013,9.44533062752711));
#30483=CARTESIAN_POINT('Ctrl Pts',(14.1314756644999,-14.7098821065065,9.40366396086044));
#30484=CARTESIAN_POINT('Ctrl Pts',(13.6753008859999,-15.5,9.36199729419377));
#30485=CARTESIAN_POINT('Ctrl Pts',(14.1314756644999,-16.2901178934935,9.32033062752711));
#30486=CARTESIAN_POINT('Ctrl Pts',(14.587650443,-17.080235786987,9.27866396086044));
#30487=CARTESIAN_POINT('Ctrl Pts',(15.5,-17.080235786987,9.23699729419377));
#30488=CARTESIAN_POINT('Ctrl Pts',(16.412349557,-17.080235786987,9.19533062752711));
#30489=CARTESIAN_POINT('Ctrl Pts',(16.8685243355001,-16.2901178934935,9.15366396086044));
#30490=CARTESIAN_POINT('Ctrl Pts',(17.3246991140001,-15.5,9.11199729419377));
#30491=CARTESIAN_POINT('Ctrl Pts',(16.8685243355001,-14.7098821065065,9.0703306275271));
#30492=CARTESIAN_POINT('Ctrl Pts',(16.412349557,-13.919764213013,9.02866396086044));
#30493=CARTESIAN_POINT('Ctrl Pts',(15.5,-13.919764213013,8.98699729419377));
#30494=CARTESIAN_POINT('Ctrl Pts',(14.587650443,-13.919764213013,8.9453306275271));
#30495=CARTESIAN_POINT('Ctrl Pts',(14.1314756644999,-14.7098821065065,8.90366396086044));
#30496=CARTESIAN_POINT('Ctrl Pts',(13.6753008859999,-15.5,8.86199729419377));
#30497=CARTESIAN_POINT('Ctrl Pts',(14.1314756644999,-16.2901178934935,8.8203306275271));
#30498=CARTESIAN_POINT('Ctrl Pts',(14.587650443,-17.080235786987,8.77866396086043));
#30499=CARTESIAN_POINT('Ctrl Pts',(15.5,-17.080235786987,8.73699729419377));
#30500=CARTESIAN_POINT('Ctrl Pts',(16.412349557,-17.080235786987,8.6953306275271));
#30501=CARTESIAN_POINT('Ctrl Pts',(16.8685243355001,-16.2901178934935,8.65366396086043));
#30502=CARTESIAN_POINT('Ctrl Pts',(17.3246991140001,-15.5,8.61199729419376));
#30503=CARTESIAN_POINT('Ctrl Pts',(16.8685243355001,-14.7098821065065,8.57033062752709));
#30504=CARTESIAN_POINT('Ctrl Pts',(16.412349557,-13.919764213013,8.52866396086043));
#30505=CARTESIAN_POINT('Ctrl Pts',(15.5,-13.919764213013,8.48699729419376));
#30506=CARTESIAN_POINT('Ctrl Pts',(14.587650443,-13.919764213013,8.44533062752709));
#30507=CARTESIAN_POINT('Ctrl Pts',(14.1314756644999,-14.7098821065065,8.40366396086043));
#30508=CARTESIAN_POINT('Ctrl Pts',(13.6753008859999,-15.5,8.36199729419376));
#30509=CARTESIAN_POINT('Ctrl Pts',(14.1314756644999,-16.2901178934935,8.32033062752709));
#30510=CARTESIAN_POINT('Ctrl Pts',(14.587650443,-17.080235786987,8.27866396086043));
#30511=CARTESIAN_POINT('Ctrl Pts',(15.5,-17.080235786987,8.23699729419376));
#30512=CARTESIAN_POINT('Ctrl Pts',(16.412349557,-17.080235786987,8.19533062752709));
#30513=CARTESIAN_POINT('Ctrl Pts',(16.8685243355001,-16.2901178934935,8.15366396086043));
#30514=CARTESIAN_POINT('Ctrl Pts',(17.3246991140001,-15.5,8.11199729419376));
#30515=CARTESIAN_POINT('Ctrl Pts',(16.8685243355001,-14.7098821065065,8.07033062752709));
#30516=CARTESIAN_POINT('Ctrl Pts',(16.412349557,-13.919764213013,8.02866396086042));
#30517=CARTESIAN_POINT('Ctrl Pts',(15.5,-13.919764213013,7.98699729419376));
#30518=CARTESIAN_POINT('Ctrl Pts',(14.587650443,-13.919764213013,7.94533062752709));
#30519=CARTESIAN_POINT('Ctrl Pts',(14.1314756644999,-14.7098821065065,7.90366396086042));
#30520=CARTESIAN_POINT('Ctrl Pts',(13.6753008859999,-15.5,7.86199729419375));
#30521=CARTESIAN_POINT('Ctrl Pts',(14.1314756644999,-16.2901178934935,7.82033062752709));
#30522=CARTESIAN_POINT('Ctrl Pts',(14.587650443,-17.080235786987,7.77866396086042));
#30523=CARTESIAN_POINT('Ctrl Pts',(15.5,-17.080235786987,7.73699729419375));
#30524=CARTESIAN_POINT('Ctrl Pts',(16.412349557,-17.080235786987,7.69533062752709));
#30525=CARTESIAN_POINT('Ctrl Pts',(16.8685243355001,-16.2901178934935,7.65366396086042));
#30526=CARTESIAN_POINT('Ctrl Pts',(17.3246991140001,-15.5,7.61199729419375));
#30527=CARTESIAN_POINT('Ctrl Pts',(16.8685243355001,-14.7098821065065,7.57033062752708));
#30528=CARTESIAN_POINT('Ctrl Pts',(16.412349557,-13.919764213013,7.52866396086041));
#30529=CARTESIAN_POINT('Ctrl Pts',(15.5,-13.919764213013,7.48699729419375));
#30530=CARTESIAN_POINT('Ctrl Pts',(14.587650443,-13.919764213013,7.44533062752708));
#30531=CARTESIAN_POINT('Ctrl Pts',(14.1314756644999,-14.7098821065065,7.40366396086041));
#30532=CARTESIAN_POINT('Ctrl Pts',(13.6753008859999,-15.5,7.36199729419375));
#30533=CARTESIAN_POINT('Ctrl Pts',(14.1314756644999,-16.2901178934935,7.32033062752708));
#30534=CARTESIAN_POINT('Ctrl Pts',(14.587650443,-17.080235786987,7.27866396086041));
#30535=CARTESIAN_POINT('Ctrl Pts',(15.5,-17.080235786987,7.23699729419375));
#30536=CARTESIAN_POINT('Ctrl Pts',(16.412349557,-17.080235786987,7.19533062752708));
#30537=CARTESIAN_POINT('Ctrl Pts',(16.8685243355001,-16.2901178934935,7.15366396086041));
#30538=CARTESIAN_POINT('Ctrl Pts',(17.3246991140001,-15.5,7.11199729419374));
#30539=CARTESIAN_POINT('Ctrl Pts',(16.8685243355001,-14.7098821065065,7.07033062752708));
#30540=CARTESIAN_POINT('Ctrl Pts',(16.412349557,-13.919764213013,7.02866396086041));
#30541=CARTESIAN_POINT('Ctrl Pts',(15.5,-13.919764213013,6.98699729419374));
#30542=CARTESIAN_POINT('Ctrl Pts',(14.587650443,-13.919764213013,6.94533062752707));
#30543=CARTESIAN_POINT('Ctrl Pts',(14.1314756644999,-14.7098821065065,6.90366396086041));
#30544=CARTESIAN_POINT('Ctrl Pts',(13.6753008859999,-15.5,6.86199729419374));
#30545=CARTESIAN_POINT('Ctrl Pts',(14.1314756644999,-16.2901178934935,6.82033062752707));
#30546=CARTESIAN_POINT('Ctrl Pts',(14.587650443,-17.080235786987,6.77866396086041));
#30547=CARTESIAN_POINT('Ctrl Pts',(15.5,-17.080235786987,6.73699729419374));
#30548=CARTESIAN_POINT('Ctrl Pts',(16.412349557,-17.080235786987,6.69533062752707));
#30549=CARTESIAN_POINT('Ctrl Pts',(16.8685243355001,-16.2901178934935,6.65366396086041));
#30550=CARTESIAN_POINT('Ctrl Pts',(17.3246991140001,-15.5,6.61199729419374));
#30551=CARTESIAN_POINT('Ctrl Pts',(16.8685243355001,-14.7098821065065,6.57033062752707));
#30552=CARTESIAN_POINT('Ctrl Pts',(16.412349557,-13.919764213013,6.5286639608604));
#30553=CARTESIAN_POINT('Ctrl Pts',(15.5,-13.919764213013,6.48699729419374));
#30554=CARTESIAN_POINT('Ctrl Pts',(14.587650443,-13.919764213013,6.44533062752707));
#30555=CARTESIAN_POINT('Ctrl Pts',(14.1314756644999,-14.7098821065065,6.4036639608604));
#30556=CARTESIAN_POINT('Ctrl Pts',(13.6753008859999,-15.5,6.36199729419373));
#30557=CARTESIAN_POINT('Ctrl Pts',(14.1314756644999,-16.2901178934935,6.32033062752707));
#30558=CARTESIAN_POINT('Ctrl Pts',(14.587650443,-17.080235786987,6.2786639608604));
#30559=CARTESIAN_POINT('Ctrl Pts',(15.5,-17.080235786987,6.23699729419373));
#30560=CARTESIAN_POINT('Ctrl Pts',(16.412349557,-17.080235786987,6.19533062752706));
#30561=CARTESIAN_POINT('Ctrl Pts',(16.8685243355001,-16.2901178934935,6.1536639608604));
#30562=CARTESIAN_POINT('Ctrl Pts',(17.3246991140001,-15.5,6.11199729419373));
#30563=CARTESIAN_POINT('Ctrl Pts',(16.8685243355001,-14.7098821065065,6.07033062752706));
#30564=CARTESIAN_POINT('Ctrl Pts',(16.412349557,-13.919764213013,6.0286639608604));
#30565=CARTESIAN_POINT('Ctrl Pts',(15.5,-13.919764213013,5.98699729419373));
#30566=CARTESIAN_POINT('Ctrl Pts',(14.587650443,-13.919764213013,5.94533062752706));
#30567=CARTESIAN_POINT('Ctrl Pts',(14.1314756644999,-14.7098821065065,5.9036639608604));
#30568=CARTESIAN_POINT('Ctrl Pts',(13.6753008859999,-15.5,5.86199729419373));
#30569=CARTESIAN_POINT('Ctrl Pts',(14.1314756644999,-16.2901178934935,5.82033062752706));
#30570=CARTESIAN_POINT('Ctrl Pts',(14.587650443,-17.080235786987,5.77866396086039));
#30571=CARTESIAN_POINT('Ctrl Pts',(15.5,-17.080235786987,5.73699729419373));
#30572=CARTESIAN_POINT('Ctrl Pts',(16.412349557,-17.080235786987,5.69533062752706));
#30573=CARTESIAN_POINT('Ctrl Pts',(16.8685243355001,-16.2901178934935,5.65366396086039));
#30574=CARTESIAN_POINT('Ctrl Pts',(17.3246991140001,-15.5,5.61199729419372));
#30575=CARTESIAN_POINT('Ctrl Pts',(16.8685243355001,-14.7098821065065,5.57033062752706));
#30576=CARTESIAN_POINT('Ctrl Pts',(16.412349557,-13.919764213013,5.52866396086039));
#30577=CARTESIAN_POINT('Ctrl Pts',(15.5,-13.919764213013,5.48699729419372));
#30578=CARTESIAN_POINT('Ctrl Pts',(14.587650443,-13.919764213013,5.44533062752706));
#30579=CARTESIAN_POINT('Ctrl Pts',(14.1314756644999,-14.7098821065065,5.40366396086039));
#30580=CARTESIAN_POINT('Ctrl Pts',(13.6753008859999,-15.5,5.36199729419372));
#30581=CARTESIAN_POINT('Ctrl Pts',(14.1314756644999,-16.2901178934935,5.32033062752705));
#30582=CARTESIAN_POINT('Ctrl Pts',(14.587650443,-17.080235786987,5.27866396086039));
#30583=CARTESIAN_POINT('Ctrl Pts',(15.5,-17.080235786987,5.23699729419372));
#30584=CARTESIAN_POINT('Ctrl Pts',(16.412349557,-17.080235786987,5.19533062752705));
#30585=CARTESIAN_POINT('Ctrl Pts',(16.8685243355001,-16.2901178934935,5.15366396086038));
#30586=CARTESIAN_POINT('Ctrl Pts',(17.3246991140001,-15.5,5.11199729419372));
#30587=CARTESIAN_POINT('Ctrl Pts',(16.8685243355001,-14.7098821065065,5.07033062752705));
#30588=CARTESIAN_POINT('Ctrl Pts',(16.412349557,-13.919764213013,5.02866396086038));
#30589=CARTESIAN_POINT('Ctrl Pts',(15.5,-13.919764213013,4.98699729419372));
#30590=CARTESIAN_POINT('Ctrl Pts',(14.587650443,-13.919764213013,4.94533062752705));
#30591=CARTESIAN_POINT('Ctrl Pts',(14.1314756644999,-14.7098821065065,4.90366396086038));
#30592=CARTESIAN_POINT('Ctrl Pts',(13.6753008859999,-15.5,4.86199729419371));
#30593=CARTESIAN_POINT('Ctrl Pts',(14.1314756644999,-16.2901178934935,4.82033062752705));
#30594=CARTESIAN_POINT('Ctrl Pts',(14.587650443,-17.080235786987,4.77866396086038));
#30595=CARTESIAN_POINT('Ctrl Pts',(15.5,-17.080235786987,4.73699729419371));
#30596=CARTESIAN_POINT('Ctrl Pts',(16.412349557,-17.080235786987,4.69533062752705));
#30597=CARTESIAN_POINT('Ctrl Pts',(16.8685243355001,-16.2901178934935,4.65366396086038));
#30598=CARTESIAN_POINT('Ctrl Pts',(17.3246991140001,-15.5,4.61199729419371));
#30599=CARTESIAN_POINT('Ctrl Pts',(16.8685243355001,-14.7098821065065,4.57033062752704));
#30600=CARTESIAN_POINT('Ctrl Pts',(16.412349557,-13.919764213013,4.52866396086038));
#30601=CARTESIAN_POINT('Ctrl Pts',(15.5,-13.919764213013,4.48699729419371));
#30602=CARTESIAN_POINT('Ctrl Pts',(14.587650443,-13.919764213013,4.44533062752704));
#30603=CARTESIAN_POINT('Ctrl Pts',(14.1314756644999,-14.7098821065065,4.40366396086038));
#30604=CARTESIAN_POINT('Ctrl Pts',(13.6753008859999,-15.5,4.36199729419371));
#30605=CARTESIAN_POINT('Ctrl Pts',(14.1314756644999,-16.2901178934935,4.32033062752704));
#30606=CARTESIAN_POINT('Ctrl Pts',(14.587650443,-17.080235786987,4.27866396086037));
#30607=CARTESIAN_POINT('Ctrl Pts',(15.5,-17.080235786987,4.23699729419371));
#30608=CARTESIAN_POINT('Ctrl Pts',(16.412349557,-17.080235786987,4.19533062752704));
#30609=CARTESIAN_POINT('Ctrl Pts',(16.8685243355001,-16.2901178934935,4.15366396086037));
#30610=CARTESIAN_POINT('Ctrl Pts',(17.3246991140001,-15.5,4.1119972941937));
#30611=CARTESIAN_POINT('Ctrl Pts',(16.8685243355001,-14.7098821065065,4.07033062752704));
#30612=CARTESIAN_POINT('Ctrl Pts',(16.412349557,-13.919764213013,4.02866396086037));
#30613=CARTESIAN_POINT('Ctrl Pts',(15.5,-13.919764213013,3.9869972941937));
#30614=CARTESIAN_POINT('Ctrl Pts',(14.587650443,-13.919764213013,3.94533062752703));
#30615=CARTESIAN_POINT('Ctrl Pts',(14.1314756644999,-14.7098821065065,3.90366396086037));
#30616=CARTESIAN_POINT('Ctrl Pts',(13.6753008859999,-15.5,3.8619972941937));
#30617=CARTESIAN_POINT('Ctrl Pts',(14.1314756644999,-16.2901178934935,3.82033062752703));
#30618=CARTESIAN_POINT('Ctrl Pts',(14.587650443,-17.080235786987,3.77866396086037));
#30619=CARTESIAN_POINT('Ctrl Pts',(15.5,-17.080235786987,3.7369972941937));
#30620=CARTESIAN_POINT('Ctrl Pts',(16.412349557,-17.080235786987,3.69533062752703));
#30621=CARTESIAN_POINT('Ctrl Pts',(16.8685243355001,-16.2901178934935,3.65366396086036));
#30622=CARTESIAN_POINT('Ctrl Pts',(17.3246991140001,-15.5,3.6119972941937));
#30623=CARTESIAN_POINT('Ctrl Pts',(16.8685243355001,-14.7098821065065,3.57033062752703));
#30624=CARTESIAN_POINT('Ctrl Pts',(16.412349557,-13.919764213013,3.52866396086036));
#30625=CARTESIAN_POINT('Ctrl Pts',(15.5,-13.919764213013,3.4869972941937));
#30626=CARTESIAN_POINT('Ctrl Pts',(14.587650443,-13.919764213013,3.44533062752703));
#30627=CARTESIAN_POINT('Ctrl Pts',(14.1314756644999,-14.7098821065065,3.40366396086036));
#30628=CARTESIAN_POINT('Ctrl Pts',(13.6753008859999,-15.5,3.36199729419369));
#30629=CARTESIAN_POINT('Ctrl Pts',(14.1314756644999,-16.2901178934935,3.32033062752703));
#30630=CARTESIAN_POINT('Ctrl Pts',(14.587650443,-17.080235786987,3.27866396086036));
#30631=CARTESIAN_POINT('Ctrl Pts',(15.5,-17.080235786987,3.23699729419369));
#30632=CARTESIAN_POINT('Ctrl Pts',(16.412349557,-17.080235786987,3.19533062752703));
#30633=CARTESIAN_POINT('Ctrl Pts',(16.8685243355001,-16.2901178934935,3.15366396086036));
#30634=CARTESIAN_POINT('Ctrl Pts',(17.3246991140001,-15.5,3.11199729419369));
#30635=CARTESIAN_POINT('Ctrl Pts',(16.8685243355001,-14.7098821065065,3.07033062752702));
#30636=CARTESIAN_POINT('Ctrl Pts',(16.412349557,-13.919764213013,3.02866396086036));
#30637=CARTESIAN_POINT('Ctrl Pts',(15.5,-13.919764213013,2.98699729419369));
#30638=CARTESIAN_POINT('Ctrl Pts',(14.587650443,-13.919764213013,2.94533062752702));
#30639=CARTESIAN_POINT('Ctrl Pts',(14.1314756644999,-14.7098821065065,2.90366396086036));
#30640=CARTESIAN_POINT('Ctrl Pts',(13.6753008859999,-15.5,2.86199729419369));
#30641=CARTESIAN_POINT('Ctrl Pts',(14.1314756644999,-16.2901178934935,2.82033062752702));
#30642=CARTESIAN_POINT('Ctrl Pts',(14.587650443,-17.080235786987,2.77866396086035));
#30643=CARTESIAN_POINT('Ctrl Pts',(15.5,-17.080235786987,2.73699729419369));
#30644=CARTESIAN_POINT('Ctrl Pts',(16.412349557,-17.080235786987,2.69533062752702));
#30645=CARTESIAN_POINT('Ctrl Pts',(16.8685243355001,-16.2901178934935,2.65366396086035));
#30646=CARTESIAN_POINT('Ctrl Pts',(17.3246991140001,-15.5,2.61199729419368));
#30647=CARTESIAN_POINT('Ctrl Pts',(16.8685243355001,-14.7098821065065,2.57033062752702));
#30648=CARTESIAN_POINT('Ctrl Pts',(16.412349557,-13.919764213013,2.52866396086035));
#30649=CARTESIAN_POINT('Ctrl Pts',(15.5,-13.919764213013,2.48699729419368));
#30650=CARTESIAN_POINT('Ctrl Pts',(14.587650443,-13.919764213013,2.44533062752701));
#30651=CARTESIAN_POINT('Ctrl Pts',(14.1314756644999,-14.7098821065065,2.40366396086035));
#30652=CARTESIAN_POINT('Ctrl Pts',(13.6753008859999,-15.5,2.36199729419368));
#30653=CARTESIAN_POINT('Ctrl Pts',(14.1314756644999,-16.2901178934935,2.32033062752701));
#30654=CARTESIAN_POINT('Ctrl Pts',(14.587650443,-17.080235786987,2.27866396086035));
#30655=CARTESIAN_POINT('Ctrl Pts',(15.5,-17.080235786987,2.23699729419368));
#30656=CARTESIAN_POINT('Ctrl Pts',(16.412349557,-17.080235786987,2.19533062752701));
#30657=CARTESIAN_POINT('Ctrl Pts',(16.8685243355001,-16.2901178934935,2.15366396086035));
#30658=CARTESIAN_POINT('Ctrl Pts',(17.3246991140001,-15.5,2.11199729419368));
#30659=CARTESIAN_POINT('Ctrl Pts',(16.8685243355001,-14.7098821065065,2.07033062752701));
#30660=CARTESIAN_POINT('Ctrl Pts',(16.412349557,-13.919764213013,2.02866396086034));
#30661=CARTESIAN_POINT('Ctrl Pts',(15.5,-13.919764213013,1.98699729419368));
#30662=CARTESIAN_POINT('Ctrl Pts',(14.587650443,-13.919764213013,1.94533062752701));
#30663=CARTESIAN_POINT('Ctrl Pts',(14.1314756644999,-14.7098821065065,1.90366396086034));
#30664=CARTESIAN_POINT('Ctrl Pts',(13.6753008859999,-15.5,1.86199729419367));
#30665=CARTESIAN_POINT('Ctrl Pts',(14.1314756644999,-16.2901178934935,1.82033062752701));
#30666=CARTESIAN_POINT('Ctrl Pts',(14.587650443,-17.080235786987,1.77866396086034));
#30667=CARTESIAN_POINT('Ctrl Pts',(15.5,-17.080235786987,1.73699729419367));
#30668=CARTESIAN_POINT('Ctrl Pts',(16.412349557,-17.080235786987,1.695330627527));
#30669=CARTESIAN_POINT('Ctrl Pts',(16.8685243355001,-16.2901178934935,1.65366396086034));
#30670=CARTESIAN_POINT('Ctrl Pts',(17.3246991140001,-15.5,1.61199729419367));
#30671=CARTESIAN_POINT('Ctrl Pts',(16.8685243355001,-14.7098821065065,1.570330627527));
#30672=CARTESIAN_POINT('Ctrl Pts',(16.412349557,-13.919764213013,1.52866396086034));
#30673=CARTESIAN_POINT('Ctrl Pts',(15.5,-13.919764213013,1.48699729419367));
#30674=CARTESIAN_POINT('Ctrl Pts',(14.587650443,-13.919764213013,1.445330627527));
#30675=CARTESIAN_POINT('Ctrl Pts',(14.1314756644999,-14.7098821065065,1.40366396086033));
#30676=CARTESIAN_POINT('Ctrl Pts',(13.6753008859999,-15.5,1.36199729419367));
#30677=CARTESIAN_POINT('Ctrl Pts',(14.1314756644999,-16.2901178934935,1.320330627527));
#30678=CARTESIAN_POINT('Ctrl Pts',(14.587650443,-17.080235786987,1.27866396086033));
#30679=CARTESIAN_POINT('Ctrl Pts',(15.5,-17.080235786987,1.23699729419367));
#30680=CARTESIAN_POINT('Ctrl Pts',(16.412349557,-17.080235786987,1.195330627527));
#30681=CARTESIAN_POINT('Ctrl Pts',(16.8685243355001,-16.2901178934935,1.15366396086033));
#30682=CARTESIAN_POINT('Ctrl Pts',(17.3246991140001,-15.5,1.11199729419366));
#30683=CARTESIAN_POINT('Ctrl Pts',(16.8685243355001,-14.7098821065065,1.070330627527));
#30684=CARTESIAN_POINT('Ctrl Pts',(16.412349557,-13.919764213013,1.02866396086033));
#30685=CARTESIAN_POINT('Ctrl Pts',(15.5,-13.919764213013,0.986997294193663));
#30686=CARTESIAN_POINT('Ctrl Pts',(14.587650443,-13.919764213013,0.945330627526996));
#30687=CARTESIAN_POINT('Ctrl Pts',(14.1314756644999,-14.7098821065065,0.903663960860329));
#30688=CARTESIAN_POINT('Ctrl Pts',(13.6753008859999,-15.5,0.861997294193661));
#30689=CARTESIAN_POINT('Ctrl Pts',(14.1314756644999,-16.2901178934935,0.820330627526994));
#30690=CARTESIAN_POINT('Ctrl Pts',(14.587650443,-17.080235786987,0.778663960860328));
#30691=CARTESIAN_POINT('Ctrl Pts',(15.5,-17.080235786987,0.736997294193659));
#30692=CARTESIAN_POINT('Ctrl Pts',(16.412349557,-17.080235786987,0.695330627526992));
#30693=CARTESIAN_POINT('Ctrl Pts',(16.8685243355001,-16.2901178934935,0.653663960860325));
#30694=CARTESIAN_POINT('Ctrl Pts',(17.3246991140001,-15.5,0.611997294193657));
#30695=CARTESIAN_POINT('Ctrl Pts',(16.8685243355001,-14.7098821065065,0.57033062752699));
#30696=CARTESIAN_POINT('Ctrl Pts',(16.412349557,-13.919764213013,0.528663960860323));
#30697=CARTESIAN_POINT('Ctrl Pts',(15.5,-13.919764213013,0.486997294193656));
#30698=CARTESIAN_POINT('Ctrl Pts',(14.587650443,-13.919764213013,0.445330627526988));
#30699=CARTESIAN_POINT('Ctrl Pts',(14.1314756644999,-14.7098821065065,0.403663960860321));
#30700=CARTESIAN_POINT('Ctrl Pts',(13.6753008859999,-15.5,0.361997294193654));
#30701=CARTESIAN_POINT('Ctrl Pts',(14.1314756644999,-16.2901178934935,0.320330627526986));
#30702=CARTESIAN_POINT('Ctrl Pts',(14.587650443,-17.080235786987,0.278663960860319));
#30703=CARTESIAN_POINT('Ctrl Pts',(15.5,-17.080235786987,0.236997294193652));
#30704=CARTESIAN_POINT('Ctrl Pts',(16.412349557,-17.080235786987,0.195330627526985));
#30705=CARTESIAN_POINT('Ctrl Pts',(16.8685243355001,-16.2901178934935,0.153663960860317));
#30706=CARTESIAN_POINT('Ctrl Pts',(17.3246991140001,-15.5,0.11199729419365));
#30707=CARTESIAN_POINT('Ctrl Pts',(16.8685243355001,-14.7098821065065,0.0703306275269832));
#30708=CARTESIAN_POINT('Ctrl Pts',(16.412349557,-13.919764213013,0.0286639608603159));
#30709=CARTESIAN_POINT('Ctrl Pts',(15.5,-13.919764213013,-0.0130027058063514));
#30710=CARTESIAN_POINT('Ctrl Pts',(14.587650443,-13.919764213013,-0.0546693724730169));
#30711=CARTESIAN_POINT('Ctrl Pts',(14.1314756644999,-14.7098821065065,-0.0963360391396842));
#30712=CARTESIAN_POINT('Ctrl Pts',(13.6753008859999,-15.5,-0.138002705806352));
#30713=CARTESIAN_POINT('Ctrl Pts',(14.1314756644999,-16.2901178934935,-0.179669372473019));
#30714=CARTESIAN_POINT('Ctrl Pts',(14.587650443,-17.080235786987,-0.221336039139686));
#30715=CARTESIAN_POINT('Ctrl Pts',(15.5,-17.080235786987,-0.263002705806354));
#30716=CARTESIAN_POINT('Ctrl Pts',(16.412349557,-17.080235786987,-0.304669372473021));
#30717=CARTESIAN_POINT('Ctrl Pts',(16.8685243355001,-16.2901178934935,-0.346336039139688));
#30718=CARTESIAN_POINT('Ctrl Pts',(17.3246991140001,-15.5,-0.388002705806356));
#30719=CARTESIAN_POINT('Ctrl Pts',(16.8685243355001,-14.7098821065065,-0.429669372473023));
#30720=CARTESIAN_POINT('Ctrl Pts',(16.412349557,-13.919764213013,-0.47133603913969));
#30721=CARTESIAN_POINT('Ctrl Pts',(15.5,-13.919764213013,-0.513002705806357));
#30722=CARTESIAN_POINT('Ctrl Pts',(14.587650443,-13.919764213013,-0.554669372473025));
#30723=CARTESIAN_POINT('Ctrl Pts',(14.1314756644999,-14.7098821065065,-0.596336039139692));
#30724=CARTESIAN_POINT('Ctrl Pts',(13.6753008859999,-15.5,-0.638002705806359));
#30725=CARTESIAN_POINT('Ctrl Pts',(14.1314756644999,-16.2901178934935,-0.679669372473027));
#30726=CARTESIAN_POINT('Ctrl Pts',(14.587650443,-17.080235786987,-0.721336039139694));
#30727=CARTESIAN_POINT('Ctrl Pts',(15.5,-17.080235786987,-0.763002705806361));
#30728=CARTESIAN_POINT('Ctrl Pts',(16.412349557,-17.080235786987,-0.804669372473029));
#30729=CARTESIAN_POINT('Ctrl Pts',(16.8685243355001,-16.2901178934935,-0.846336039139696));
#30730=CARTESIAN_POINT('Ctrl Pts',(17.3246991140001,-15.5,-0.888002705806363));
#30731=CARTESIAN_POINT('Ctrl Pts',(16.8685243355001,-14.7098821065065,-0.92966937247303));
#30732=CARTESIAN_POINT('Ctrl Pts',(16.412349557,-13.919764213013,-0.971336039139697));
#30733=CARTESIAN_POINT('Ctrl Pts',(15.5,-13.919764213013,-1.01300270580636));
#30734=CARTESIAN_POINT('Ctrl Pts',(14.587650443,-13.919764213013,-1.05466937247303));
#30735=CARTESIAN_POINT('Ctrl Pts',(14.1314756644999,-14.7098821065065,-1.0963360391397));
#30736=CARTESIAN_POINT('Ctrl Pts',(13.6753008859999,-15.5,-1.13800270580637));
#30737=CARTESIAN_POINT('Ctrl Pts',(14.1314756644999,-16.2901178934935,-1.17966937247303));
#30738=CARTESIAN_POINT('Ctrl Pts',(14.587650443,-17.080235786987,-1.2213360391397));
#30739=CARTESIAN_POINT('Ctrl Pts',(15.5,-17.080235786987,-1.26300270580637));
#30740=CARTESIAN_POINT('Ctrl Pts',(16.412349557,-17.080235786987,-1.30466937247303));
#30741=CARTESIAN_POINT('Ctrl Pts',(16.8685243355001,-16.2901178934935,-1.3463360391397));
#30742=CARTESIAN_POINT('Ctrl Pts',(17.3246991140001,-15.5,-1.38800270580637));
#30743=CARTESIAN_POINT('Ctrl Pts',(16.8685243355001,-14.7098821065065,-1.42966937247304));
#30744=CARTESIAN_POINT('Ctrl Pts',(16.412349557,-13.919764213013,-1.4713360391397));
#30745=CARTESIAN_POINT('Ctrl Pts',(15.5,-13.919764213013,-1.51300270580637));
#30746=CARTESIAN_POINT('Ctrl Pts',(14.587650443,-13.919764213013,-1.55466937247304));
#30747=CARTESIAN_POINT('Ctrl Pts',(14.1314756644999,-14.7098821065065,-1.59633603913971));
#30748=CARTESIAN_POINT('Ctrl Pts',(13.6753008859999,-15.5,-1.63800270580637));
#30749=CARTESIAN_POINT('Ctrl Pts',(14.1314756644999,-16.2901178934935,-1.67966937247304));
#30750=CARTESIAN_POINT('Ctrl Pts',(14.587650443,-17.080235786987,-1.72133603913971));
#30751=CARTESIAN_POINT('Ctrl Pts',(15.5,-17.080235786987,-1.76300270580637));
#30752=CARTESIAN_POINT('Ctrl Pts',(16.412349557,-17.080235786987,-1.80466937247304));
#30753=CARTESIAN_POINT('Ctrl Pts',(16.8685243355001,-16.2901178934935,-1.84633603913971));
#30754=CARTESIAN_POINT('Ctrl Pts',(17.3246991140001,-15.5,-1.88800270580638));
#30755=CARTESIAN_POINT('Ctrl Pts',(16.8685243355001,-14.7098821065065,-1.92966937247304));
#30756=CARTESIAN_POINT('Ctrl Pts',(16.7005762151491,-14.4189874290231,-1.94500962949244));
#30757=CARTESIAN_POINT('Ctrl Pts',(16.4288288330633,-14.2215547953296,-1.96262601180153));
#30758=CARTESIAN_POINT('',(16.4288315898516,-14.2215509627457,-1.96262324188451));
#30759=CARTESIAN_POINT('',(16.4288304039466,-14.2215500160357,-1.96262332703658));
#30760=CARTESIAN_POINT('Ctrl Pts',(14.2313898004749,-14.5577749122403,10.4122404735808));
#30761=CARTESIAN_POINT('Ctrl Pts',(14.1770441521709,-14.6309457974488,10.407829216981));
#30762=CARTESIAN_POINT('Ctrl Pts',(14.1314716057906,-14.7098797632096,10.4036666666667));
#30763=CARTESIAN_POINT('Ctrl Pts',(13.6752954743875,-15.5,10.362));
#30764=CARTESIAN_POINT('Ctrl Pts',(14.1314716057906,-16.2901202367904,10.3203333333333));
#30765=CARTESIAN_POINT('Ctrl Pts',(14.5876477371938,-17.0802404735808,10.2786666666667));
#30766=CARTESIAN_POINT('Ctrl Pts',(15.5,-17.0802404735808,10.237));
#30767=CARTESIAN_POINT('Ctrl Pts',(16.4123522628062,-17.0802404735808,10.1953333333333));
#30768=CARTESIAN_POINT('Ctrl Pts',(16.8685283942094,-16.2901202367904,10.1536666666667));
#30769=CARTESIAN_POINT('Ctrl Pts',(17.3247045256125,-15.5,10.112));
#30770=CARTESIAN_POINT('Ctrl Pts',(16.8685283942094,-14.7098797632096,10.0703333333333));
#30771=CARTESIAN_POINT('Ctrl Pts',(16.4123522628062,-13.9197595264192,10.0286666666667));
#30772=CARTESIAN_POINT('Ctrl Pts',(15.5,-13.9197595264192,9.98699999999998));
#30773=CARTESIAN_POINT('Ctrl Pts',(14.5876477371938,-13.9197595264192,9.94533333333331));
#30774=CARTESIAN_POINT('Ctrl Pts',(14.1314716057906,-14.7098797632096,9.90366666666665));
#30775=CARTESIAN_POINT('Ctrl Pts',(13.6752954743875,-15.5,9.86199999999998));
#30776=CARTESIAN_POINT('Ctrl Pts',(14.1314716057906,-16.2901202367904,9.82033333333331));
#30777=CARTESIAN_POINT('Ctrl Pts',(14.5876477371938,-17.0802404735808,9.77866666666665));
#30778=CARTESIAN_POINT('Ctrl Pts',(15.5,-17.0802404735808,9.73699999999998));
#30779=CARTESIAN_POINT('Ctrl Pts',(16.4123522628062,-17.0802404735808,9.69533333333331));
#30780=CARTESIAN_POINT('Ctrl Pts',(16.8685283942094,-16.2901202367904,9.65366666666664));
#30781=CARTESIAN_POINT('Ctrl Pts',(17.3247045256125,-15.5,9.61199999999998));
#30782=CARTESIAN_POINT('Ctrl Pts',(16.8685283942094,-14.7098797632096,9.57033333333331));
#30783=CARTESIAN_POINT('Ctrl Pts',(16.4123522628062,-13.9197595264192,9.52866666666664));
#30784=CARTESIAN_POINT('Ctrl Pts',(15.5,-13.9197595264192,9.48699999999998));
#30785=CARTESIAN_POINT('Ctrl Pts',(14.5876477371938,-13.9197595264192,9.44533333333331));
#30786=CARTESIAN_POINT('Ctrl Pts',(14.1314716057906,-14.7098797632096,9.40366666666664));
#30787=CARTESIAN_POINT('Ctrl Pts',(13.6752954743875,-15.5,9.36199999999998));
#30788=CARTESIAN_POINT('Ctrl Pts',(14.1314716057906,-16.2901202367904,9.32033333333331));
#30789=CARTESIAN_POINT('Ctrl Pts',(14.5876477371938,-17.0802404735808,9.27866666666664));
#30790=CARTESIAN_POINT('Ctrl Pts',(15.5,-17.0802404735808,9.23699999999997));
#30791=CARTESIAN_POINT('Ctrl Pts',(16.4123522628062,-17.0802404735808,9.19533333333331));
#30792=CARTESIAN_POINT('Ctrl Pts',(16.8685283942094,-16.2901202367904,9.15366666666664));
#30793=CARTESIAN_POINT('Ctrl Pts',(17.3247045256125,-15.5,9.11199999999997));
#30794=CARTESIAN_POINT('Ctrl Pts',(16.8685283942094,-14.7098797632096,9.0703333333333));
#30795=CARTESIAN_POINT('Ctrl Pts',(16.4123522628062,-13.9197595264192,9.02866666666664));
#30796=CARTESIAN_POINT('Ctrl Pts',(15.5,-13.9197595264192,8.98699999999997));
#30797=CARTESIAN_POINT('Ctrl Pts',(14.5876477371938,-13.9197595264192,8.9453333333333));
#30798=CARTESIAN_POINT('Ctrl Pts',(14.1314716057906,-14.7098797632096,8.90366666666664));
#30799=CARTESIAN_POINT('Ctrl Pts',(13.6752954743875,-15.5,8.86199999999997));
#30800=CARTESIAN_POINT('Ctrl Pts',(14.1314716057906,-16.2901202367904,8.8203333333333));
#30801=CARTESIAN_POINT('Ctrl Pts',(14.5876477371938,-17.0802404735808,8.77866666666663));
#30802=CARTESIAN_POINT('Ctrl Pts',(15.5,-17.0802404735808,8.73699999999997));
#30803=CARTESIAN_POINT('Ctrl Pts',(16.4123522628062,-17.0802404735808,8.6953333333333));
#30804=CARTESIAN_POINT('Ctrl Pts',(16.8685283942094,-16.2901202367904,8.65366666666663));
#30805=CARTESIAN_POINT('Ctrl Pts',(17.3247045256125,-15.5,8.61199999999996));
#30806=CARTESIAN_POINT('Ctrl Pts',(16.8685283942094,-14.7098797632096,8.57033333333329));
#30807=CARTESIAN_POINT('Ctrl Pts',(16.4123522628062,-13.9197595264192,8.52866666666663));
#30808=CARTESIAN_POINT('Ctrl Pts',(15.5,-13.9197595264192,8.48699999999996));
#30809=CARTESIAN_POINT('Ctrl Pts',(14.5876477371938,-13.9197595264192,8.44533333333329));
#30810=CARTESIAN_POINT('Ctrl Pts',(14.1314716057906,-14.7098797632096,8.40366666666663));
#30811=CARTESIAN_POINT('Ctrl Pts',(13.6752954743875,-15.5,8.36199999999996));
#30812=CARTESIAN_POINT('Ctrl Pts',(14.1314716057906,-16.2901202367904,8.32033333333329));
#30813=CARTESIAN_POINT('Ctrl Pts',(14.5876477371938,-17.0802404735808,8.27866666666663));
#30814=CARTESIAN_POINT('Ctrl Pts',(15.5,-17.0802404735808,8.23699999999996));
#30815=CARTESIAN_POINT('Ctrl Pts',(16.4123522628062,-17.0802404735808,8.19533333333329));
#30816=CARTESIAN_POINT('Ctrl Pts',(16.8685283942094,-16.2901202367904,8.15366666666663));
#30817=CARTESIAN_POINT('Ctrl Pts',(17.3247045256125,-15.5,8.11199999999996));
#30818=CARTESIAN_POINT('Ctrl Pts',(16.8685283942094,-14.7098797632096,8.07033333333329));
#30819=CARTESIAN_POINT('Ctrl Pts',(16.4123522628062,-13.9197595264192,8.02866666666662));
#30820=CARTESIAN_POINT('Ctrl Pts',(15.5,-13.9197595264192,7.98699999999996));
#30821=CARTESIAN_POINT('Ctrl Pts',(14.5876477371938,-13.9197595264192,7.94533333333329));
#30822=CARTESIAN_POINT('Ctrl Pts',(14.1314716057906,-14.7098797632096,7.90366666666662));
#30823=CARTESIAN_POINT('Ctrl Pts',(13.6752954743875,-15.5,7.86199999999995));
#30824=CARTESIAN_POINT('Ctrl Pts',(14.1314716057906,-16.2901202367904,7.82033333333329));
#30825=CARTESIAN_POINT('Ctrl Pts',(14.5876477371938,-17.0802404735808,7.77866666666662));
#30826=CARTESIAN_POINT('Ctrl Pts',(15.5,-17.0802404735808,7.73699999999995));
#30827=CARTESIAN_POINT('Ctrl Pts',(16.4123522628062,-17.0802404735808,7.69533333333329));
#30828=CARTESIAN_POINT('Ctrl Pts',(16.8685283942094,-16.2901202367904,7.65366666666662));
#30829=CARTESIAN_POINT('Ctrl Pts',(17.3247045256125,-15.5,7.61199999999995));
#30830=CARTESIAN_POINT('Ctrl Pts',(16.8685283942094,-14.7098797632096,7.57033333333328));
#30831=CARTESIAN_POINT('Ctrl Pts',(16.4123522628062,-13.9197595264192,7.52866666666662));
#30832=CARTESIAN_POINT('Ctrl Pts',(15.5,-13.9197595264192,7.48699999999995));
#30833=CARTESIAN_POINT('Ctrl Pts',(14.5876477371938,-13.9197595264192,7.44533333333328));
#30834=CARTESIAN_POINT('Ctrl Pts',(14.1314716057906,-14.7098797632096,7.40366666666661));
#30835=CARTESIAN_POINT('Ctrl Pts',(13.6752954743875,-15.5,7.36199999999995));
#30836=CARTESIAN_POINT('Ctrl Pts',(14.1314716057906,-16.2901202367904,7.32033333333328));
#30837=CARTESIAN_POINT('Ctrl Pts',(14.5876477371938,-17.0802404735808,7.27866666666661));
#30838=CARTESIAN_POINT('Ctrl Pts',(15.5,-17.0802404735808,7.23699999999995));
#30839=CARTESIAN_POINT('Ctrl Pts',(16.4123522628062,-17.0802404735808,7.19533333333328));
#30840=CARTESIAN_POINT('Ctrl Pts',(16.8685283942094,-16.2901202367904,7.15366666666661));
#30841=CARTESIAN_POINT('Ctrl Pts',(17.3247045256125,-15.5,7.11199999999994));
#30842=CARTESIAN_POINT('Ctrl Pts',(16.8685283942094,-14.7098797632096,7.07033333333328));
#30843=CARTESIAN_POINT('Ctrl Pts',(16.4123522628062,-13.9197595264192,7.02866666666661));
#30844=CARTESIAN_POINT('Ctrl Pts',(15.5,-13.9197595264192,6.98699999999994));
#30845=CARTESIAN_POINT('Ctrl Pts',(14.5876477371938,-13.9197595264192,6.94533333333327));
#30846=CARTESIAN_POINT('Ctrl Pts',(14.1314716057906,-14.7098797632096,6.90366666666661));
#30847=CARTESIAN_POINT('Ctrl Pts',(13.6752954743875,-15.5,6.86199999999994));
#30848=CARTESIAN_POINT('Ctrl Pts',(14.1314716057906,-16.2901202367904,6.82033333333327));
#30849=CARTESIAN_POINT('Ctrl Pts',(14.5876477371938,-17.0802404735808,6.77866666666661));
#30850=CARTESIAN_POINT('Ctrl Pts',(15.5,-17.0802404735808,6.73699999999994));
#30851=CARTESIAN_POINT('Ctrl Pts',(16.4123522628062,-17.0802404735808,6.69533333333327));
#30852=CARTESIAN_POINT('Ctrl Pts',(16.8685283942094,-16.2901202367904,6.65366666666661));
#30853=CARTESIAN_POINT('Ctrl Pts',(17.3247045256125,-15.5,6.61199999999994));
#30854=CARTESIAN_POINT('Ctrl Pts',(16.8685283942094,-14.7098797632096,6.57033333333327));
#30855=CARTESIAN_POINT('Ctrl Pts',(16.4123522628062,-13.9197595264192,6.5286666666666));
#30856=CARTESIAN_POINT('Ctrl Pts',(15.5,-13.9197595264192,6.48699999999994));
#30857=CARTESIAN_POINT('Ctrl Pts',(14.5876477371938,-13.9197595264192,6.44533333333327));
#30858=CARTESIAN_POINT('Ctrl Pts',(14.1314716057906,-14.7098797632096,6.4036666666666));
#30859=CARTESIAN_POINT('Ctrl Pts',(13.6752954743875,-15.5,6.36199999999993));
#30860=CARTESIAN_POINT('Ctrl Pts',(14.1314716057906,-16.2901202367904,6.32033333333327));
#30861=CARTESIAN_POINT('Ctrl Pts',(14.5876477371938,-17.0802404735808,6.2786666666666));
#30862=CARTESIAN_POINT('Ctrl Pts',(15.5,-17.0802404735808,6.23699999999993));
#30863=CARTESIAN_POINT('Ctrl Pts',(16.4123522628062,-17.0802404735808,6.19533333333326));
#30864=CARTESIAN_POINT('Ctrl Pts',(16.8685283942094,-16.2901202367904,6.1536666666666));
#30865=CARTESIAN_POINT('Ctrl Pts',(17.3247045256125,-15.5,6.11199999999993));
#30866=CARTESIAN_POINT('Ctrl Pts',(16.8685283942094,-14.7098797632096,6.07033333333326));
#30867=CARTESIAN_POINT('Ctrl Pts',(16.4123522628062,-13.9197595264192,6.0286666666666));
#30868=CARTESIAN_POINT('Ctrl Pts',(15.5,-13.9197595264192,5.98699999999993));
#30869=CARTESIAN_POINT('Ctrl Pts',(14.5876477371938,-13.9197595264192,5.94533333333326));
#30870=CARTESIAN_POINT('Ctrl Pts',(14.1314716057906,-14.7098797632096,5.9036666666666));
#30871=CARTESIAN_POINT('Ctrl Pts',(13.6752954743875,-15.5,5.86199999999993));
#30872=CARTESIAN_POINT('Ctrl Pts',(14.1314716057906,-16.2901202367904,5.82033333333326));
#30873=CARTESIAN_POINT('Ctrl Pts',(14.5876477371938,-17.0802404735808,5.77866666666659));
#30874=CARTESIAN_POINT('Ctrl Pts',(15.5,-17.0802404735808,5.73699999999993));
#30875=CARTESIAN_POINT('Ctrl Pts',(16.4123522628062,-17.0802404735808,5.69533333333326));
#30876=CARTESIAN_POINT('Ctrl Pts',(16.8685283942094,-16.2901202367904,5.65366666666659));
#30877=CARTESIAN_POINT('Ctrl Pts',(17.3247045256125,-15.5,5.61199999999992));
#30878=CARTESIAN_POINT('Ctrl Pts',(16.8685283942094,-14.7098797632096,5.57033333333326));
#30879=CARTESIAN_POINT('Ctrl Pts',(16.4123522628062,-13.9197595264192,5.52866666666659));
#30880=CARTESIAN_POINT('Ctrl Pts',(15.5,-13.9197595264192,5.48699999999992));
#30881=CARTESIAN_POINT('Ctrl Pts',(14.5876477371938,-13.9197595264192,5.44533333333326));
#30882=CARTESIAN_POINT('Ctrl Pts',(14.1314716057906,-14.7098797632096,5.40366666666659));
#30883=CARTESIAN_POINT('Ctrl Pts',(13.6752954743875,-15.5,5.36199999999992));
#30884=CARTESIAN_POINT('Ctrl Pts',(14.1314716057906,-16.2901202367904,5.32033333333325));
#30885=CARTESIAN_POINT('Ctrl Pts',(14.5876477371938,-17.0802404735808,5.27866666666659));
#30886=CARTESIAN_POINT('Ctrl Pts',(15.5,-17.0802404735808,5.23699999999992));
#30887=CARTESIAN_POINT('Ctrl Pts',(16.4123522628062,-17.0802404735808,5.19533333333325));
#30888=CARTESIAN_POINT('Ctrl Pts',(16.8685283942094,-16.2901202367904,5.15366666666658));
#30889=CARTESIAN_POINT('Ctrl Pts',(17.3247045256125,-15.5,5.11199999999992));
#30890=CARTESIAN_POINT('Ctrl Pts',(16.8685283942094,-14.7098797632096,5.07033333333325));
#30891=CARTESIAN_POINT('Ctrl Pts',(16.4123522628062,-13.9197595264192,5.02866666666658));
#30892=CARTESIAN_POINT('Ctrl Pts',(15.5,-13.9197595264192,4.98699999999992));
#30893=CARTESIAN_POINT('Ctrl Pts',(14.5876477371938,-13.9197595264192,4.94533333333325));
#30894=CARTESIAN_POINT('Ctrl Pts',(14.1314716057906,-14.7098797632096,4.90366666666658));
#30895=CARTESIAN_POINT('Ctrl Pts',(13.6752954743875,-15.5,4.86199999999991));
#30896=CARTESIAN_POINT('Ctrl Pts',(14.1314716057906,-16.2901202367904,4.82033333333325));
#30897=CARTESIAN_POINT('Ctrl Pts',(14.5876477371938,-17.0802404735808,4.77866666666658));
#30898=CARTESIAN_POINT('Ctrl Pts',(15.5,-17.0802404735808,4.73699999999991));
#30899=CARTESIAN_POINT('Ctrl Pts',(16.4123522628062,-17.0802404735808,4.69533333333325));
#30900=CARTESIAN_POINT('Ctrl Pts',(16.8685283942094,-16.2901202367904,4.65366666666658));
#30901=CARTESIAN_POINT('Ctrl Pts',(17.3247045256125,-15.5,4.61199999999991));
#30902=CARTESIAN_POINT('Ctrl Pts',(16.8685283942094,-14.7098797632096,4.57033333333324));
#30903=CARTESIAN_POINT('Ctrl Pts',(16.4123522628062,-13.9197595264192,4.52866666666658));
#30904=CARTESIAN_POINT('Ctrl Pts',(15.5,-13.9197595264192,4.48699999999991));
#30905=CARTESIAN_POINT('Ctrl Pts',(14.5876477371938,-13.9197595264192,4.44533333333324));
#30906=CARTESIAN_POINT('Ctrl Pts',(14.1314716057906,-14.7098797632096,4.40366666666658));
#30907=CARTESIAN_POINT('Ctrl Pts',(13.6752954743875,-15.5,4.36199999999991));
#30908=CARTESIAN_POINT('Ctrl Pts',(14.1314716057906,-16.2901202367904,4.32033333333324));
#30909=CARTESIAN_POINT('Ctrl Pts',(14.5876477371938,-17.0802404735808,4.27866666666657));
#30910=CARTESIAN_POINT('Ctrl Pts',(15.5,-17.0802404735808,4.23699999999991));
#30911=CARTESIAN_POINT('Ctrl Pts',(16.4123522628062,-17.0802404735808,4.19533333333324));
#30912=CARTESIAN_POINT('Ctrl Pts',(16.8685283942094,-16.2901202367904,4.15366666666657));
#30913=CARTESIAN_POINT('Ctrl Pts',(17.3247045256125,-15.5,4.1119999999999));
#30914=CARTESIAN_POINT('Ctrl Pts',(16.8685283942094,-14.7098797632096,4.07033333333324));
#30915=CARTESIAN_POINT('Ctrl Pts',(16.4123522628062,-13.9197595264192,4.02866666666657));
#30916=CARTESIAN_POINT('Ctrl Pts',(15.5,-13.9197595264192,3.9869999999999));
#30917=CARTESIAN_POINT('Ctrl Pts',(14.5876477371938,-13.9197595264192,3.94533333333323));
#30918=CARTESIAN_POINT('Ctrl Pts',(14.1314716057906,-14.7098797632096,3.90366666666657));
#30919=CARTESIAN_POINT('Ctrl Pts',(13.6752954743875,-15.5,3.8619999999999));
#30920=CARTESIAN_POINT('Ctrl Pts',(14.1314716057906,-16.2901202367904,3.82033333333323));
#30921=CARTESIAN_POINT('Ctrl Pts',(14.5876477371938,-17.0802404735808,3.77866666666657));
#30922=CARTESIAN_POINT('Ctrl Pts',(15.5,-17.0802404735808,3.7369999999999));
#30923=CARTESIAN_POINT('Ctrl Pts',(16.4123522628062,-17.0802404735808,3.69533333333323));
#30924=CARTESIAN_POINT('Ctrl Pts',(16.8685283942094,-16.2901202367904,3.65366666666656));
#30925=CARTESIAN_POINT('Ctrl Pts',(17.3247045256125,-15.5,3.6119999999999));
#30926=CARTESIAN_POINT('Ctrl Pts',(16.8685283942094,-14.7098797632096,3.57033333333323));
#30927=CARTESIAN_POINT('Ctrl Pts',(16.4123522628062,-13.9197595264192,3.52866666666656));
#30928=CARTESIAN_POINT('Ctrl Pts',(15.5,-13.9197595264192,3.4869999999999));
#30929=CARTESIAN_POINT('Ctrl Pts',(14.5876477371938,-13.9197595264192,3.44533333333323));
#30930=CARTESIAN_POINT('Ctrl Pts',(14.1314716057906,-14.7098797632096,3.40366666666656));
#30931=CARTESIAN_POINT('Ctrl Pts',(13.6752954743875,-15.5,3.36199999999989));
#30932=CARTESIAN_POINT('Ctrl Pts',(14.1314716057906,-16.2901202367904,3.32033333333323));
#30933=CARTESIAN_POINT('Ctrl Pts',(14.5876477371938,-17.0802404735808,3.27866666666656));
#30934=CARTESIAN_POINT('Ctrl Pts',(15.5,-17.0802404735808,3.23699999999989));
#30935=CARTESIAN_POINT('Ctrl Pts',(16.4123522628062,-17.0802404735808,3.19533333333323));
#30936=CARTESIAN_POINT('Ctrl Pts',(16.8685283942094,-16.2901202367904,3.15366666666656));
#30937=CARTESIAN_POINT('Ctrl Pts',(17.3247045256125,-15.5,3.11199999999989));
#30938=CARTESIAN_POINT('Ctrl Pts',(16.8685283942094,-14.7098797632096,3.07033333333322));
#30939=CARTESIAN_POINT('Ctrl Pts',(16.4123522628062,-13.9197595264192,3.02866666666656));
#30940=CARTESIAN_POINT('Ctrl Pts',(15.5,-13.9197595264192,2.98699999999989));
#30941=CARTESIAN_POINT('Ctrl Pts',(14.5876477371938,-13.9197595264192,2.94533333333322));
#30942=CARTESIAN_POINT('Ctrl Pts',(14.1314716057906,-14.7098797632096,2.90366666666656));
#30943=CARTESIAN_POINT('Ctrl Pts',(13.6752954743875,-15.5,2.86199999999989));
#30944=CARTESIAN_POINT('Ctrl Pts',(14.1314716057906,-16.2901202367904,2.82033333333322));
#30945=CARTESIAN_POINT('Ctrl Pts',(14.5876477371938,-17.0802404735808,2.77866666666655));
#30946=CARTESIAN_POINT('Ctrl Pts',(15.5,-17.0802404735808,2.73699999999989));
#30947=CARTESIAN_POINT('Ctrl Pts',(16.4123522628062,-17.0802404735808,2.69533333333322));
#30948=CARTESIAN_POINT('Ctrl Pts',(16.8685283942094,-16.2901202367904,2.65366666666655));
#30949=CARTESIAN_POINT('Ctrl Pts',(17.3247045256125,-15.5,2.61199999999988));
#30950=CARTESIAN_POINT('Ctrl Pts',(16.8685283942094,-14.7098797632096,2.57033333333322));
#30951=CARTESIAN_POINT('Ctrl Pts',(16.4123522628062,-13.9197595264192,2.52866666666655));
#30952=CARTESIAN_POINT('Ctrl Pts',(15.5,-13.9197595264192,2.48699999999988));
#30953=CARTESIAN_POINT('Ctrl Pts',(14.5876477371938,-13.9197595264192,2.44533333333321));
#30954=CARTESIAN_POINT('Ctrl Pts',(14.1314716057906,-14.7098797632096,2.40366666666655));
#30955=CARTESIAN_POINT('Ctrl Pts',(13.6752954743875,-15.5,2.36199999999988));
#30956=CARTESIAN_POINT('Ctrl Pts',(14.1314716057906,-16.2901202367904,2.32033333333321));
#30957=CARTESIAN_POINT('Ctrl Pts',(14.5876477371938,-17.0802404735808,2.27866666666655));
#30958=CARTESIAN_POINT('Ctrl Pts',(15.5,-17.0802404735808,2.23699999999988));
#30959=CARTESIAN_POINT('Ctrl Pts',(16.4123522628062,-17.0802404735808,2.19533333333321));
#30960=CARTESIAN_POINT('Ctrl Pts',(16.8685283942094,-16.2901202367904,2.15366666666655));
#30961=CARTESIAN_POINT('Ctrl Pts',(17.3247045256125,-15.5,2.11199999999988));
#30962=CARTESIAN_POINT('Ctrl Pts',(16.8685283942094,-14.7098797632096,2.07033333333321));
#30963=CARTESIAN_POINT('Ctrl Pts',(16.4123522628062,-13.9197595264192,2.02866666666654));
#30964=CARTESIAN_POINT('Ctrl Pts',(15.5,-13.9197595264192,1.98699999999988));
#30965=CARTESIAN_POINT('Ctrl Pts',(14.5876477371938,-13.9197595264192,1.94533333333321));
#30966=CARTESIAN_POINT('Ctrl Pts',(14.1314716057906,-14.7098797632096,1.90366666666654));
#30967=CARTESIAN_POINT('Ctrl Pts',(13.6752954743875,-15.5,1.86199999999987));
#30968=CARTESIAN_POINT('Ctrl Pts',(14.1314716057906,-16.2901202367904,1.82033333333321));
#30969=CARTESIAN_POINT('Ctrl Pts',(14.5876477371938,-17.0802404735808,1.77866666666654));
#30970=CARTESIAN_POINT('Ctrl Pts',(15.5,-17.0802404735808,1.73699999999987));
#30971=CARTESIAN_POINT('Ctrl Pts',(16.4123522628062,-17.0802404735808,1.6953333333332));
#30972=CARTESIAN_POINT('Ctrl Pts',(16.8685283942094,-16.2901202367904,1.65366666666654));
#30973=CARTESIAN_POINT('Ctrl Pts',(17.3247045256125,-15.5,1.61199999999987));
#30974=CARTESIAN_POINT('Ctrl Pts',(16.8685283942094,-14.7098797632096,1.5703333333332));
#30975=CARTESIAN_POINT('Ctrl Pts',(16.4123522628062,-13.9197595264192,1.52866666666654));
#30976=CARTESIAN_POINT('Ctrl Pts',(15.5,-13.9197595264192,1.48699999999987));
#30977=CARTESIAN_POINT('Ctrl Pts',(14.5876477371938,-13.9197595264192,1.4453333333332));
#30978=CARTESIAN_POINT('Ctrl Pts',(14.1314716057906,-14.7098797632096,1.40366666666653));
#30979=CARTESIAN_POINT('Ctrl Pts',(13.6752954743875,-15.5,1.36199999999987));
#30980=CARTESIAN_POINT('Ctrl Pts',(14.1314716057906,-16.2901202367904,1.3203333333332));
#30981=CARTESIAN_POINT('Ctrl Pts',(14.5876477371938,-17.0802404735808,1.27866666666653));
#30982=CARTESIAN_POINT('Ctrl Pts',(15.5,-17.0802404735808,1.23699999999987));
#30983=CARTESIAN_POINT('Ctrl Pts',(16.4123522628062,-17.0802404735808,1.1953333333332));
#30984=CARTESIAN_POINT('Ctrl Pts',(16.8685283942094,-16.2901202367904,1.15366666666653));
#30985=CARTESIAN_POINT('Ctrl Pts',(17.3247045256125,-15.5,1.11199999999986));
#30986=CARTESIAN_POINT('Ctrl Pts',(16.8685283942094,-14.7098797632096,1.0703333333332));
#30987=CARTESIAN_POINT('Ctrl Pts',(16.4123522628062,-13.9197595264192,1.02866666666653));
#30988=CARTESIAN_POINT('Ctrl Pts',(15.5,-13.9197595264192,0.986999999999863));
#30989=CARTESIAN_POINT('Ctrl Pts',(14.5876477371938,-13.9197595264192,0.945333333333196));
#30990=CARTESIAN_POINT('Ctrl Pts',(14.1314716057906,-14.7098797632096,0.903666666666529));
#30991=CARTESIAN_POINT('Ctrl Pts',(13.6752954743875,-15.5,0.861999999999861));
#30992=CARTESIAN_POINT('Ctrl Pts',(14.1314716057906,-16.2901202367904,0.820333333333194));
#30993=CARTESIAN_POINT('Ctrl Pts',(14.5876477371938,-17.0802404735808,0.778666666666527));
#30994=CARTESIAN_POINT('Ctrl Pts',(15.5,-17.0802404735808,0.736999999999859));
#30995=CARTESIAN_POINT('Ctrl Pts',(16.4123522628062,-17.0802404735808,0.695333333333192));
#30996=CARTESIAN_POINT('Ctrl Pts',(16.8685283942094,-16.2901202367904,0.653666666666525));
#30997=CARTESIAN_POINT('Ctrl Pts',(17.3247045256125,-15.5,0.611999999999858));
#30998=CARTESIAN_POINT('Ctrl Pts',(16.8685283942094,-14.7098797632096,0.57033333333319));
#30999=CARTESIAN_POINT('Ctrl Pts',(16.4123522628062,-13.9197595264192,0.528666666666523));
#31000=CARTESIAN_POINT('Ctrl Pts',(15.5,-13.9197595264192,0.486999999999856));
#31001=CARTESIAN_POINT('Ctrl Pts',(14.5876477371938,-13.9197595264192,0.445333333333188));
#31002=CARTESIAN_POINT('Ctrl Pts',(14.1314716057906,-14.7098797632096,0.403666666666521));
#31003=CARTESIAN_POINT('Ctrl Pts',(13.6752954743875,-15.5,0.361999999999854));
#31004=CARTESIAN_POINT('Ctrl Pts',(14.1314716057906,-16.2901202367904,0.320333333333186));
#31005=CARTESIAN_POINT('Ctrl Pts',(14.5876477371938,-17.0802404735808,0.278666666666519));
#31006=CARTESIAN_POINT('Ctrl Pts',(15.5,-17.0802404735808,0.236999999999852));
#31007=CARTESIAN_POINT('Ctrl Pts',(16.4123522628062,-17.0802404735808,0.195333333333185));
#31008=CARTESIAN_POINT('Ctrl Pts',(16.8685283942094,-16.2901202367904,0.153666666666517));
#31009=CARTESIAN_POINT('Ctrl Pts',(17.3247045256125,-15.5,0.11199999999985));
#31010=CARTESIAN_POINT('Ctrl Pts',(16.8685283942094,-14.7098797632096,0.0703333333331828));
#31011=CARTESIAN_POINT('Ctrl Pts',(16.4123522628062,-13.9197595264192,0.0286666666665155));
#31012=CARTESIAN_POINT('Ctrl Pts',(15.5,-13.9197595264192,-0.0130000000001518));
#31013=CARTESIAN_POINT('Ctrl Pts',(14.5876477371938,-13.9197595264192,-0.0546666666668173));
#31014=CARTESIAN_POINT('Ctrl Pts',(14.1314716057906,-14.7098797632096,-0.0963333333334846));
#31015=CARTESIAN_POINT('Ctrl Pts',(13.6752954743875,-15.5,-0.138000000000152));
#31016=CARTESIAN_POINT('Ctrl Pts',(14.1314716057906,-16.2901202367904,-0.179666666666819));
#31017=CARTESIAN_POINT('Ctrl Pts',(14.5876477371938,-17.0802404735808,-0.221333333333486));
#31018=CARTESIAN_POINT('Ctrl Pts',(15.5,-17.0802404735808,-0.263000000000154));
#31019=CARTESIAN_POINT('Ctrl Pts',(16.4123522628062,-17.0802404735808,-0.304666666666821));
#31020=CARTESIAN_POINT('Ctrl Pts',(16.8685283942094,-16.2901202367904,-0.346333333333488));
#31021=CARTESIAN_POINT('Ctrl Pts',(17.3247045256125,-15.5,-0.388000000000156));
#31022=CARTESIAN_POINT('Ctrl Pts',(16.8685283942094,-14.7098797632096,-0.429666666666823));
#31023=CARTESIAN_POINT('Ctrl Pts',(16.4123522628062,-13.9197595264192,-0.47133333333349));
#31024=CARTESIAN_POINT('Ctrl Pts',(15.5,-13.9197595264192,-0.513000000000157));
#31025=CARTESIAN_POINT('Ctrl Pts',(14.5876477371938,-13.9197595264192,-0.554666666666825));
#31026=CARTESIAN_POINT('Ctrl Pts',(14.1314716057906,-14.7098797632096,-0.596333333333492));
#31027=CARTESIAN_POINT('Ctrl Pts',(13.6752954743875,-15.5,-0.638000000000159));
#31028=CARTESIAN_POINT('Ctrl Pts',(14.1314716057906,-16.2901202367904,-0.679666666666827));
#31029=CARTESIAN_POINT('Ctrl Pts',(14.5876477371938,-17.0802404735808,-0.721333333333494));
#31030=CARTESIAN_POINT('Ctrl Pts',(15.5,-17.0802404735808,-0.763000000000161));
#31031=CARTESIAN_POINT('Ctrl Pts',(16.4123522628062,-17.0802404735808,-0.804666666666829));
#31032=CARTESIAN_POINT('Ctrl Pts',(16.8685283942094,-16.2901202367904,-0.846333333333496));
#31033=CARTESIAN_POINT('Ctrl Pts',(17.3247045256125,-15.5,-0.888000000000163));
#31034=CARTESIAN_POINT('Ctrl Pts',(16.8685283942094,-14.7098797632096,-0.92966666666683));
#31035=CARTESIAN_POINT('Ctrl Pts',(16.4123522628062,-13.9197595264192,-0.971333333333498));
#31036=CARTESIAN_POINT('Ctrl Pts',(15.5,-13.9197595264192,-1.01300000000016));
#31037=CARTESIAN_POINT('Ctrl Pts',(14.5876477371938,-13.9197595264192,-1.05466666666683));
#31038=CARTESIAN_POINT('Ctrl Pts',(14.1314716057906,-14.7098797632096,-1.0963333333335));
#31039=CARTESIAN_POINT('Ctrl Pts',(13.6752954743875,-15.5,-1.13800000000017));
#31040=CARTESIAN_POINT('Ctrl Pts',(14.1314716057906,-16.2901202367904,-1.17966666666683));
#31041=CARTESIAN_POINT('Ctrl Pts',(14.5876477371938,-17.0802404735808,-1.2213333333335));
#31042=CARTESIAN_POINT('Ctrl Pts',(15.5,-17.0802404735808,-1.26300000000017));
#31043=CARTESIAN_POINT('Ctrl Pts',(16.4123522628062,-17.0802404735808,-1.30466666666683));
#31044=CARTESIAN_POINT('Ctrl Pts',(16.8685283942094,-16.2901202367904,-1.3463333333335));
#31045=CARTESIAN_POINT('Ctrl Pts',(17.3247045256125,-15.5,-1.38800000000017));
#31046=CARTESIAN_POINT('Ctrl Pts',(16.8685283942094,-14.7098797632096,-1.42966666666684));
#31047=CARTESIAN_POINT('Ctrl Pts',(16.4123522628062,-13.9197595264192,-1.4713333333335));
#31048=CARTESIAN_POINT('Ctrl Pts',(15.5,-13.9197595264192,-1.51300000000017));
#31049=CARTESIAN_POINT('Ctrl Pts',(14.5876477371938,-13.9197595264192,-1.55466666666684));
#31050=CARTESIAN_POINT('Ctrl Pts',(14.1314716057906,-14.7098797632096,-1.59633333333351));
#31051=CARTESIAN_POINT('Ctrl Pts',(13.6752954743875,-15.5,-1.63800000000017));
#31052=CARTESIAN_POINT('Ctrl Pts',(14.1314716057906,-16.2901202367904,-1.67966666666684));
#31053=CARTESIAN_POINT('Ctrl Pts',(14.5876477371938,-17.0802404735808,-1.72133333333351));
#31054=CARTESIAN_POINT('Ctrl Pts',(15.5,-17.0802404735808,-1.76300000000017));
#31055=CARTESIAN_POINT('Ctrl Pts',(16.4123522628062,-17.0802404735808,-1.80466666666684));
#31056=CARTESIAN_POINT('Ctrl Pts',(16.8685283942094,-16.2901202367904,-1.84633333333351));
#31057=CARTESIAN_POINT('Ctrl Pts',(17.3247045256125,-15.5,-1.88800000000018));
#31058=CARTESIAN_POINT('Ctrl Pts',(16.8685283942094,-14.7098797632096,-1.92966666666684));
#31059=CARTESIAN_POINT('Ctrl Pts',(16.700583153372,-14.4189900731899,-1.94500661517905));
#31060=CARTESIAN_POINT('Ctrl Pts',(16.4288340223699,-14.2215527726061,-1.96262314816781));
#31061=CARTESIAN_POINT('Origin',(16.5839252605846,-14.0080754615186,-2.17746715486548));
#31062=CARTESIAN_POINT('',(16.4288300625788,-14.2215498957104,-2.02512301642216));
#31063=CARTESIAN_POINT('Ctrl Pts',(15.5,-17.0802404735808,11.2370201234482));
#31064=CARTESIAN_POINT('Ctrl Pts',(16.4123522628062,-17.0802404735808,11.1953534567815));
#31065=CARTESIAN_POINT('Ctrl Pts',(16.8685283942094,-16.2901202367904,11.1536867901149));
#31066=CARTESIAN_POINT('Ctrl Pts',(17.3247045256125,-15.5,11.1120201234482));
#31067=CARTESIAN_POINT('Ctrl Pts',(16.8685283942094,-14.7098797632096,11.0703534567815));
#31068=CARTESIAN_POINT('Ctrl Pts',(16.4123522628062,-13.9197595264192,11.0286867901149));
#31069=CARTESIAN_POINT('Ctrl Pts',(15.5,-13.9197595264192,10.9870201234482));
#31070=CARTESIAN_POINT('Ctrl Pts',(14.5876477371938,-13.9197595264192,10.9453534567815));
#31071=CARTESIAN_POINT('Ctrl Pts',(14.1314716057906,-14.7098797632096,10.9036867901149));
#31072=CARTESIAN_POINT('Ctrl Pts',(13.6752954743875,-15.5,10.8620201234482));
#31073=CARTESIAN_POINT('Ctrl Pts',(14.1314716057906,-16.2901202367904,10.8203534567815));
#31074=CARTESIAN_POINT('Ctrl Pts',(14.5876477371938,-17.0802404735808,10.7786867901149));
#31075=CARTESIAN_POINT('Ctrl Pts',(15.5,-17.0802404735808,10.7370201234482));
#31076=CARTESIAN_POINT('Ctrl Pts',(16.4123522628062,-17.0802404735808,10.6953534567815));
#31077=CARTESIAN_POINT('Ctrl Pts',(16.8685283942094,-16.2901202367904,10.6536867901149));
#31078=CARTESIAN_POINT('Ctrl Pts',(17.3247045256125,-15.5,10.6120201234482));
#31079=CARTESIAN_POINT('Ctrl Pts',(16.8685283942094,-14.7098797632096,10.5703534567815));
#31080=CARTESIAN_POINT('Ctrl Pts',(16.4123522628062,-13.9197595264192,10.5286867901149));
#31081=CARTESIAN_POINT('Ctrl Pts',(15.5,-13.9197595264192,10.4870201234482));
#31082=CARTESIAN_POINT('Ctrl Pts',(14.5876477371938,-13.9197595264192,10.4453534567815));
#31083=CARTESIAN_POINT('Ctrl Pts',(14.1314716057906,-14.7098797632096,10.4036867901149));
#31084=CARTESIAN_POINT('Ctrl Pts',(13.6752954743875,-15.5,10.3620201234482));
#31085=CARTESIAN_POINT('Ctrl Pts',(14.1314716057906,-16.2901202367904,10.3203534567815));
#31086=CARTESIAN_POINT('Ctrl Pts',(14.5876477371938,-17.0802404735808,10.2786867901149));
#31087=CARTESIAN_POINT('Ctrl Pts',(15.5,-17.0802404735808,10.2370201234482));
#31088=CARTESIAN_POINT('Ctrl Pts',(16.4123522628062,-17.0802404735808,10.1953534567815));
#31089=CARTESIAN_POINT('Ctrl Pts',(16.8685283942094,-16.2901202367904,10.1536867901149));
#31090=CARTESIAN_POINT('Ctrl Pts',(17.3247045256125,-15.5,10.1120201234482));
#31091=CARTESIAN_POINT('Ctrl Pts',(16.8685283942094,-14.7098797632096,10.0703534567815));
#31092=CARTESIAN_POINT('Ctrl Pts',(16.4123522628062,-13.9197595264192,10.0286867901149));
#31093=CARTESIAN_POINT('Ctrl Pts',(15.5,-13.9197595264192,9.98702012344819));
#31094=CARTESIAN_POINT('Ctrl Pts',(14.5876477371938,-13.9197595264192,9.94535345678152));
#31095=CARTESIAN_POINT('Ctrl Pts',(14.1314716057906,-14.7098797632096,9.90368679011485));
#31096=CARTESIAN_POINT('Ctrl Pts',(13.6752954743875,-15.5,9.86202012344818));
#31097=CARTESIAN_POINT('Ctrl Pts',(14.1314716057906,-16.2901202367904,9.82035345678151));
#31098=CARTESIAN_POINT('Ctrl Pts',(14.5876477371938,-17.0802404735808,9.77868679011485));
#31099=CARTESIAN_POINT('Ctrl Pts',(15.5,-17.0802404735808,9.73702012344818));
#31100=CARTESIAN_POINT('Ctrl Pts',(16.4123522628062,-17.0802404735808,9.69535345678151));
#31101=CARTESIAN_POINT('Ctrl Pts',(16.8685283942094,-16.2901202367904,9.65368679011485));
#31102=CARTESIAN_POINT('Ctrl Pts',(17.3247045256125,-15.5,9.61202012344818));
#31103=CARTESIAN_POINT('Ctrl Pts',(16.8685283942094,-14.7098797632096,9.57035345678151));
#31104=CARTESIAN_POINT('Ctrl Pts',(16.4123522628062,-13.9197595264192,9.52868679011484));
#31105=CARTESIAN_POINT('Ctrl Pts',(15.5,-13.9197595264192,9.48702012344818));
#31106=CARTESIAN_POINT('Ctrl Pts',(14.5876477371938,-13.9197595264192,9.44535345678151));
#31107=CARTESIAN_POINT('Ctrl Pts',(14.1314716057906,-14.7098797632096,9.40368679011484));
#31108=CARTESIAN_POINT('Ctrl Pts',(13.6752954743875,-15.5,9.36202012344818));
#31109=CARTESIAN_POINT('Ctrl Pts',(14.1314716057906,-16.2901202367904,9.32035345678151));
#31110=CARTESIAN_POINT('Ctrl Pts',(14.5876477371938,-17.0802404735808,9.27868679011484));
#31111=CARTESIAN_POINT('Ctrl Pts',(15.5,-17.0802404735808,9.23702012344818));
#31112=CARTESIAN_POINT('Ctrl Pts',(16.4123522628062,-17.0802404735808,9.19535345678151));
#31113=CARTESIAN_POINT('Ctrl Pts',(16.8685283942094,-16.2901202367904,9.15368679011484));
#31114=CARTESIAN_POINT('Ctrl Pts',(17.3247045256125,-15.5,9.11202012344818));
#31115=CARTESIAN_POINT('Ctrl Pts',(16.8685283942094,-14.7098797632096,9.07035345678151));
#31116=CARTESIAN_POINT('Ctrl Pts',(16.4123522628062,-13.9197595264192,9.02868679011484));
#31117=CARTESIAN_POINT('Ctrl Pts',(15.5,-13.9197595264192,8.98702012344817));
#31118=CARTESIAN_POINT('Ctrl Pts',(14.5876477371938,-13.9197595264192,8.9453534567815));
#31119=CARTESIAN_POINT('Ctrl Pts',(14.1314716057906,-14.7098797632096,8.90368679011484));
#31120=CARTESIAN_POINT('Ctrl Pts',(13.6752954743875,-15.5,8.86202012344817));
#31121=CARTESIAN_POINT('Ctrl Pts',(14.1314716057906,-16.2901202367904,8.8203534567815));
#31122=CARTESIAN_POINT('Ctrl Pts',(14.5876477371938,-17.0802404735808,8.77868679011483));
#31123=CARTESIAN_POINT('Ctrl Pts',(15.5,-17.0802404735808,8.73702012344817));
#31124=CARTESIAN_POINT('Ctrl Pts',(16.4123522628062,-17.0802404735808,8.6953534567815));
#31125=CARTESIAN_POINT('Ctrl Pts',(16.8685283942094,-16.2901202367904,8.65368679011483));
#31126=CARTESIAN_POINT('Ctrl Pts',(17.3247045256125,-15.5,8.61202012344817));
#31127=CARTESIAN_POINT('Ctrl Pts',(16.8685283942094,-14.7098797632096,8.5703534567815));
#31128=CARTESIAN_POINT('Ctrl Pts',(16.4123522628062,-13.9197595264192,8.52868679011483));
#31129=CARTESIAN_POINT('Ctrl Pts',(15.5,-13.9197595264192,8.48702012344816));
#31130=CARTESIAN_POINT('Ctrl Pts',(14.5876477371938,-13.9197595264192,8.4453534567815));
#31131=CARTESIAN_POINT('Ctrl Pts',(14.1314716057906,-14.7098797632096,8.40368679011483));
#31132=CARTESIAN_POINT('Ctrl Pts',(13.6752954743875,-15.5,8.36202012344816));
#31133=CARTESIAN_POINT('Ctrl Pts',(14.1314716057906,-16.2901202367904,8.3203534567815));
#31134=CARTESIAN_POINT('Ctrl Pts',(14.5876477371938,-17.0802404735808,8.27868679011483));
#31135=CARTESIAN_POINT('Ctrl Pts',(15.5,-17.0802404735808,8.23702012344816));
#31136=CARTESIAN_POINT('Ctrl Pts',(16.4123522628062,-17.0802404735808,8.19535345678149));
#31137=CARTESIAN_POINT('Ctrl Pts',(16.8685283942094,-16.2901202367904,8.15368679011483));
#31138=CARTESIAN_POINT('Ctrl Pts',(17.3247045256125,-15.5,8.11202012344816));
#31139=CARTESIAN_POINT('Ctrl Pts',(16.8685283942094,-14.7098797632096,8.0703534567815));
#31140=CARTESIAN_POINT('Ctrl Pts',(16.4123522628062,-13.9197595264192,8.02868679011483));
#31141=CARTESIAN_POINT('Ctrl Pts',(15.5,-13.9197595264192,7.98702012344816));
#31142=CARTESIAN_POINT('Ctrl Pts',(14.5876477371938,-13.9197595264192,7.94535345678149));
#31143=CARTESIAN_POINT('Ctrl Pts',(14.1314716057906,-14.7098797632096,7.90368679011482));
#31144=CARTESIAN_POINT('Ctrl Pts',(13.6752954743875,-15.5,7.86202012344816));
#31145=CARTESIAN_POINT('Ctrl Pts',(14.1314716057906,-16.2901202367904,7.82035345678149));
#31146=CARTESIAN_POINT('Ctrl Pts',(14.5876477371938,-17.0802404735808,7.77868679011482));
#31147=CARTESIAN_POINT('Ctrl Pts',(15.5,-17.0802404735808,7.73702012344816));
#31148=CARTESIAN_POINT('Ctrl Pts',(16.4123522628062,-17.0802404735808,7.69535345678149));
#31149=CARTESIAN_POINT('Ctrl Pts',(16.8685283942094,-16.2901202367904,7.65368679011482));
#31150=CARTESIAN_POINT('Ctrl Pts',(17.3247045256125,-15.5,7.61202012344815));
#31151=CARTESIAN_POINT('Ctrl Pts',(16.8685283942094,-14.7098797632096,7.57035345678149));
#31152=CARTESIAN_POINT('Ctrl Pts',(16.4123522628062,-13.9197595264192,7.52868679011482));
#31153=CARTESIAN_POINT('Ctrl Pts',(15.5,-13.9197595264192,7.48702012344815));
#31154=CARTESIAN_POINT('Ctrl Pts',(14.5876477371938,-13.9197595264192,7.44535345678148));
#31155=CARTESIAN_POINT('Ctrl Pts',(14.1314716057906,-14.7098797632096,7.40368679011482));
#31156=CARTESIAN_POINT('Ctrl Pts',(13.6752954743875,-15.5,7.36202012344815));
#31157=CARTESIAN_POINT('Ctrl Pts',(14.1314716057906,-16.2901202367904,7.32035345678148));
#31158=CARTESIAN_POINT('Ctrl Pts',(14.5876477371938,-17.0802404735808,7.27868679011482));
#31159=CARTESIAN_POINT('Ctrl Pts',(15.5,-17.0802404735808,7.23702012344815));
#31160=CARTESIAN_POINT('Ctrl Pts',(16.4123522628062,-17.0802404735808,7.19535345678148));
#31161=CARTESIAN_POINT('Ctrl Pts',(16.8685283942094,-16.2901202367904,7.15368679011481));
#31162=CARTESIAN_POINT('Ctrl Pts',(17.3247045256125,-15.5,7.11202012344815));
#31163=CARTESIAN_POINT('Ctrl Pts',(16.8685283942094,-14.7098797632096,7.07035345678148));
#31164=CARTESIAN_POINT('Ctrl Pts',(16.4123522628062,-13.9197595264192,7.02868679011481));
#31165=CARTESIAN_POINT('Ctrl Pts',(15.5,-13.9197595264192,6.98702012344815));
#31166=CARTESIAN_POINT('Ctrl Pts',(14.5876477371938,-13.9197595264192,6.94535345678148));
#31167=CARTESIAN_POINT('Ctrl Pts',(14.1314716057906,-14.7098797632096,6.90368679011481));
#31168=CARTESIAN_POINT('Ctrl Pts',(13.6752954743875,-15.5,6.86202012344814));
#31169=CARTESIAN_POINT('Ctrl Pts',(14.1314716057906,-16.2901202367904,6.82035345678148));
#31170=CARTESIAN_POINT('Ctrl Pts',(14.5876477371938,-17.0802404735808,6.77868679011481));
#31171=CARTESIAN_POINT('Ctrl Pts',(15.5,-17.0802404735808,6.73702012344814));
#31172=CARTESIAN_POINT('Ctrl Pts',(16.4123522628062,-17.0802404735808,6.69535345678147));
#31173=CARTESIAN_POINT('Ctrl Pts',(16.8685283942094,-16.2901202367904,6.65368679011481));
#31174=CARTESIAN_POINT('Ctrl Pts',(17.3247045256125,-15.5,6.61202012344814));
#31175=CARTESIAN_POINT('Ctrl Pts',(16.8685283942094,-14.7098797632096,6.57035345678147));
#31176=CARTESIAN_POINT('Ctrl Pts',(16.4123522628062,-13.9197595264192,6.52868679011481));
#31177=CARTESIAN_POINT('Ctrl Pts',(15.5,-13.9197595264192,6.48702012344814));
#31178=CARTESIAN_POINT('Ctrl Pts',(14.5876477371938,-13.9197595264192,6.44535345678147));
#31179=CARTESIAN_POINT('Ctrl Pts',(14.1314716057906,-14.7098797632096,6.40368679011481));
#31180=CARTESIAN_POINT('Ctrl Pts',(13.6752954743875,-15.5,6.36202012344814));
#31181=CARTESIAN_POINT('Ctrl Pts',(14.1314716057906,-16.2901202367904,6.32035345678147));
#31182=CARTESIAN_POINT('Ctrl Pts',(14.5876477371938,-17.0802404735808,6.2786867901148));
#31183=CARTESIAN_POINT('Ctrl Pts',(15.5,-17.0802404735808,6.23702012344813));
#31184=CARTESIAN_POINT('Ctrl Pts',(16.4123522628062,-17.0802404735808,6.19535345678147));
#31185=CARTESIAN_POINT('Ctrl Pts',(16.8685283942094,-16.2901202367904,6.1536867901148));
#31186=CARTESIAN_POINT('Ctrl Pts',(17.3247045256125,-15.5,6.11202012344813));
#31187=CARTESIAN_POINT('Ctrl Pts',(16.8685283942094,-14.7098797632096,6.07035345678147));
#31188=CARTESIAN_POINT('Ctrl Pts',(16.4123522628062,-13.9197595264192,6.0286867901148));
#31189=CARTESIAN_POINT('Ctrl Pts',(15.5,-13.9197595264192,5.98702012344813));
#31190=CARTESIAN_POINT('Ctrl Pts',(14.5876477371938,-13.9197595264192,5.94535345678146));
#31191=CARTESIAN_POINT('Ctrl Pts',(14.1314716057906,-14.7098797632096,5.9036867901148));
#31192=CARTESIAN_POINT('Ctrl Pts',(13.6752954743875,-15.5,5.86202012344813));
#31193=CARTESIAN_POINT('Ctrl Pts',(14.1314716057906,-16.2901202367904,5.82035345678146));
#31194=CARTESIAN_POINT('Ctrl Pts',(14.5876477371938,-17.0802404735808,5.7786867901148));
#31195=CARTESIAN_POINT('Ctrl Pts',(15.5,-17.0802404735808,5.73702012344813));
#31196=CARTESIAN_POINT('Ctrl Pts',(16.4123522628062,-17.0802404735808,5.69535345678146));
#31197=CARTESIAN_POINT('Ctrl Pts',(16.8685283942094,-16.2901202367904,5.65368679011479));
#31198=CARTESIAN_POINT('Ctrl Pts',(17.3247045256125,-15.5,5.61202012344813));
#31199=CARTESIAN_POINT('Ctrl Pts',(16.8685283942094,-14.7098797632096,5.57035345678146));
#31200=CARTESIAN_POINT('Ctrl Pts',(16.4123522628062,-13.9197595264192,5.52868679011479));
#31201=CARTESIAN_POINT('Ctrl Pts',(15.5,-13.9197595264192,5.48702012344813));
#31202=CARTESIAN_POINT('Ctrl Pts',(14.5876477371938,-13.9197595264192,5.44535345678146));
#31203=CARTESIAN_POINT('Ctrl Pts',(14.1314716057906,-14.7098797632096,5.40368679011479));
#31204=CARTESIAN_POINT('Ctrl Pts',(13.6752954743875,-15.5,5.36202012344812));
#31205=CARTESIAN_POINT('Ctrl Pts',(14.1314716057906,-16.2901202367904,5.32035345678146));
#31206=CARTESIAN_POINT('Ctrl Pts',(14.5876477371938,-17.0802404735808,5.27868679011479));
#31207=CARTESIAN_POINT('Ctrl Pts',(15.5,-17.0802404735808,5.23702012344812));
#31208=CARTESIAN_POINT('Ctrl Pts',(16.4123522628062,-17.0802404735808,5.19535345678145));
#31209=CARTESIAN_POINT('Ctrl Pts',(16.8685283942094,-16.2901202367904,5.15368679011479));
#31210=CARTESIAN_POINT('Ctrl Pts',(17.3247045256125,-15.5,5.11202012344812));
#31211=CARTESIAN_POINT('Ctrl Pts',(16.8685283942094,-14.7098797632096,5.07035345678145));
#31212=CARTESIAN_POINT('Ctrl Pts',(16.4123522628062,-13.9197595264192,5.02868679011478));
#31213=CARTESIAN_POINT('Ctrl Pts',(15.5,-13.9197595264192,4.98702012344812));
#31214=CARTESIAN_POINT('Ctrl Pts',(14.5876477371938,-13.9197595264192,4.94535345678145));
#31215=CARTESIAN_POINT('Ctrl Pts',(14.1314716057906,-14.7098797632096,4.90368679011478));
#31216=CARTESIAN_POINT('Ctrl Pts',(13.6752954743875,-15.5,4.86202012344812));
#31217=CARTESIAN_POINT('Ctrl Pts',(14.1314716057906,-16.2901202367904,4.82035345678145));
#31218=CARTESIAN_POINT('Ctrl Pts',(14.5876477371938,-17.0802404735808,4.77868679011478));
#31219=CARTESIAN_POINT('Ctrl Pts',(15.5,-17.0802404735808,4.73702012344812));
#31220=CARTESIAN_POINT('Ctrl Pts',(16.4123522628062,-17.0802404735808,4.69535345678145));
#31221=CARTESIAN_POINT('Ctrl Pts',(16.8685283942094,-16.2901202367904,4.65368679011478));
#31222=CARTESIAN_POINT('Ctrl Pts',(17.3247045256125,-15.5,4.61202012344811));
#31223=CARTESIAN_POINT('Ctrl Pts',(16.8685283942094,-14.7098797632096,4.57035345678145));
#31224=CARTESIAN_POINT('Ctrl Pts',(16.4123522628062,-13.9197595264192,4.52868679011478));
#31225=CARTESIAN_POINT('Ctrl Pts',(15.5,-13.9197595264192,4.48702012344811));
#31226=CARTESIAN_POINT('Ctrl Pts',(14.5876477371938,-13.9197595264192,4.44535345678144));
#31227=CARTESIAN_POINT('Ctrl Pts',(14.1314716057906,-14.7098797632096,4.40368679011478));
#31228=CARTESIAN_POINT('Ctrl Pts',(13.6752954743875,-15.5,4.36202012344811));
#31229=CARTESIAN_POINT('Ctrl Pts',(14.1314716057906,-16.2901202367904,4.32035345678144));
#31230=CARTESIAN_POINT('Ctrl Pts',(14.5876477371938,-17.0802404735808,4.27868679011477));
#31231=CARTESIAN_POINT('Ctrl Pts',(15.5,-17.0802404735808,4.23702012344811));
#31232=CARTESIAN_POINT('Ctrl Pts',(16.4123522628062,-17.0802404735808,4.19535345678144));
#31233=CARTESIAN_POINT('Ctrl Pts',(16.8685283942094,-16.2901202367904,4.15368679011477));
#31234=CARTESIAN_POINT('Ctrl Pts',(17.3247045256125,-15.5,4.11202012344811));
#31235=CARTESIAN_POINT('Ctrl Pts',(16.8685283942094,-14.7098797632096,4.07035345678144));
#31236=CARTESIAN_POINT('Ctrl Pts',(16.4123522628062,-13.9197595264192,4.02868679011477));
#31237=CARTESIAN_POINT('Ctrl Pts',(15.5,-13.9197595264192,3.9870201234481));
#31238=CARTESIAN_POINT('Ctrl Pts',(14.5876477371938,-13.9197595264192,3.94535345678144));
#31239=CARTESIAN_POINT('Ctrl Pts',(14.1314716057906,-14.7098797632096,3.90368679011477));
#31240=CARTESIAN_POINT('Ctrl Pts',(13.6752954743875,-15.5,3.8620201234481));
#31241=CARTESIAN_POINT('Ctrl Pts',(14.1314716057906,-16.2901202367904,3.82035345678144));
#31242=CARTESIAN_POINT('Ctrl Pts',(14.5876477371938,-17.0802404735808,3.77868679011477));
#31243=CARTESIAN_POINT('Ctrl Pts',(15.5,-17.0802404735808,3.7370201234481));
#31244=CARTESIAN_POINT('Ctrl Pts',(16.4123522628062,-17.0802404735808,3.69535345678143));
#31245=CARTESIAN_POINT('Ctrl Pts',(16.8685283942094,-16.2901202367904,3.65368679011477));
#31246=CARTESIAN_POINT('Ctrl Pts',(17.3247045256125,-15.5,3.6120201234481));
#31247=CARTESIAN_POINT('Ctrl Pts',(16.8685283942094,-14.7098797632096,3.57035345678143));
#31248=CARTESIAN_POINT('Ctrl Pts',(16.4123522628062,-13.9197595264192,3.52868679011477));
#31249=CARTESIAN_POINT('Ctrl Pts',(15.5,-13.9197595264192,3.4870201234481));
#31250=CARTESIAN_POINT('Ctrl Pts',(14.5876477371938,-13.9197595264192,3.44535345678143));
#31251=CARTESIAN_POINT('Ctrl Pts',(14.1314716057906,-14.7098797632096,3.40368679011477));
#31252=CARTESIAN_POINT('Ctrl Pts',(13.6752954743875,-15.5,3.3620201234481));
#31253=CARTESIAN_POINT('Ctrl Pts',(14.1314716057906,-16.2901202367904,3.32035345678143));
#31254=CARTESIAN_POINT('Ctrl Pts',(14.5876477371938,-17.0802404735808,3.27868679011476));
#31255=CARTESIAN_POINT('Ctrl Pts',(15.5,-17.0802404735808,3.2370201234481));
#31256=CARTESIAN_POINT('Ctrl Pts',(16.4123522628062,-17.0802404735808,3.19535345678143));
#31257=CARTESIAN_POINT('Ctrl Pts',(16.8685283942094,-16.2901202367904,3.15368679011476));
#31258=CARTESIAN_POINT('Ctrl Pts',(17.3247045256125,-15.5,3.11202012344809));
#31259=CARTESIAN_POINT('Ctrl Pts',(16.8685283942094,-14.7098797632096,3.07035345678143));
#31260=CARTESIAN_POINT('Ctrl Pts',(16.4123522628062,-13.9197595264192,3.02868679011476));
#31261=CARTESIAN_POINT('Ctrl Pts',(15.5,-13.9197595264192,2.98702012344809));
#31262=CARTESIAN_POINT('Ctrl Pts',(14.5876477371938,-13.9197595264192,2.94535345678143));
#31263=CARTESIAN_POINT('Ctrl Pts',(14.1314716057906,-14.7098797632096,2.90368679011476));
#31264=CARTESIAN_POINT('Ctrl Pts',(13.6752954743875,-15.5,2.86202012344809));
#31265=CARTESIAN_POINT('Ctrl Pts',(14.1314716057906,-16.2901202367904,2.82035345678142));
#31266=CARTESIAN_POINT('Ctrl Pts',(14.5876477371938,-17.0802404735808,2.77868679011475));
#31267=CARTESIAN_POINT('Ctrl Pts',(15.5,-17.0802404735808,2.73702012344809));
#31268=CARTESIAN_POINT('Ctrl Pts',(16.4123522628062,-17.0802404735808,2.69535345678142));
#31269=CARTESIAN_POINT('Ctrl Pts',(16.8685283942094,-16.2901202367904,2.65368679011475));
#31270=CARTESIAN_POINT('Ctrl Pts',(17.3247045256125,-15.5,2.61202012344809));
#31271=CARTESIAN_POINT('Ctrl Pts',(16.8685283942094,-14.7098797632096,2.57035345678142));
#31272=CARTESIAN_POINT('Ctrl Pts',(16.4123522628062,-13.9197595264192,2.52868679011475));
#31273=CARTESIAN_POINT('Ctrl Pts',(15.5,-13.9197595264192,2.48702012344808));
#31274=CARTESIAN_POINT('Ctrl Pts',(14.5876477371938,-13.9197595264192,2.44535345678142));
#31275=CARTESIAN_POINT('Ctrl Pts',(14.1314716057906,-14.7098797632096,2.40368679011475));
#31276=CARTESIAN_POINT('Ctrl Pts',(13.6752954743875,-15.5,2.36202012344808));
#31277=CARTESIAN_POINT('Ctrl Pts',(14.1314716057906,-16.2901202367904,2.32035345678142));
#31278=CARTESIAN_POINT('Ctrl Pts',(14.5876477371938,-17.0802404735808,2.27868679011475));
#31279=CARTESIAN_POINT('Ctrl Pts',(15.5,-17.0802404735808,2.23702012344808));
#31280=CARTESIAN_POINT('Ctrl Pts',(16.4123522628062,-17.0802404735808,2.19535345678142));
#31281=CARTESIAN_POINT('Ctrl Pts',(16.8685283942094,-16.2901202367904,2.15368679011475));
#31282=CARTESIAN_POINT('Ctrl Pts',(17.3247045256125,-15.5,2.11202012344808));
#31283=CARTESIAN_POINT('Ctrl Pts',(16.8685283942094,-14.7098797632096,2.07035345678141));
#31284=CARTESIAN_POINT('Ctrl Pts',(16.4123522628062,-13.9197595264192,2.02868679011475));
#31285=CARTESIAN_POINT('Ctrl Pts',(15.5,-13.9197595264192,1.98702012344808));
#31286=CARTESIAN_POINT('Ctrl Pts',(14.5876477371938,-13.9197595264192,1.94535345678141));
#31287=CARTESIAN_POINT('Ctrl Pts',(14.1314716057906,-14.7098797632096,1.90368679011474));
#31288=CARTESIAN_POINT('Ctrl Pts',(13.6752954743875,-15.5,1.86202012344808));
#31289=CARTESIAN_POINT('Ctrl Pts',(14.1314716057906,-16.2901202367904,1.82035345678141));
#31290=CARTESIAN_POINT('Ctrl Pts',(14.5876477371938,-17.0802404735808,1.77868679011474));
#31291=CARTESIAN_POINT('Ctrl Pts',(15.5,-17.0802404735808,1.73702012344808));
#31292=CARTESIAN_POINT('Ctrl Pts',(16.4123522628062,-17.0802404735808,1.69535345678141));
#31293=CARTESIAN_POINT('Ctrl Pts',(16.8685283942094,-16.2901202367904,1.65368679011474));
#31294=CARTESIAN_POINT('Ctrl Pts',(17.3247045256125,-15.5,1.61202012344807));
#31295=CARTESIAN_POINT('Ctrl Pts',(16.8685283942094,-14.7098797632096,1.57035345678141));
#31296=CARTESIAN_POINT('Ctrl Pts',(16.4123522628062,-13.9197595264192,1.52868679011474));
#31297=CARTESIAN_POINT('Ctrl Pts',(15.5,-13.9197595264192,1.48702012344807));
#31298=CARTESIAN_POINT('Ctrl Pts',(14.5876477371938,-13.9197595264192,1.4453534567814));
#31299=CARTESIAN_POINT('Ctrl Pts',(14.1314716057906,-14.7098797632096,1.40368679011474));
#31300=CARTESIAN_POINT('Ctrl Pts',(13.6752954743875,-15.5,1.36202012344807));
#31301=CARTESIAN_POINT('Ctrl Pts',(14.1314716057906,-16.2901202367904,1.3203534567814));
#31302=CARTESIAN_POINT('Ctrl Pts',(14.5876477371938,-17.0802404735808,1.27868679011473));
#31303=CARTESIAN_POINT('Ctrl Pts',(15.5,-17.0802404735808,1.23702012344807));
#31304=CARTESIAN_POINT('Ctrl Pts',(16.4123522628062,-17.0802404735808,1.1953534567814));
#31305=CARTESIAN_POINT('Ctrl Pts',(16.8685283942094,-16.2901202367904,1.15368679011473));
#31306=CARTESIAN_POINT('Ctrl Pts',(17.3247045256125,-15.5,1.11202012344807));
#31307=CARTESIAN_POINT('Ctrl Pts',(16.8685283942094,-14.7098797632096,1.0703534567814));
#31308=CARTESIAN_POINT('Ctrl Pts',(16.4123522628062,-13.9197595264192,1.02868679011473));
#31309=CARTESIAN_POINT('Ctrl Pts',(15.5,-13.9197595264192,0.987020123448066));
#31310=CARTESIAN_POINT('Ctrl Pts',(14.5876477371938,-13.9197595264192,0.945353456781398));
#31311=CARTESIAN_POINT('Ctrl Pts',(14.1314716057906,-14.7098797632096,0.903686790114731));
#31312=CARTESIAN_POINT('Ctrl Pts',(13.6752954743875,-15.5,0.862020123448063));
#31313=CARTESIAN_POINT('Ctrl Pts',(14.1314716057906,-16.2901202367904,0.820353456781396));
#31314=CARTESIAN_POINT('Ctrl Pts',(14.5876477371938,-17.0802404735808,0.778686790114729));
#31315=CARTESIAN_POINT('Ctrl Pts',(15.5,-17.0802404735808,0.737020123448062));
#31316=CARTESIAN_POINT('Ctrl Pts',(16.4123522628062,-17.0802404735808,0.695353456781395));
#31317=CARTESIAN_POINT('Ctrl Pts',(16.8685283942094,-16.2901202367904,0.653686790114727));
#31318=CARTESIAN_POINT('Ctrl Pts',(17.3247045256125,-15.5,0.61202012344806));
#31319=CARTESIAN_POINT('Ctrl Pts',(16.8685283942094,-14.7098797632096,0.570353456781393));
#31320=CARTESIAN_POINT('Ctrl Pts',(16.4123522628062,-13.9197595264192,0.528686790114725));
#31321=CARTESIAN_POINT('Ctrl Pts',(15.5,-13.9197595264192,0.487020123448058));
#31322=CARTESIAN_POINT('Ctrl Pts',(14.5876477371938,-13.9197595264192,0.445353456781391));
#31323=CARTESIAN_POINT('Ctrl Pts',(14.1314716057906,-14.7098797632096,0.403686790114724));
#31324=CARTESIAN_POINT('Ctrl Pts',(13.6752954743875,-15.5,0.362020123448056));
#31325=CARTESIAN_POINT('Ctrl Pts',(14.1314716057906,-16.2901202367904,0.320353456781389));
#31326=CARTESIAN_POINT('Ctrl Pts',(14.5876477371938,-17.0802404735808,0.278686790114722));
#31327=CARTESIAN_POINT('Ctrl Pts',(15.5,-17.0802404735808,0.237020123448055));
#31328=CARTESIAN_POINT('Ctrl Pts',(16.4123522628062,-17.0802404735808,0.195353456781387));
#31329=CARTESIAN_POINT('Ctrl Pts',(16.8685283942094,-16.2901202367904,0.15368679011472));
#31330=CARTESIAN_POINT('Ctrl Pts',(17.3247045256125,-15.5,0.112020123448053));
#31331=CARTESIAN_POINT('Ctrl Pts',(16.8685283942094,-14.7098797632096,0.0703534567813853));
#31332=CARTESIAN_POINT('Ctrl Pts',(16.4123522628062,-13.9197595264192,0.028686790114718));
#31333=CARTESIAN_POINT('Ctrl Pts',(15.5,-13.9197595264192,-0.0129798765519492));
#31334=CARTESIAN_POINT('Ctrl Pts',(14.5876477371938,-13.9197595264192,-0.0546465432186148));
#31335=CARTESIAN_POINT('Ctrl Pts',(14.1314716057906,-14.7098797632096,-0.0963132098852821));
#31336=CARTESIAN_POINT('Ctrl Pts',(13.6752954743875,-15.5,-0.137979876551949));
#31337=CARTESIAN_POINT('Ctrl Pts',(14.1314716057906,-16.2901202367904,-0.179646543218617));
#31338=CARTESIAN_POINT('Ctrl Pts',(14.5876477371938,-17.0802404735808,-0.221313209885284));
#31339=CARTESIAN_POINT('Ctrl Pts',(15.5,-17.0802404735808,-0.262979876551951));
#31340=CARTESIAN_POINT('Ctrl Pts',(16.4123522628062,-17.0802404735808,-0.304646543218618));
#31341=CARTESIAN_POINT('Ctrl Pts',(16.8685283942094,-16.2901202367904,-0.346313209885286));
#31342=CARTESIAN_POINT('Ctrl Pts',(17.3247045256125,-15.5,-0.387979876551953));
#31343=CARTESIAN_POINT('Ctrl Pts',(16.8685283942094,-14.7098797632096,-0.42964654321862));
#31344=CARTESIAN_POINT('Ctrl Pts',(16.4123522628062,-13.9197595264192,-0.471313209885288));
#31345=CARTESIAN_POINT('Ctrl Pts',(15.5,-13.9197595264192,-0.512979876551955));
#31346=CARTESIAN_POINT('Ctrl Pts',(14.5876477371938,-13.9197595264192,-0.554646543218622));
#31347=CARTESIAN_POINT('Ctrl Pts',(14.1314716057906,-14.7098797632096,-0.596313209885289));
#31348=CARTESIAN_POINT('Ctrl Pts',(13.6752954743875,-15.5,-0.637979876551957));
#31349=CARTESIAN_POINT('Ctrl Pts',(14.1314716057906,-16.2901202367904,-0.679646543218624));
#31350=CARTESIAN_POINT('Ctrl Pts',(14.5876477371938,-17.0802404735808,-0.721313209885291));
#31351=CARTESIAN_POINT('Ctrl Pts',(15.5,-17.0802404735808,-0.762979876551959));
#31352=CARTESIAN_POINT('Ctrl Pts',(16.4123522628062,-17.0802404735808,-0.804646543218626));
#31353=CARTESIAN_POINT('Ctrl Pts',(16.8685283942094,-16.2901202367904,-0.846313209885293));
#31354=CARTESIAN_POINT('Ctrl Pts',(17.3247045256125,-15.5,-0.88797987655196));
#31355=CARTESIAN_POINT('Ctrl Pts',(16.8685283942094,-14.7098797632096,-0.929646543218628));
#31356=CARTESIAN_POINT('Ctrl Pts',(16.4123522628062,-13.9197595264192,-0.971313209885295));
#31357=CARTESIAN_POINT('Ctrl Pts',(15.5,-13.9197595264192,-1.01297987655196));
#31358=CARTESIAN_POINT('Ctrl Pts',(14.5876477371938,-13.9197595264192,-1.05464654321863));
#31359=CARTESIAN_POINT('Ctrl Pts',(14.1314716057906,-14.7098797632096,-1.0963132098853));
#31360=CARTESIAN_POINT('Ctrl Pts',(13.6752954743875,-15.5,-1.13797987655196));
#31361=CARTESIAN_POINT('Ctrl Pts',(14.1314716057906,-16.2901202367904,-1.17964654321863));
#31362=CARTESIAN_POINT('Ctrl Pts',(14.5876477371938,-17.0802404735808,-1.2213132098853));
#31363=CARTESIAN_POINT('Ctrl Pts',(15.5,-17.0802404735808,-1.26297987655196));
#31364=CARTESIAN_POINT('Ctrl Pts',(16.4123522628062,-17.0802404735808,-1.30464654321863));
#31365=CARTESIAN_POINT('Ctrl Pts',(16.8685283942094,-16.2901202367904,-1.3463132098853));
#31366=CARTESIAN_POINT('Ctrl Pts',(17.3247045256125,-15.5,-1.38797987655197));
#31367=CARTESIAN_POINT('Ctrl Pts',(16.8685283942094,-14.7098797632096,-1.42964654321863));
#31368=CARTESIAN_POINT('Ctrl Pts',(16.4123522628062,-13.9197595264192,-1.4713132098853));
#31369=CARTESIAN_POINT('Ctrl Pts',(15.5,-13.9197595264192,-1.51297987655197));
#31370=CARTESIAN_POINT('Ctrl Pts',(14.5876477371938,-13.9197595264192,-1.55464654321864));
#31371=CARTESIAN_POINT('Ctrl Pts',(14.1314716057906,-14.7098797632096,-1.5963132098853));
#31372=CARTESIAN_POINT('Ctrl Pts',(13.6752954743875,-15.5,-1.63797987655197));
#31373=CARTESIAN_POINT('Ctrl Pts',(14.1314716057906,-16.2901202367904,-1.67964654321864));
#31374=CARTESIAN_POINT('Ctrl Pts',(14.5876477371938,-17.0802404735808,-1.7213132098853));
#31375=CARTESIAN_POINT('Ctrl Pts',(15.5,-17.0802404735808,-1.76297987655197));
#31376=CARTESIAN_POINT('Ctrl Pts',(16.4123522628062,-17.0802404735808,-1.80464654321864));
#31377=CARTESIAN_POINT('Ctrl Pts',(16.8685283942094,-16.2901202367904,-1.84631320988531));
#31378=CARTESIAN_POINT('Ctrl Pts',(17.3247045256125,-15.5,-1.88797987655197));
#31379=CARTESIAN_POINT('Ctrl Pts',(16.8685283942094,-14.7098797632096,-1.92964654321864));
#31380=CARTESIAN_POINT('Ctrl Pts',(16.700583153372,-14.4189900731899,-1.94498649173085));
#31381=CARTESIAN_POINT('Ctrl Pts',(16.4288420454487,-14.2215586016756,-1.96260250461286));
#31382=CARTESIAN_POINT('Ctrl Pts',(15.3465777998745,-13.4352476007234,-2.03276185973389));
#31383=CARTESIAN_POINT('Ctrl Pts',(14.2643135543003,-12.6489365997713,-2.10292121485492));
#31384=CARTESIAN_POINT('Ctrl Pts',(15.5,-17.0802404735808,11.1745));
#31385=CARTESIAN_POINT('Ctrl Pts',(16.4123522628062,-17.0802404735808,11.1328333333333));
#31386=CARTESIAN_POINT('Ctrl Pts',(16.8685283942094,-16.2901202367904,11.0911666666667));
#31387=CARTESIAN_POINT('Ctrl Pts',(17.3247045256125,-15.5,11.0495));
#31388=CARTESIAN_POINT('Ctrl Pts',(16.8685283942094,-14.7098797632096,11.0078333333333));
#31389=CARTESIAN_POINT('Ctrl Pts',(16.4123522628062,-13.9197595264192,10.9661666666667));
#31390=CARTESIAN_POINT('Ctrl Pts',(15.5,-13.9197595264192,10.9245));
#31391=CARTESIAN_POINT('Ctrl Pts',(14.5876477371938,-13.9197595264192,10.8828333333333));
#31392=CARTESIAN_POINT('Ctrl Pts',(14.1314716057906,-14.7098797632096,10.8411666666667));
#31393=CARTESIAN_POINT('Ctrl Pts',(13.6752954743875,-15.5,10.7995));
#31394=CARTESIAN_POINT('Ctrl Pts',(14.1314716057906,-16.2901202367904,10.7578333333333));
#31395=CARTESIAN_POINT('Ctrl Pts',(14.5876477371938,-17.0802404735808,10.7161666666667));
#31396=CARTESIAN_POINT('Ctrl Pts',(15.5,-17.0802404735808,10.6745));
#31397=CARTESIAN_POINT('Ctrl Pts',(16.4123522628062,-17.0802404735808,10.6328333333333));
#31398=CARTESIAN_POINT('Ctrl Pts',(16.8685283942094,-16.2901202367904,10.5911666666667));
#31399=CARTESIAN_POINT('Ctrl Pts',(17.3247045256125,-15.5,10.5495));
#31400=CARTESIAN_POINT('Ctrl Pts',(16.8685283942094,-14.7098797632096,10.5078333333333));
#31401=CARTESIAN_POINT('Ctrl Pts',(16.4123522628062,-13.9197595264192,10.4661666666667));
#31402=CARTESIAN_POINT('Ctrl Pts',(15.5,-13.9197595264192,10.4245));
#31403=CARTESIAN_POINT('Ctrl Pts',(14.5876477371938,-13.9197595264192,10.3828333333333));
#31404=CARTESIAN_POINT('Ctrl Pts',(14.1314716057906,-14.7098797632096,10.3411666666667));
#31405=CARTESIAN_POINT('Ctrl Pts',(13.6752954743875,-15.5,10.2995));
#31406=CARTESIAN_POINT('Ctrl Pts',(14.1314716057906,-16.2901202367904,10.2578333333333));
#31407=CARTESIAN_POINT('Ctrl Pts',(14.5876477371938,-17.0802404735808,10.2161666666667));
#31408=CARTESIAN_POINT('Ctrl Pts',(15.5,-17.0802404735808,10.1745));
#31409=CARTESIAN_POINT('Ctrl Pts',(16.4123522628062,-17.0802404735808,10.1328333333333));
#31410=CARTESIAN_POINT('Ctrl Pts',(16.8685283942094,-16.2901202367904,10.0911666666667));
#31411=CARTESIAN_POINT('Ctrl Pts',(17.3247045256125,-15.5,10.0495));
#31412=CARTESIAN_POINT('Ctrl Pts',(16.8685283942094,-14.7098797632096,10.0078333333333));
#31413=CARTESIAN_POINT('Ctrl Pts',(16.4123522628062,-13.9197595264192,9.96616666666665));
#31414=CARTESIAN_POINT('Ctrl Pts',(15.5,-13.9197595264192,9.92449999999998));
#31415=CARTESIAN_POINT('Ctrl Pts',(14.5876477371938,-13.9197595264192,9.88283333333331));
#31416=CARTESIAN_POINT('Ctrl Pts',(14.1314716057906,-14.7098797632096,9.84116666666665));
#31417=CARTESIAN_POINT('Ctrl Pts',(13.6752954743875,-15.5,9.79949999999998));
#31418=CARTESIAN_POINT('Ctrl Pts',(14.1314716057906,-16.2901202367904,9.75783333333331));
#31419=CARTESIAN_POINT('Ctrl Pts',(14.5876477371938,-17.0802404735808,9.71616666666665));
#31420=CARTESIAN_POINT('Ctrl Pts',(15.5,-17.0802404735808,9.67449999999998));
#31421=CARTESIAN_POINT('Ctrl Pts',(16.4123522628062,-17.0802404735808,9.63283333333331));
#31422=CARTESIAN_POINT('Ctrl Pts',(16.8685283942094,-16.2901202367904,9.59116666666664));
#31423=CARTESIAN_POINT('Ctrl Pts',(17.3247045256125,-15.5,9.54949999999998));
#31424=CARTESIAN_POINT('Ctrl Pts',(16.8685283942094,-14.7098797632096,9.50783333333331));
#31425=CARTESIAN_POINT('Ctrl Pts',(16.4123522628062,-13.9197595264192,9.46616666666664));
#31426=CARTESIAN_POINT('Ctrl Pts',(15.5,-13.9197595264192,9.42449999999998));
#31427=CARTESIAN_POINT('Ctrl Pts',(14.5876477371938,-13.9197595264192,9.38283333333331));
#31428=CARTESIAN_POINT('Ctrl Pts',(14.1314716057906,-14.7098797632096,9.34116666666664));
#31429=CARTESIAN_POINT('Ctrl Pts',(13.6752954743875,-15.5,9.29949999999998));
#31430=CARTESIAN_POINT('Ctrl Pts',(14.1314716057906,-16.2901202367904,9.25783333333331));
#31431=CARTESIAN_POINT('Ctrl Pts',(14.5876477371938,-17.0802404735808,9.21616666666664));
#31432=CARTESIAN_POINT('Ctrl Pts',(15.5,-17.0802404735808,9.17449999999997));
#31433=CARTESIAN_POINT('Ctrl Pts',(16.4123522628062,-17.0802404735808,9.13283333333331));
#31434=CARTESIAN_POINT('Ctrl Pts',(16.8685283942094,-16.2901202367904,9.09116666666664));
#31435=CARTESIAN_POINT('Ctrl Pts',(17.3247045256125,-15.5,9.04949999999997));
#31436=CARTESIAN_POINT('Ctrl Pts',(16.8685283942094,-14.7098797632096,9.0078333333333));
#31437=CARTESIAN_POINT('Ctrl Pts',(16.4123522628062,-13.9197595264192,8.96616666666664));
#31438=CARTESIAN_POINT('Ctrl Pts',(15.5,-13.9197595264192,8.92449999999997));
#31439=CARTESIAN_POINT('Ctrl Pts',(14.5876477371938,-13.9197595264192,8.8828333333333));
#31440=CARTESIAN_POINT('Ctrl Pts',(14.1314716057906,-14.7098797632096,8.84116666666664));
#31441=CARTESIAN_POINT('Ctrl Pts',(13.6752954743875,-15.5,8.79949999999997));
#31442=CARTESIAN_POINT('Ctrl Pts',(14.1314716057906,-16.2901202367904,8.7578333333333));
#31443=CARTESIAN_POINT('Ctrl Pts',(14.5876477371938,-17.0802404735808,8.71616666666663));
#31444=CARTESIAN_POINT('Ctrl Pts',(15.5,-17.0802404735808,8.67449999999997));
#31445=CARTESIAN_POINT('Ctrl Pts',(16.4123522628062,-17.0802404735808,8.6328333333333));
#31446=CARTESIAN_POINT('Ctrl Pts',(16.8685283942094,-16.2901202367904,8.59116666666663));
#31447=CARTESIAN_POINT('Ctrl Pts',(17.3247045256125,-15.5,8.54949999999996));
#31448=CARTESIAN_POINT('Ctrl Pts',(16.8685283942094,-14.7098797632096,8.50783333333329));
#31449=CARTESIAN_POINT('Ctrl Pts',(16.4123522628062,-13.9197595264192,8.46616666666663));
#31450=CARTESIAN_POINT('Ctrl Pts',(15.5,-13.9197595264192,8.42449999999996));
#31451=CARTESIAN_POINT('Ctrl Pts',(14.5876477371938,-13.9197595264192,8.3828333333333));
#31452=CARTESIAN_POINT('Ctrl Pts',(14.1314716057906,-14.7098797632096,8.34116666666663));
#31453=CARTESIAN_POINT('Ctrl Pts',(13.6752954743875,-15.5,8.29949999999996));
#31454=CARTESIAN_POINT('Ctrl Pts',(14.1314716057906,-16.2901202367904,8.25783333333329));
#31455=CARTESIAN_POINT('Ctrl Pts',(14.5876477371938,-17.0802404735808,8.21616666666663));
#31456=CARTESIAN_POINT('Ctrl Pts',(15.5,-17.0802404735808,8.17449999999996));
#31457=CARTESIAN_POINT('Ctrl Pts',(16.4123522628062,-17.0802404735808,8.13283333333329));
#31458=CARTESIAN_POINT('Ctrl Pts',(16.8685283942094,-16.2901202367904,8.09116666666663));
#31459=CARTESIAN_POINT('Ctrl Pts',(17.3247045256125,-15.5,8.04949999999996));
#31460=CARTESIAN_POINT('Ctrl Pts',(16.8685283942094,-14.7098797632096,8.00783333333329));
#31461=CARTESIAN_POINT('Ctrl Pts',(16.4123522628062,-13.9197595264192,7.96616666666662));
#31462=CARTESIAN_POINT('Ctrl Pts',(15.5,-13.9197595264192,7.92449999999996));
#31463=CARTESIAN_POINT('Ctrl Pts',(14.5876477371938,-13.9197595264192,7.88283333333329));
#31464=CARTESIAN_POINT('Ctrl Pts',(14.1314716057906,-14.7098797632096,7.84116666666662));
#31465=CARTESIAN_POINT('Ctrl Pts',(13.6752954743875,-15.5,7.79949999999995));
#31466=CARTESIAN_POINT('Ctrl Pts',(14.1314716057906,-16.2901202367904,7.75783333333329));
#31467=CARTESIAN_POINT('Ctrl Pts',(14.5876477371938,-17.0802404735808,7.71616666666662));
#31468=CARTESIAN_POINT('Ctrl Pts',(15.5,-17.0802404735808,7.67449999999995));
#31469=CARTESIAN_POINT('Ctrl Pts',(16.4123522628062,-17.0802404735808,7.63283333333328));
#31470=CARTESIAN_POINT('Ctrl Pts',(16.8685283942094,-16.2901202367904,7.59116666666662));
#31471=CARTESIAN_POINT('Ctrl Pts',(17.3247045256125,-15.5,7.54949999999995));
#31472=CARTESIAN_POINT('Ctrl Pts',(16.8685283942094,-14.7098797632096,7.50783333333328));
#31473=CARTESIAN_POINT('Ctrl Pts',(16.4123522628062,-13.9197595264192,7.46616666666662));
#31474=CARTESIAN_POINT('Ctrl Pts',(15.5,-13.9197595264192,7.42449999999995));
#31475=CARTESIAN_POINT('Ctrl Pts',(14.5876477371938,-13.9197595264192,7.38283333333328));
#31476=CARTESIAN_POINT('Ctrl Pts',(14.1314716057906,-14.7098797632096,7.34116666666661));
#31477=CARTESIAN_POINT('Ctrl Pts',(13.6752954743875,-15.5,7.29949999999995));
#31478=CARTESIAN_POINT('Ctrl Pts',(14.1314716057906,-16.2901202367904,7.25783333333328));
#31479=CARTESIAN_POINT('Ctrl Pts',(14.5876477371938,-17.0802404735808,7.21616666666661));
#31480=CARTESIAN_POINT('Ctrl Pts',(15.5,-17.0802404735808,7.17449999999995));
#31481=CARTESIAN_POINT('Ctrl Pts',(16.4123522628062,-17.0802404735808,7.13283333333328));
#31482=CARTESIAN_POINT('Ctrl Pts',(16.8685283942094,-16.2901202367904,7.09116666666661));
#31483=CARTESIAN_POINT('Ctrl Pts',(17.3247045256125,-15.5,7.04949999999994));
#31484=CARTESIAN_POINT('Ctrl Pts',(16.8685283942094,-14.7098797632096,7.00783333333328));
#31485=CARTESIAN_POINT('Ctrl Pts',(16.4123522628062,-13.9197595264192,6.96616666666661));
#31486=CARTESIAN_POINT('Ctrl Pts',(15.5,-13.9197595264192,6.92449999999994));
#31487=CARTESIAN_POINT('Ctrl Pts',(14.5876477371938,-13.9197595264192,6.88283333333327));
#31488=CARTESIAN_POINT('Ctrl Pts',(14.1314716057906,-14.7098797632096,6.84116666666661));
#31489=CARTESIAN_POINT('Ctrl Pts',(13.6752954743875,-15.5,6.79949999999994));
#31490=CARTESIAN_POINT('Ctrl Pts',(14.1314716057906,-16.2901202367904,6.75783333333327));
#31491=CARTESIAN_POINT('Ctrl Pts',(14.5876477371938,-17.0802404735808,6.71616666666661));
#31492=CARTESIAN_POINT('Ctrl Pts',(15.5,-17.0802404735808,6.67449999999994));
#31493=CARTESIAN_POINT('Ctrl Pts',(16.4123522628062,-17.0802404735808,6.63283333333327));
#31494=CARTESIAN_POINT('Ctrl Pts',(16.8685283942094,-16.2901202367904,6.59116666666661));
#31495=CARTESIAN_POINT('Ctrl Pts',(17.3247045256125,-15.5,6.54949999999994));
#31496=CARTESIAN_POINT('Ctrl Pts',(16.8685283942094,-14.7098797632096,6.50783333333327));
#31497=CARTESIAN_POINT('Ctrl Pts',(16.4123522628062,-13.9197595264192,6.4661666666666));
#31498=CARTESIAN_POINT('Ctrl Pts',(15.5,-13.9197595264192,6.42449999999994));
#31499=CARTESIAN_POINT('Ctrl Pts',(14.5876477371938,-13.9197595264192,6.38283333333327));
#31500=CARTESIAN_POINT('Ctrl Pts',(14.1314716057906,-14.7098797632096,6.3411666666666));
#31501=CARTESIAN_POINT('Ctrl Pts',(13.6752954743875,-15.5,6.29949999999993));
#31502=CARTESIAN_POINT('Ctrl Pts',(14.1314716057906,-16.2901202367904,6.25783333333327));
#31503=CARTESIAN_POINT('Ctrl Pts',(14.5876477371938,-17.0802404735808,6.2161666666666));
#31504=CARTESIAN_POINT('Ctrl Pts',(15.5,-17.0802404735808,6.17449999999993));
#31505=CARTESIAN_POINT('Ctrl Pts',(16.4123522628062,-17.0802404735808,6.13283333333326));
#31506=CARTESIAN_POINT('Ctrl Pts',(16.8685283942094,-16.2901202367904,6.0911666666666));
#31507=CARTESIAN_POINT('Ctrl Pts',(17.3247045256125,-15.5,6.04949999999993));
#31508=CARTESIAN_POINT('Ctrl Pts',(16.8685283942094,-14.7098797632096,6.00783333333326));
#31509=CARTESIAN_POINT('Ctrl Pts',(16.4123522628062,-13.9197595264192,5.9661666666666));
#31510=CARTESIAN_POINT('Ctrl Pts',(15.5,-13.9197595264192,5.92449999999993));
#31511=CARTESIAN_POINT('Ctrl Pts',(14.5876477371938,-13.9197595264192,5.88283333333326));
#31512=CARTESIAN_POINT('Ctrl Pts',(14.1314716057906,-14.7098797632096,5.8411666666666));
#31513=CARTESIAN_POINT('Ctrl Pts',(13.6752954743875,-15.5,5.79949999999993));
#31514=CARTESIAN_POINT('Ctrl Pts',(14.1314716057906,-16.2901202367904,5.75783333333326));
#31515=CARTESIAN_POINT('Ctrl Pts',(14.5876477371938,-17.0802404735808,5.71616666666659));
#31516=CARTESIAN_POINT('Ctrl Pts',(15.5,-17.0802404735808,5.67449999999993));
#31517=CARTESIAN_POINT('Ctrl Pts',(16.4123522628062,-17.0802404735808,5.63283333333326));
#31518=CARTESIAN_POINT('Ctrl Pts',(16.8685283942094,-16.2901202367904,5.59116666666659));
#31519=CARTESIAN_POINT('Ctrl Pts',(17.3247045256125,-15.5,5.54949999999992));
#31520=CARTESIAN_POINT('Ctrl Pts',(16.8685283942094,-14.7098797632096,5.50783333333326));
#31521=CARTESIAN_POINT('Ctrl Pts',(16.4123522628062,-13.9197595264192,5.46616666666659));
#31522=CARTESIAN_POINT('Ctrl Pts',(15.5,-13.9197595264192,5.42449999999992));
#31523=CARTESIAN_POINT('Ctrl Pts',(14.5876477371938,-13.9197595264192,5.38283333333326));
#31524=CARTESIAN_POINT('Ctrl Pts',(14.1314716057906,-14.7098797632096,5.34116666666659));
#31525=CARTESIAN_POINT('Ctrl Pts',(13.6752954743875,-15.5,5.29949999999992));
#31526=CARTESIAN_POINT('Ctrl Pts',(14.1314716057906,-16.2901202367904,5.25783333333325));
#31527=CARTESIAN_POINT('Ctrl Pts',(14.5876477371938,-17.0802404735808,5.21616666666659));
#31528=CARTESIAN_POINT('Ctrl Pts',(15.5,-17.0802404735808,5.17449999999992));
#31529=CARTESIAN_POINT('Ctrl Pts',(16.4123522628062,-17.0802404735808,5.13283333333325));
#31530=CARTESIAN_POINT('Ctrl Pts',(16.8685283942094,-16.2901202367904,5.09116666666658));
#31531=CARTESIAN_POINT('Ctrl Pts',(17.3247045256125,-15.5,5.04949999999992));
#31532=CARTESIAN_POINT('Ctrl Pts',(16.8685283942094,-14.7098797632096,5.00783333333325));
#31533=CARTESIAN_POINT('Ctrl Pts',(16.4123522628062,-13.9197595264192,4.96616666666658));
#31534=CARTESIAN_POINT('Ctrl Pts',(15.5,-13.9197595264192,4.92449999999992));
#31535=CARTESIAN_POINT('Ctrl Pts',(14.5876477371938,-13.9197595264192,4.88283333333325));
#31536=CARTESIAN_POINT('Ctrl Pts',(14.1314716057906,-14.7098797632096,4.84116666666658));
#31537=CARTESIAN_POINT('Ctrl Pts',(13.6752954743875,-15.5,4.79949999999991));
#31538=CARTESIAN_POINT('Ctrl Pts',(14.1314716057906,-16.2901202367904,4.75783333333325));
#31539=CARTESIAN_POINT('Ctrl Pts',(14.5876477371938,-17.0802404735808,4.71616666666658));
#31540=CARTESIAN_POINT('Ctrl Pts',(15.5,-17.0802404735808,4.67449999999991));
#31541=CARTESIAN_POINT('Ctrl Pts',(16.4123522628062,-17.0802404735808,4.63283333333324));
#31542=CARTESIAN_POINT('Ctrl Pts',(16.8685283942094,-16.2901202367904,4.59116666666658));
#31543=CARTESIAN_POINT('Ctrl Pts',(17.3247045256125,-15.5,4.54949999999991));
#31544=CARTESIAN_POINT('Ctrl Pts',(16.8685283942094,-14.7098797632096,4.50783333333324));
#31545=CARTESIAN_POINT('Ctrl Pts',(16.4123522628062,-13.9197595264192,4.46616666666658));
#31546=CARTESIAN_POINT('Ctrl Pts',(15.5,-13.9197595264192,4.42449999999991));
#31547=CARTESIAN_POINT('Ctrl Pts',(14.5876477371938,-13.9197595264192,4.38283333333324));
#31548=CARTESIAN_POINT('Ctrl Pts',(14.1314716057906,-14.7098797632096,4.34116666666657));
#31549=CARTESIAN_POINT('Ctrl Pts',(13.6752954743875,-15.5,4.29949999999991));
#31550=CARTESIAN_POINT('Ctrl Pts',(14.1314716057906,-16.2901202367904,4.25783333333324));
#31551=CARTESIAN_POINT('Ctrl Pts',(14.5876477371938,-17.0802404735808,4.21616666666657));
#31552=CARTESIAN_POINT('Ctrl Pts',(15.5,-17.0802404735808,4.17449999999991));
#31553=CARTESIAN_POINT('Ctrl Pts',(16.4123522628062,-17.0802404735808,4.13283333333324));
#31554=CARTESIAN_POINT('Ctrl Pts',(16.8685283942094,-16.2901202367904,4.09116666666657));
#31555=CARTESIAN_POINT('Ctrl Pts',(17.3247045256125,-15.5,4.0494999999999));
#31556=CARTESIAN_POINT('Ctrl Pts',(16.8685283942094,-14.7098797632096,4.00783333333324));
#31557=CARTESIAN_POINT('Ctrl Pts',(16.4123522628062,-13.9197595264192,3.96616666666657));
#31558=CARTESIAN_POINT('Ctrl Pts',(15.5,-13.9197595264192,3.9244999999999));
#31559=CARTESIAN_POINT('Ctrl Pts',(14.5876477371938,-13.9197595264192,3.88283333333323));
#31560=CARTESIAN_POINT('Ctrl Pts',(14.1314716057906,-14.7098797632096,3.84116666666657));
#31561=CARTESIAN_POINT('Ctrl Pts',(13.6752954743875,-15.5,3.7994999999999));
#31562=CARTESIAN_POINT('Ctrl Pts',(14.1314716057906,-16.2901202367904,3.75783333333323));
#31563=CARTESIAN_POINT('Ctrl Pts',(14.5876477371938,-17.0802404735808,3.71616666666657));
#31564=CARTESIAN_POINT('Ctrl Pts',(15.5,-17.0802404735808,3.6744999999999));
#31565=CARTESIAN_POINT('Ctrl Pts',(16.4123522628062,-17.0802404735808,3.63283333333323));
#31566=CARTESIAN_POINT('Ctrl Pts',(16.8685283942094,-16.2901202367904,3.59116666666656));
#31567=CARTESIAN_POINT('Ctrl Pts',(17.3247045256125,-15.5,3.5494999999999));
#31568=CARTESIAN_POINT('Ctrl Pts',(16.8685283942094,-14.7098797632096,3.50783333333323));
#31569=CARTESIAN_POINT('Ctrl Pts',(16.4123522628062,-13.9197595264192,3.46616666666656));
#31570=CARTESIAN_POINT('Ctrl Pts',(15.5,-13.9197595264192,3.4244999999999));
#31571=CARTESIAN_POINT('Ctrl Pts',(14.5876477371938,-13.9197595264192,3.38283333333323));
#31572=CARTESIAN_POINT('Ctrl Pts',(14.1314716057906,-14.7098797632096,3.34116666666656));
#31573=CARTESIAN_POINT('Ctrl Pts',(13.6752954743875,-15.5,3.29949999999989));
#31574=CARTESIAN_POINT('Ctrl Pts',(14.1314716057906,-16.2901202367904,3.25783333333323));
#31575=CARTESIAN_POINT('Ctrl Pts',(14.5876477371938,-17.0802404735808,3.21616666666656));
#31576=CARTESIAN_POINT('Ctrl Pts',(15.5,-17.0802404735808,3.17449999999989));
#31577=CARTESIAN_POINT('Ctrl Pts',(16.4123522628062,-17.0802404735808,3.13283333333323));
#31578=CARTESIAN_POINT('Ctrl Pts',(16.8685283942094,-16.2901202367904,3.09116666666656));
#31579=CARTESIAN_POINT('Ctrl Pts',(17.3247045256125,-15.5,3.04949999999989));
#31580=CARTESIAN_POINT('Ctrl Pts',(16.8685283942094,-14.7098797632096,3.00783333333322));
#31581=CARTESIAN_POINT('Ctrl Pts',(16.4123522628062,-13.9197595264192,2.96616666666656));
#31582=CARTESIAN_POINT('Ctrl Pts',(15.5,-13.9197595264192,2.92449999999989));
#31583=CARTESIAN_POINT('Ctrl Pts',(14.5876477371938,-13.9197595264192,2.88283333333322));
#31584=CARTESIAN_POINT('Ctrl Pts',(14.1314716057906,-14.7098797632096,2.84116666666655));
#31585=CARTESIAN_POINT('Ctrl Pts',(13.6752954743875,-15.5,2.79949999999989));
#31586=CARTESIAN_POINT('Ctrl Pts',(14.1314716057906,-16.2901202367904,2.75783333333322));
#31587=CARTESIAN_POINT('Ctrl Pts',(14.5876477371938,-17.0802404735808,2.71616666666655));
#31588=CARTESIAN_POINT('Ctrl Pts',(15.5,-17.0802404735808,2.67449999999989));
#31589=CARTESIAN_POINT('Ctrl Pts',(16.4123522628062,-17.0802404735808,2.63283333333322));
#31590=CARTESIAN_POINT('Ctrl Pts',(16.8685283942094,-16.2901202367904,2.59116666666655));
#31591=CARTESIAN_POINT('Ctrl Pts',(17.3247045256125,-15.5,2.54949999999988));
#31592=CARTESIAN_POINT('Ctrl Pts',(16.8685283942094,-14.7098797632096,2.50783333333322));
#31593=CARTESIAN_POINT('Ctrl Pts',(16.4123522628062,-13.9197595264192,2.46616666666655));
#31594=CARTESIAN_POINT('Ctrl Pts',(15.5,-13.9197595264192,2.42449999999988));
#31595=CARTESIAN_POINT('Ctrl Pts',(14.5876477371938,-13.9197595264192,2.38283333333321));
#31596=CARTESIAN_POINT('Ctrl Pts',(14.1314716057906,-14.7098797632096,2.34116666666655));
#31597=CARTESIAN_POINT('Ctrl Pts',(13.6752954743875,-15.5,2.29949999999988));
#31598=CARTESIAN_POINT('Ctrl Pts',(14.1314716057906,-16.2901202367904,2.25783333333321));
#31599=CARTESIAN_POINT('Ctrl Pts',(14.5876477371938,-17.0802404735808,2.21616666666655));
#31600=CARTESIAN_POINT('Ctrl Pts',(15.5,-17.0802404735808,2.17449999999988));
#31601=CARTESIAN_POINT('Ctrl Pts',(16.4123522628062,-17.0802404735808,2.13283333333321));
#31602=CARTESIAN_POINT('Ctrl Pts',(16.8685283942094,-16.2901202367904,2.09116666666655));
#31603=CARTESIAN_POINT('Ctrl Pts',(17.3247045256125,-15.5,2.04949999999988));
#31604=CARTESIAN_POINT('Ctrl Pts',(16.8685283942094,-14.7098797632096,2.00783333333321));
#31605=CARTESIAN_POINT('Ctrl Pts',(16.4123522628062,-13.9197595264192,1.96616666666654));
#31606=CARTESIAN_POINT('Ctrl Pts',(15.5,-13.9197595264192,1.92449999999988));
#31607=CARTESIAN_POINT('Ctrl Pts',(14.5876477371938,-13.9197595264192,1.88283333333321));
#31608=CARTESIAN_POINT('Ctrl Pts',(14.1314716057906,-14.7098797632096,1.84116666666654));
#31609=CARTESIAN_POINT('Ctrl Pts',(13.6752954743875,-15.5,1.79949999999987));
#31610=CARTESIAN_POINT('Ctrl Pts',(14.1314716057906,-16.2901202367904,1.75783333333321));
#31611=CARTESIAN_POINT('Ctrl Pts',(14.5876477371938,-17.0802404735808,1.71616666666654));
#31612=CARTESIAN_POINT('Ctrl Pts',(15.5,-17.0802404735808,1.67449999999987));
#31613=CARTESIAN_POINT('Ctrl Pts',(16.4123522628062,-17.0802404735808,1.63283333333321));
#31614=CARTESIAN_POINT('Ctrl Pts',(16.8685283942094,-16.2901202367904,1.59116666666654));
#31615=CARTESIAN_POINT('Ctrl Pts',(17.3247045256125,-15.5,1.54949999999987));
#31616=CARTESIAN_POINT('Ctrl Pts',(16.8685283942094,-14.7098797632096,1.5078333333332));
#31617=CARTESIAN_POINT('Ctrl Pts',(16.4123522628062,-13.9197595264192,1.46616666666654));
#31618=CARTESIAN_POINT('Ctrl Pts',(15.5,-13.9197595264192,1.42449999999987));
#31619=CARTESIAN_POINT('Ctrl Pts',(14.5876477371938,-13.9197595264192,1.3828333333332));
#31620=CARTESIAN_POINT('Ctrl Pts',(14.1314716057906,-14.7098797632096,1.34116666666653));
#31621=CARTESIAN_POINT('Ctrl Pts',(13.6752954743875,-15.5,1.29949999999987));
#31622=CARTESIAN_POINT('Ctrl Pts',(14.1314716057906,-16.2901202367904,1.2578333333332));
#31623=CARTESIAN_POINT('Ctrl Pts',(14.5876477371938,-17.0802404735808,1.21616666666653));
#31624=CARTESIAN_POINT('Ctrl Pts',(15.5,-17.0802404735808,1.17449999999986));
#31625=CARTESIAN_POINT('Ctrl Pts',(16.4123522628062,-17.0802404735808,1.1328333333332));
#31626=CARTESIAN_POINT('Ctrl Pts',(16.8685283942094,-16.2901202367904,1.09116666666653));
#31627=CARTESIAN_POINT('Ctrl Pts',(17.3247045256125,-15.5,1.04949999999986));
#31628=CARTESIAN_POINT('Ctrl Pts',(16.8685283942094,-14.7098797632096,1.0078333333332));
#31629=CARTESIAN_POINT('Ctrl Pts',(16.4123522628062,-13.9197595264192,0.96616666666653));
#31630=CARTESIAN_POINT('Ctrl Pts',(15.5,-13.9197595264192,0.924499999999863));
#31631=CARTESIAN_POINT('Ctrl Pts',(14.5876477371938,-13.9197595264192,0.882833333333196));
#31632=CARTESIAN_POINT('Ctrl Pts',(14.1314716057906,-14.7098797632096,0.841166666666529));
#31633=CARTESIAN_POINT('Ctrl Pts',(13.6752954743875,-15.5,0.799499999999861));
#31634=CARTESIAN_POINT('Ctrl Pts',(14.1314716057906,-16.2901202367904,0.757833333333194));
#31635=CARTESIAN_POINT('Ctrl Pts',(14.5876477371938,-17.0802404735808,0.716166666666527));
#31636=CARTESIAN_POINT('Ctrl Pts',(15.5,-17.0802404735808,0.674499999999859));
#31637=CARTESIAN_POINT('Ctrl Pts',(16.4123522628062,-17.0802404735808,0.632833333333192));
#31638=CARTESIAN_POINT('Ctrl Pts',(16.8685283942094,-16.2901202367904,0.591166666666525));
#31639=CARTESIAN_POINT('Ctrl Pts',(17.3247045256125,-15.5,0.549499999999857));
#31640=CARTESIAN_POINT('Ctrl Pts',(16.8685283942094,-14.7098797632096,0.50783333333319));
#31641=CARTESIAN_POINT('Ctrl Pts',(16.4123522628062,-13.9197595264192,0.466166666666523));
#31642=CARTESIAN_POINT('Ctrl Pts',(15.5,-13.9197595264192,0.424499999999856));
#31643=CARTESIAN_POINT('Ctrl Pts',(14.5876477371938,-13.9197595264192,0.382833333333188));
#31644=CARTESIAN_POINT('Ctrl Pts',(14.1314716057906,-14.7098797632096,0.341166666666521));
#31645=CARTESIAN_POINT('Ctrl Pts',(13.6752954743875,-15.5,0.299499999999854));
#31646=CARTESIAN_POINT('Ctrl Pts',(14.1314716057906,-16.2901202367904,0.257833333333186));
#31647=CARTESIAN_POINT('Ctrl Pts',(14.5876477371938,-17.0802404735808,0.216166666666519));
#31648=CARTESIAN_POINT('Ctrl Pts',(15.5,-17.0802404735808,0.174499999999852));
#31649=CARTESIAN_POINT('Ctrl Pts',(16.4123522628062,-17.0802404735808,0.132833333333185));
#31650=CARTESIAN_POINT('Ctrl Pts',(16.8685283942094,-16.2901202367904,0.0911666666665173));
#31651=CARTESIAN_POINT('Ctrl Pts',(17.3247045256125,-15.5,0.04949999999985));
#31652=CARTESIAN_POINT('Ctrl Pts',(16.8685283942094,-14.7098797632096,0.00783333333318273));
#31653=CARTESIAN_POINT('Ctrl Pts',(16.4123522628062,-13.9197595264192,-0.0338333333334846));
#31654=CARTESIAN_POINT('Ctrl Pts',(15.5,-13.9197595264192,-0.0755000000001518));
#31655=CARTESIAN_POINT('Ctrl Pts',(14.5876477371938,-13.9197595264192,-0.117166666666817));
#31656=CARTESIAN_POINT('Ctrl Pts',(14.1314716057906,-14.7098797632096,-0.158833333333485));
#31657=CARTESIAN_POINT('Ctrl Pts',(13.6752954743875,-15.5,-0.200500000000152));
#31658=CARTESIAN_POINT('Ctrl Pts',(14.1314716057906,-16.2901202367904,-0.242166666666819));
#31659=CARTESIAN_POINT('Ctrl Pts',(14.5876477371938,-17.0802404735808,-0.283833333333486));
#31660=CARTESIAN_POINT('Ctrl Pts',(15.5,-17.0802404735808,-0.325500000000154));
#31661=CARTESIAN_POINT('Ctrl Pts',(16.4123522628062,-17.0802404735808,-0.367166666666821));
#31662=CARTESIAN_POINT('Ctrl Pts',(16.8685283942094,-16.2901202367904,-0.408833333333488));
#31663=CARTESIAN_POINT('Ctrl Pts',(17.3247045256125,-15.5,-0.450500000000156));
#31664=CARTESIAN_POINT('Ctrl Pts',(16.8685283942094,-14.7098797632096,-0.492166666666823));
#31665=CARTESIAN_POINT('Ctrl Pts',(16.4123522628062,-13.9197595264192,-0.53383333333349));
#31666=CARTESIAN_POINT('Ctrl Pts',(15.5,-13.9197595264192,-0.575500000000157));
#31667=CARTESIAN_POINT('Ctrl Pts',(14.5876477371938,-13.9197595264192,-0.617166666666825));
#31668=CARTESIAN_POINT('Ctrl Pts',(14.1314716057906,-14.7098797632096,-0.658833333333492));
#31669=CARTESIAN_POINT('Ctrl Pts',(13.6752954743875,-15.5,-0.700500000000159));
#31670=CARTESIAN_POINT('Ctrl Pts',(14.1314716057906,-16.2901202367904,-0.742166666666827));
#31671=CARTESIAN_POINT('Ctrl Pts',(14.5876477371938,-17.0802404735808,-0.783833333333494));
#31672=CARTESIAN_POINT('Ctrl Pts',(15.5,-17.0802404735808,-0.825500000000161));
#31673=CARTESIAN_POINT('Ctrl Pts',(16.4123522628062,-17.0802404735808,-0.867166666666829));
#31674=CARTESIAN_POINT('Ctrl Pts',(16.8685283942094,-16.2901202367904,-0.908833333333496));
#31675=CARTESIAN_POINT('Ctrl Pts',(17.3247045256125,-15.5,-0.950500000000163));
#31676=CARTESIAN_POINT('Ctrl Pts',(16.8685283942094,-14.7098797632096,-0.99216666666683));
#31677=CARTESIAN_POINT('Ctrl Pts',(16.4123522628062,-13.9197595264192,-1.0338333333335));
#31678=CARTESIAN_POINT('Ctrl Pts',(15.5,-13.9197595264192,-1.07550000000016));
#31679=CARTESIAN_POINT('Ctrl Pts',(14.5876477371938,-13.9197595264192,-1.11716666666683));
#31680=CARTESIAN_POINT('Ctrl Pts',(14.1314716057906,-14.7098797632096,-1.1588333333335));
#31681=CARTESIAN_POINT('Ctrl Pts',(13.6752954743875,-15.5,-1.20050000000017));
#31682=CARTESIAN_POINT('Ctrl Pts',(14.1314716057906,-16.2901202367904,-1.24216666666683));
#31683=CARTESIAN_POINT('Ctrl Pts',(14.5876477371938,-17.0802404735808,-1.2838333333335));
#31684=CARTESIAN_POINT('Ctrl Pts',(15.5,-17.0802404735808,-1.32550000000017));
#31685=CARTESIAN_POINT('Ctrl Pts',(16.4123522628062,-17.0802404735808,-1.36716666666683));
#31686=CARTESIAN_POINT('Ctrl Pts',(16.8685283942094,-16.2901202367904,-1.4088333333335));
#31687=CARTESIAN_POINT('Ctrl Pts',(17.3247045256125,-15.5,-1.45050000000017));
#31688=CARTESIAN_POINT('Ctrl Pts',(16.8685283942094,-14.7098797632096,-1.49216666666684));
#31689=CARTESIAN_POINT('Ctrl Pts',(16.4123522628062,-13.9197595264192,-1.5338333333335));
#31690=CARTESIAN_POINT('Ctrl Pts',(15.5,-13.9197595264192,-1.57550000000017));
#31691=CARTESIAN_POINT('Ctrl Pts',(14.5876477371938,-13.9197595264192,-1.61716666666684));
#31692=CARTESIAN_POINT('Ctrl Pts',(14.1314716057906,-14.7098797632096,-1.65883333333351));
#31693=CARTESIAN_POINT('Ctrl Pts',(13.6752954743875,-15.5,-1.70050000000017));
#31694=CARTESIAN_POINT('Ctrl Pts',(14.1314716057906,-16.2901202367904,-1.74216666666684));
#31695=CARTESIAN_POINT('Ctrl Pts',(14.5876477371938,-17.0802404735808,-1.78383333333351));
#31696=CARTESIAN_POINT('Ctrl Pts',(15.5,-17.0802404735808,-1.82550000000017));
#31697=CARTESIAN_POINT('Ctrl Pts',(16.4123522628062,-17.0802404735808,-1.86716666666684));
#31698=CARTESIAN_POINT('Ctrl Pts',(16.8685283942094,-16.2901202367904,-1.90883333333351));
#31699=CARTESIAN_POINT('Ctrl Pts',(17.3247045256125,-15.5,-1.95050000000018));
#31700=CARTESIAN_POINT('Ctrl Pts',(16.8685283942094,-14.7098797632096,-1.99216666666684));
#31701=CARTESIAN_POINT('Ctrl Pts',(16.700583153372,-14.4189900731899,-2.00750661517905));
#31702=CARTESIAN_POINT('Ctrl Pts',(16.4288420454487,-14.2215586016756,-2.02512262806106));
#31703=CARTESIAN_POINT('Ctrl Pts',(15.3465777998745,-13.4352476007234,-2.09528198318209));
#31704=CARTESIAN_POINT('Ctrl Pts',(14.2643135543003,-12.6489365997713,-2.16544133830312));
#31705=CARTESIAN_POINT('Ctrl Pts',(-17.0802317716412,-15.5000000000001,
11.1745050240672));
#31706=CARTESIAN_POINT('Ctrl Pts',(-17.0802317716412,-16.4123472387391,
11.1328383574005));
#31707=CARTESIAN_POINT('Ctrl Pts',(-16.2901158858206,-16.8685208581087,
11.0911716907338));
#31708=CARTESIAN_POINT('Ctrl Pts',(-15.4999999999999,-17.3246944774782,
11.0495050240672));
#31709=CARTESIAN_POINT('Ctrl Pts',(-14.7098841141793,-16.8685208581087,
11.0078383574005));
#31710=CARTESIAN_POINT('Ctrl Pts',(-13.9197682283587,-16.4123472387391,
10.9661716907338));
#31711=CARTESIAN_POINT('Ctrl Pts',(-13.9197682283587,-15.5,10.9245050240672));
#31712=CARTESIAN_POINT('Ctrl Pts',(-13.9197682283587,-14.587652761261,10.8828383574005));
#31713=CARTESIAN_POINT('Ctrl Pts',(-14.7098841141793,-14.1314791418915,
10.8411716907338));
#31714=CARTESIAN_POINT('Ctrl Pts',(-15.5,-13.6753055225219,10.7995050240672));
#31715=CARTESIAN_POINT('Ctrl Pts',(-16.2901158858206,-14.1314791418915,
10.7578383574005));
#31716=CARTESIAN_POINT('Ctrl Pts',(-17.0802317716412,-14.587652761261,10.7161716907338));
#31717=CARTESIAN_POINT('Ctrl Pts',(-17.0802317716412,-15.5000000000001,
10.6745050240672));
#31718=CARTESIAN_POINT('Ctrl Pts',(-17.0802317716412,-16.4123472387391,
10.6328383574005));
#31719=CARTESIAN_POINT('Ctrl Pts',(-16.2901158858206,-16.8685208581087,
10.5911716907338));
#31720=CARTESIAN_POINT('Ctrl Pts',(-15.4999999999999,-17.3246944774782,
10.5495050240672));
#31721=CARTESIAN_POINT('Ctrl Pts',(-14.7098841141793,-16.8685208581087,
10.5078383574005));
#31722=CARTESIAN_POINT('Ctrl Pts',(-13.9197682283587,-16.4123472387391,
10.4661716907338));
#31723=CARTESIAN_POINT('Ctrl Pts',(-13.9197682283587,-15.5,10.4245050240672));
#31724=CARTESIAN_POINT('Ctrl Pts',(-13.9197682283587,-14.587652761261,10.3828383574005));
#31725=CARTESIAN_POINT('Ctrl Pts',(-14.7098841141793,-14.1314791418915,
10.3411716907338));
#31726=CARTESIAN_POINT('Ctrl Pts',(-15.5,-13.6753055225219,10.2995050240672));
#31727=CARTESIAN_POINT('Ctrl Pts',(-16.2901158858206,-14.1314791418915,
10.2578383574005));
#31728=CARTESIAN_POINT('Ctrl Pts',(-17.0802317716412,-14.587652761261,10.2161716907338));
#31729=CARTESIAN_POINT('Ctrl Pts',(-17.0802317716412,-15.5000000000001,
10.1745050240672));
#31730=CARTESIAN_POINT('Ctrl Pts',(-17.0802317716412,-16.4123472387391,
10.1328383574005));
#31731=CARTESIAN_POINT('Ctrl Pts',(-16.2901158858206,-16.8685208581087,
10.0911716907338));
#31732=CARTESIAN_POINT('Ctrl Pts',(-15.4999999999999,-17.3246944774782,
10.0495050240672));
#31733=CARTESIAN_POINT('Ctrl Pts',(-14.7098841141793,-16.8685208581087,
10.0078383574005));
#31734=CARTESIAN_POINT('Ctrl Pts',(-13.9197682283587,-16.4123472387391,
9.96617169073382));
#31735=CARTESIAN_POINT('Ctrl Pts',(-13.9197682283587,-15.5,9.92450502406715));
#31736=CARTESIAN_POINT('Ctrl Pts',(-13.9197682283587,-14.587652761261,9.88283835740048));
#31737=CARTESIAN_POINT('Ctrl Pts',(-14.7098841141793,-14.1314791418915,
9.84117169073381));
#31738=CARTESIAN_POINT('Ctrl Pts',(-15.5,-13.6753055225219,9.79950502406715));
#31739=CARTESIAN_POINT('Ctrl Pts',(-16.2901158858206,-14.1314791418915,
9.75783835740048));
#31740=CARTESIAN_POINT('Ctrl Pts',(-17.0802317716412,-14.587652761261,9.71617169073381));
#31741=CARTESIAN_POINT('Ctrl Pts',(-17.0802317716412,-15.5000000000001,
9.67450502406715));
#31742=CARTESIAN_POINT('Ctrl Pts',(-17.0802317716412,-16.4123472387391,
9.63283835740048));
#31743=CARTESIAN_POINT('Ctrl Pts',(-16.2901158858206,-16.8685208581087,
9.59117169073381));
#31744=CARTESIAN_POINT('Ctrl Pts',(-15.4999999999999,-17.3246944774782,
9.54950502406714));
#31745=CARTESIAN_POINT('Ctrl Pts',(-14.7098841141793,-16.8685208581087,
9.50783835740048));
#31746=CARTESIAN_POINT('Ctrl Pts',(-13.9197682283587,-16.4123472387391,
9.46617169073381));
#31747=CARTESIAN_POINT('Ctrl Pts',(-13.9197682283587,-15.5,9.42450502406714));
#31748=CARTESIAN_POINT('Ctrl Pts',(-13.9197682283587,-14.587652761261,9.38283835740048));
#31749=CARTESIAN_POINT('Ctrl Pts',(-14.7098841141793,-14.1314791418915,
9.34117169073381));
#31750=CARTESIAN_POINT('Ctrl Pts',(-15.5,-13.6753055225219,9.29950502406714));
#31751=CARTESIAN_POINT('Ctrl Pts',(-16.2901158858206,-14.1314791418915,
9.25783835740048));
#31752=CARTESIAN_POINT('Ctrl Pts',(-17.0802317716412,-14.587652761261,9.21617169073381));
#31753=CARTESIAN_POINT('Ctrl Pts',(-17.0802317716412,-15.5000000000001,
9.17450502406714));
#31754=CARTESIAN_POINT('Ctrl Pts',(-17.0802317716412,-16.4123472387391,
9.13283835740048));
#31755=CARTESIAN_POINT('Ctrl Pts',(-16.2901158858206,-16.8685208581087,
9.09117169073381));
#31756=CARTESIAN_POINT('Ctrl Pts',(-15.4999999999999,-17.3246944774782,
9.04950502406714));
#31757=CARTESIAN_POINT('Ctrl Pts',(-14.7098841141793,-16.8685208581087,
9.00783835740047));
#31758=CARTESIAN_POINT('Ctrl Pts',(-13.9197682283587,-16.4123472387391,
8.9661716907338));
#31759=CARTESIAN_POINT('Ctrl Pts',(-13.9197682283587,-15.5,8.92450502406714));
#31760=CARTESIAN_POINT('Ctrl Pts',(-13.9197682283587,-14.587652761261,8.88283835740047));
#31761=CARTESIAN_POINT('Ctrl Pts',(-14.7098841141793,-14.1314791418915,
8.8411716907338));
#31762=CARTESIAN_POINT('Ctrl Pts',(-15.5,-13.6753055225219,8.79950502406714));
#31763=CARTESIAN_POINT('Ctrl Pts',(-16.2901158858206,-14.1314791418915,
8.75783835740047));
#31764=CARTESIAN_POINT('Ctrl Pts',(-17.0802317716412,-14.587652761261,8.7161716907338));
#31765=CARTESIAN_POINT('Ctrl Pts',(-17.0802317716412,-15.5000000000001,
8.67450502406713));
#31766=CARTESIAN_POINT('Ctrl Pts',(-17.0802317716412,-16.4123472387391,
8.63283835740047));
#31767=CARTESIAN_POINT('Ctrl Pts',(-16.2901158858206,-16.8685208581087,
8.5911716907338));
#31768=CARTESIAN_POINT('Ctrl Pts',(-15.4999999999999,-17.3246944774782,
8.54950502406713));
#31769=CARTESIAN_POINT('Ctrl Pts',(-14.7098841141793,-16.8685208581087,
8.50783835740046));
#31770=CARTESIAN_POINT('Ctrl Pts',(-13.9197682283587,-16.4123472387391,
8.4661716907338));
#31771=CARTESIAN_POINT('Ctrl Pts',(-13.9197682283587,-15.5,8.42450502406713));
#31772=CARTESIAN_POINT('Ctrl Pts',(-13.9197682283587,-14.587652761261,8.38283835740046));
#31773=CARTESIAN_POINT('Ctrl Pts',(-14.7098841141793,-14.1314791418915,
8.3411716907338));
#31774=CARTESIAN_POINT('Ctrl Pts',(-15.5,-13.6753055225219,8.29950502406713));
#31775=CARTESIAN_POINT('Ctrl Pts',(-16.2901158858206,-14.1314791418915,
8.25783835740046));
#31776=CARTESIAN_POINT('Ctrl Pts',(-17.0802317716412,-14.587652761261,8.21617169073379));
#31777=CARTESIAN_POINT('Ctrl Pts',(-17.0802317716412,-15.5000000000001,
8.17450502406713));
#31778=CARTESIAN_POINT('Ctrl Pts',(-17.0802317716412,-16.4123472387391,
8.13283835740046));
#31779=CARTESIAN_POINT('Ctrl Pts',(-16.2901158858206,-16.8685208581087,
8.09117169073379));
#31780=CARTESIAN_POINT('Ctrl Pts',(-15.4999999999999,-17.3246944774782,
8.04950502406713));
#31781=CARTESIAN_POINT('Ctrl Pts',(-14.7098841141793,-16.8685208581087,
8.00783835740046));
#31782=CARTESIAN_POINT('Ctrl Pts',(-13.9197682283587,-16.4123472387391,
7.96617169073379));
#31783=CARTESIAN_POINT('Ctrl Pts',(-13.9197682283587,-15.5,7.92450502406712));
#31784=CARTESIAN_POINT('Ctrl Pts',(-13.9197682283587,-14.587652761261,7.88283835740046));
#31785=CARTESIAN_POINT('Ctrl Pts',(-14.7098841141793,-14.1314791418915,
7.84117169073379));
#31786=CARTESIAN_POINT('Ctrl Pts',(-15.5,-13.6753055225219,7.79950502406712));
#31787=CARTESIAN_POINT('Ctrl Pts',(-16.2901158858206,-14.1314791418915,
7.75783835740046));
#31788=CARTESIAN_POINT('Ctrl Pts',(-17.0802317716412,-14.587652761261,7.71617169073379));
#31789=CARTESIAN_POINT('Ctrl Pts',(-17.0802317716412,-15.5000000000001,
7.67450502406712));
#31790=CARTESIAN_POINT('Ctrl Pts',(-17.0802317716412,-16.4123472387391,
7.63283835740045));
#31791=CARTESIAN_POINT('Ctrl Pts',(-16.2901158858206,-16.8685208581087,
7.59117169073379));
#31792=CARTESIAN_POINT('Ctrl Pts',(-15.4999999999999,-17.3246944774782,
7.54950502406712));
#31793=CARTESIAN_POINT('Ctrl Pts',(-14.7098841141793,-16.8685208581087,
7.50783835740045));
#31794=CARTESIAN_POINT('Ctrl Pts',(-13.9197682283587,-16.4123472387391,
7.46617169073379));
#31795=CARTESIAN_POINT('Ctrl Pts',(-13.9197682283587,-15.5,7.42450502406712));
#31796=CARTESIAN_POINT('Ctrl Pts',(-13.9197682283587,-14.587652761261,7.38283835740045));
#31797=CARTESIAN_POINT('Ctrl Pts',(-14.7098841141793,-14.1314791418915,
7.34117169073378));
#31798=CARTESIAN_POINT('Ctrl Pts',(-15.5,-13.6753055225219,7.29950502406712));
#31799=CARTESIAN_POINT('Ctrl Pts',(-16.2901158858206,-14.1314791418915,
7.25783835740045));
#31800=CARTESIAN_POINT('Ctrl Pts',(-17.0802317716412,-14.587652761261,7.21617169073378));
#31801=CARTESIAN_POINT('Ctrl Pts',(-17.0802317716412,-15.5000000000001,
7.17450502406711));
#31802=CARTESIAN_POINT('Ctrl Pts',(-17.0802317716412,-16.4123472387391,
7.13283835740044));
#31803=CARTESIAN_POINT('Ctrl Pts',(-16.2901158858206,-16.8685208581087,
7.09117169073378));
#31804=CARTESIAN_POINT('Ctrl Pts',(-15.4999999999999,-17.3246944774782,
7.04950502406711));
#31805=CARTESIAN_POINT('Ctrl Pts',(-14.7098841141793,-16.8685208581087,
7.00783835740045));
#31806=CARTESIAN_POINT('Ctrl Pts',(-13.9197682283587,-16.4123472387391,
6.96617169073378));
#31807=CARTESIAN_POINT('Ctrl Pts',(-13.9197682283587,-15.5,6.92450502406711));
#31808=CARTESIAN_POINT('Ctrl Pts',(-13.9197682283587,-14.587652761261,6.88283835740044));
#31809=CARTESIAN_POINT('Ctrl Pts',(-14.7098841141793,-14.1314791418915,
6.84117169073378));
#31810=CARTESIAN_POINT('Ctrl Pts',(-15.5,-13.6753055225219,6.79950502406711));
#31811=CARTESIAN_POINT('Ctrl Pts',(-16.2901158858206,-14.1314791418915,
6.75783835740044));
#31812=CARTESIAN_POINT('Ctrl Pts',(-17.0802317716412,-14.587652761261,6.71617169073377));
#31813=CARTESIAN_POINT('Ctrl Pts',(-17.0802317716412,-15.5000000000001,
6.67450502406711));
#31814=CARTESIAN_POINT('Ctrl Pts',(-17.0802317716412,-16.4123472387391,
6.63283835740044));
#31815=CARTESIAN_POINT('Ctrl Pts',(-16.2901158858206,-16.8685208581087,
6.59117169073377));
#31816=CARTESIAN_POINT('Ctrl Pts',(-15.4999999999999,-17.3246944774782,
6.5495050240671));
#31817=CARTESIAN_POINT('Ctrl Pts',(-14.7098841141793,-16.8685208581087,
6.50783835740044));
#31818=CARTESIAN_POINT('Ctrl Pts',(-13.9197682283587,-16.4123472387391,
6.46617169073377));
#31819=CARTESIAN_POINT('Ctrl Pts',(-13.9197682283587,-15.5,6.4245050240671));
#31820=CARTESIAN_POINT('Ctrl Pts',(-13.9197682283587,-14.587652761261,6.38283835740044));
#31821=CARTESIAN_POINT('Ctrl Pts',(-14.7098841141793,-14.1314791418915,
6.34117169073377));
#31822=CARTESIAN_POINT('Ctrl Pts',(-15.5,-13.6753055225219,6.2995050240671));
#31823=CARTESIAN_POINT('Ctrl Pts',(-16.2901158858206,-14.1314791418915,
6.25783835740044));
#31824=CARTESIAN_POINT('Ctrl Pts',(-17.0802317716412,-14.587652761261,6.21617169073377));
#31825=CARTESIAN_POINT('Ctrl Pts',(-17.0802317716412,-15.5000000000001,
6.1745050240671));
#31826=CARTESIAN_POINT('Ctrl Pts',(-17.0802317716412,-16.4123472387391,
6.13283835740043));
#31827=CARTESIAN_POINT('Ctrl Pts',(-16.2901158858206,-16.8685208581087,
6.09117169073377));
#31828=CARTESIAN_POINT('Ctrl Pts',(-15.4999999999999,-17.3246944774782,
6.0495050240671));
#31829=CARTESIAN_POINT('Ctrl Pts',(-14.7098841141793,-16.8685208581087,
6.00783835740043));
#31830=CARTESIAN_POINT('Ctrl Pts',(-13.9197682283587,-16.4123472387391,
5.96617169073376));
#31831=CARTESIAN_POINT('Ctrl Pts',(-13.9197682283587,-15.5,5.9245050240671));
#31832=CARTESIAN_POINT('Ctrl Pts',(-13.9197682283587,-14.587652761261,5.88283835740043));
#31833=CARTESIAN_POINT('Ctrl Pts',(-14.7098841141793,-14.1314791418915,
5.84117169073376));
#31834=CARTESIAN_POINT('Ctrl Pts',(-15.5,-13.6753055225219,5.79950502406709));
#31835=CARTESIAN_POINT('Ctrl Pts',(-16.2901158858206,-14.1314791418915,
5.75783835740043));
#31836=CARTESIAN_POINT('Ctrl Pts',(-17.0802317716412,-14.587652761261,5.71617169073376));
#31837=CARTESIAN_POINT('Ctrl Pts',(-17.0802317716412,-15.5000000000001,
5.67450502406709));
#31838=CARTESIAN_POINT('Ctrl Pts',(-17.0802317716412,-16.4123472387391,
5.63283835740043));
#31839=CARTESIAN_POINT('Ctrl Pts',(-16.2901158858206,-16.8685208581087,
5.59117169073376));
#31840=CARTESIAN_POINT('Ctrl Pts',(-15.4999999999999,-17.3246944774782,
5.54950502406709));
#31841=CARTESIAN_POINT('Ctrl Pts',(-14.7098841141793,-16.8685208581087,
5.50783835740043));
#31842=CARTESIAN_POINT('Ctrl Pts',(-13.9197682283587,-16.4123472387391,
5.46617169073376));
#31843=CARTESIAN_POINT('Ctrl Pts',(-13.9197682283587,-15.5,5.42450502406709));
#31844=CARTESIAN_POINT('Ctrl Pts',(-13.9197682283587,-14.587652761261,5.38283835740042));
#31845=CARTESIAN_POINT('Ctrl Pts',(-14.7098841141793,-14.1314791418915,
5.34117169073376));
#31846=CARTESIAN_POINT('Ctrl Pts',(-15.5,-13.6753055225219,5.29950502406709));
#31847=CARTESIAN_POINT('Ctrl Pts',(-16.2901158858206,-14.1314791418915,
5.25783835740042));
#31848=CARTESIAN_POINT('Ctrl Pts',(-17.0802317716412,-14.587652761261,5.21617169073375));
#31849=CARTESIAN_POINT('Ctrl Pts',(-17.0802317716412,-15.5000000000001,
5.17450502406709));
#31850=CARTESIAN_POINT('Ctrl Pts',(-17.0802317716412,-16.4123472387391,
5.13283835740042));
#31851=CARTESIAN_POINT('Ctrl Pts',(-16.2901158858206,-16.8685208581087,
5.09117169073375));
#31852=CARTESIAN_POINT('Ctrl Pts',(-15.4999999999999,-17.3246944774782,
5.04950502406708));
#31853=CARTESIAN_POINT('Ctrl Pts',(-14.7098841141793,-16.8685208581087,
5.00783835740042));
#31854=CARTESIAN_POINT('Ctrl Pts',(-13.9197682283587,-16.4123472387391,
4.96617169073375));
#31855=CARTESIAN_POINT('Ctrl Pts',(-13.9197682283587,-15.5,4.92450502406708));
#31856=CARTESIAN_POINT('Ctrl Pts',(-13.9197682283587,-14.587652761261,4.88283835740042));
#31857=CARTESIAN_POINT('Ctrl Pts',(-14.7098841141793,-14.1314791418915,
4.84117169073375));
#31858=CARTESIAN_POINT('Ctrl Pts',(-15.5,-13.6753055225219,4.79950502406708));
#31859=CARTESIAN_POINT('Ctrl Pts',(-16.2901158858206,-14.1314791418915,
4.75783835740041));
#31860=CARTESIAN_POINT('Ctrl Pts',(-17.0802317716412,-14.587652761261,4.71617169073375));
#31861=CARTESIAN_POINT('Ctrl Pts',(-17.0802317716412,-15.5000000000001,
4.67450502406708));
#31862=CARTESIAN_POINT('Ctrl Pts',(-17.0802317716412,-16.4123472387391,
4.63283835740041));
#31863=CARTESIAN_POINT('Ctrl Pts',(-16.2901158858206,-16.8685208581087,
4.59117169073374));
#31864=CARTESIAN_POINT('Ctrl Pts',(-15.4999999999999,-17.3246944774782,
4.54950502406708));
#31865=CARTESIAN_POINT('Ctrl Pts',(-14.7098841141793,-16.8685208581087,
4.50783835740041));
#31866=CARTESIAN_POINT('Ctrl Pts',(-13.9197682283587,-16.4123472387391,
4.46617169073374));
#31867=CARTESIAN_POINT('Ctrl Pts',(-13.9197682283587,-15.5,4.42450502406708));
#31868=CARTESIAN_POINT('Ctrl Pts',(-13.9197682283587,-14.587652761261,4.38283835740041));
#31869=CARTESIAN_POINT('Ctrl Pts',(-14.7098841141793,-14.1314791418915,
4.34117169073374));
#31870=CARTESIAN_POINT('Ctrl Pts',(-15.5,-13.6753055225219,4.29950502406708));
#31871=CARTESIAN_POINT('Ctrl Pts',(-16.2901158858206,-14.1314791418915,
4.25783835740041));
#31872=CARTESIAN_POINT('Ctrl Pts',(-17.0802317716412,-14.587652761261,4.21617169073374));
#31873=CARTESIAN_POINT('Ctrl Pts',(-17.0802317716412,-15.5000000000001,
4.17450502406707));
#31874=CARTESIAN_POINT('Ctrl Pts',(-17.0802317716412,-16.4123472387391,
4.13283835740041));
#31875=CARTESIAN_POINT('Ctrl Pts',(-16.2901158858206,-16.8685208581087,
4.09117169073374));
#31876=CARTESIAN_POINT('Ctrl Pts',(-15.4999999999999,-17.3246944774782,
4.04950502406707));
#31877=CARTESIAN_POINT('Ctrl Pts',(-14.7098841141793,-16.8685208581087,
4.0078383574004));
#31878=CARTESIAN_POINT('Ctrl Pts',(-13.9197682283587,-16.4123472387391,
3.96617169073374));
#31879=CARTESIAN_POINT('Ctrl Pts',(-13.9197682283587,-15.5,3.92450502406707));
#31880=CARTESIAN_POINT('Ctrl Pts',(-13.9197682283587,-14.587652761261,3.8828383574004));
#31881=CARTESIAN_POINT('Ctrl Pts',(-14.7098841141793,-14.1314791418915,
3.84117169073374));
#31882=CARTESIAN_POINT('Ctrl Pts',(-15.5,-13.6753055225219,3.79950502406707));
#31883=CARTESIAN_POINT('Ctrl Pts',(-16.2901158858206,-14.1314791418915,
3.7578383574004));
#31884=CARTESIAN_POINT('Ctrl Pts',(-17.0802317716412,-14.587652761261,3.71617169073373));
#31885=CARTESIAN_POINT('Ctrl Pts',(-17.0802317716412,-15.5000000000001,
3.67450502406707));
#31886=CARTESIAN_POINT('Ctrl Pts',(-17.0802317716412,-16.4123472387391,
3.6328383574004));
#31887=CARTESIAN_POINT('Ctrl Pts',(-16.2901158858206,-16.8685208581087,
3.59117169073373));
#31888=CARTESIAN_POINT('Ctrl Pts',(-15.4999999999999,-17.3246944774782,
3.54950502406707));
#31889=CARTESIAN_POINT('Ctrl Pts',(-14.7098841141793,-16.8685208581087,
3.5078383574004));
#31890=CARTESIAN_POINT('Ctrl Pts',(-13.9197682283587,-16.4123472387391,
3.46617169073373));
#31891=CARTESIAN_POINT('Ctrl Pts',(-13.9197682283587,-15.5,3.42450502406706));
#31892=CARTESIAN_POINT('Ctrl Pts',(-13.9197682283587,-14.587652761261,3.3828383574004));
#31893=CARTESIAN_POINT('Ctrl Pts',(-14.7098841141793,-14.1314791418915,
3.34117169073373));
#31894=CARTESIAN_POINT('Ctrl Pts',(-15.5,-13.6753055225219,3.29950502406706));
#31895=CARTESIAN_POINT('Ctrl Pts',(-16.2901158858206,-14.1314791418915,
3.2578383574004));
#31896=CARTESIAN_POINT('Ctrl Pts',(-17.0802317716412,-14.587652761261,3.21617169073373));
#31897=CARTESIAN_POINT('Ctrl Pts',(-17.0802317716412,-15.5000000000001,
3.17450502406706));
#31898=CARTESIAN_POINT('Ctrl Pts',(-17.0802317716412,-16.4123472387391,
3.13283835740039));
#31899=CARTESIAN_POINT('Ctrl Pts',(-16.2901158858206,-16.8685208581087,
3.09117169073373));
#31900=CARTESIAN_POINT('Ctrl Pts',(-15.4999999999999,-17.3246944774782,
3.04950502406706));
#31901=CARTESIAN_POINT('Ctrl Pts',(-14.7098841141793,-16.8685208581087,
3.00783835740039));
#31902=CARTESIAN_POINT('Ctrl Pts',(-13.9197682283587,-16.4123472387391,
2.96617169073372));
#31903=CARTESIAN_POINT('Ctrl Pts',(-13.9197682283587,-15.5,2.92450502406706));
#31904=CARTESIAN_POINT('Ctrl Pts',(-13.9197682283587,-14.587652761261,2.88283835740039));
#31905=CARTESIAN_POINT('Ctrl Pts',(-14.7098841141793,-14.1314791418915,
2.84117169073372));
#31906=CARTESIAN_POINT('Ctrl Pts',(-15.5,-13.6753055225219,2.79950502406705));
#31907=CARTESIAN_POINT('Ctrl Pts',(-16.2901158858206,-14.1314791418915,
2.75783835740039));
#31908=CARTESIAN_POINT('Ctrl Pts',(-17.0802317716412,-14.587652761261,2.71617169073372));
#31909=CARTESIAN_POINT('Ctrl Pts',(-17.0802317716412,-15.5000000000001,
2.67450502406705));
#31910=CARTESIAN_POINT('Ctrl Pts',(-17.0802317716412,-16.4123472387391,
2.63283835740039));
#31911=CARTESIAN_POINT('Ctrl Pts',(-16.2901158858206,-16.8685208581087,
2.59117169073372));
#31912=CARTESIAN_POINT('Ctrl Pts',(-15.4999999999999,-17.3246944774782,
2.54950502406705));
#31913=CARTESIAN_POINT('Ctrl Pts',(-14.7098841141793,-16.8685208581087,
2.50783835740038));
#31914=CARTESIAN_POINT('Ctrl Pts',(-13.9197682283587,-16.4123472387391,
2.46617169073372));
#31915=CARTESIAN_POINT('Ctrl Pts',(-13.9197682283587,-15.5,2.42450502406705));
#31916=CARTESIAN_POINT('Ctrl Pts',(-13.9197682283587,-14.587652761261,2.38283835740038));
#31917=CARTESIAN_POINT('Ctrl Pts',(-14.7098841141793,-14.1314791418915,
2.34117169073371));
#31918=CARTESIAN_POINT('Ctrl Pts',(-15.5,-13.6753055225219,2.29950502406705));
#31919=CARTESIAN_POINT('Ctrl Pts',(-16.2901158858206,-14.1314791418915,
2.25783835740038));
#31920=CARTESIAN_POINT('Ctrl Pts',(-17.0802317716412,-14.587652761261,2.21617169073371));
#31921=CARTESIAN_POINT('Ctrl Pts',(-17.0802317716412,-15.5000000000001,
2.17450502406705));
#31922=CARTESIAN_POINT('Ctrl Pts',(-17.0802317716412,-16.4123472387391,
2.13283835740038));
#31923=CARTESIAN_POINT('Ctrl Pts',(-16.2901158858206,-16.8685208581087,
2.09117169073371));
#31924=CARTESIAN_POINT('Ctrl Pts',(-15.4999999999999,-17.3246944774782,
2.04950502406705));
#31925=CARTESIAN_POINT('Ctrl Pts',(-14.7098841141793,-16.8685208581087,
2.00783835740038));
#31926=CARTESIAN_POINT('Ctrl Pts',(-13.9197682283587,-16.4123472387391,
1.96617169073371));
#31927=CARTESIAN_POINT('Ctrl Pts',(-13.9197682283587,-15.5,1.92450502406704));
#31928=CARTESIAN_POINT('Ctrl Pts',(-13.9197682283587,-14.587652761261,1.88283835740038));
#31929=CARTESIAN_POINT('Ctrl Pts',(-14.7098841141793,-14.1314791418915,
1.84117169073371));
#31930=CARTESIAN_POINT('Ctrl Pts',(-15.5,-13.6753055225219,1.79950502406704));
#31931=CARTESIAN_POINT('Ctrl Pts',(-16.2901158858206,-14.1314791418915,
1.75783835740037));
#31932=CARTESIAN_POINT('Ctrl Pts',(-17.0802317716412,-14.587652761261,1.71617169073371));
#31933=CARTESIAN_POINT('Ctrl Pts',(-17.0802317716412,-15.5000000000001,
1.67450502406704));
#31934=CARTESIAN_POINT('Ctrl Pts',(-17.0802317716412,-16.4123472387391,
1.63283835740037));
#31935=CARTESIAN_POINT('Ctrl Pts',(-16.2901158858206,-16.8685208581087,
1.59117169073371));
#31936=CARTESIAN_POINT('Ctrl Pts',(-15.4999999999999,-17.3246944774782,
1.54950502406704));
#31937=CARTESIAN_POINT('Ctrl Pts',(-14.7098841141793,-16.8685208581087,
1.50783835740037));
#31938=CARTESIAN_POINT('Ctrl Pts',(-13.9197682283587,-16.4123472387391,
1.4661716907337));
#31939=CARTESIAN_POINT('Ctrl Pts',(-13.9197682283587,-15.5,1.42450502406704));
#31940=CARTESIAN_POINT('Ctrl Pts',(-13.9197682283587,-14.587652761261,1.38283835740037));
#31941=CARTESIAN_POINT('Ctrl Pts',(-14.7098841141793,-14.1314791418915,
1.3411716907337));
#31942=CARTESIAN_POINT('Ctrl Pts',(-15.5,-13.6753055225219,1.29950502406703));
#31943=CARTESIAN_POINT('Ctrl Pts',(-16.2901158858206,-14.1314791418915,
1.25783835740037));
#31944=CARTESIAN_POINT('Ctrl Pts',(-17.0802317716412,-14.587652761261,1.2161716907337));
#31945=CARTESIAN_POINT('Ctrl Pts',(-17.0802317716412,-15.5000000000001,
1.17450502406703));
#31946=CARTESIAN_POINT('Ctrl Pts',(-17.0802317716412,-16.4123472387391,
1.13283835740037));
#31947=CARTESIAN_POINT('Ctrl Pts',(-16.2901158858206,-16.8685208581087,
1.0911716907337));
#31948=CARTESIAN_POINT('Ctrl Pts',(-15.4999999999999,-17.3246944774782,
1.04950502406703));
#31949=CARTESIAN_POINT('Ctrl Pts',(-14.7098841141793,-16.8685208581087,
1.00783835740037));
#31950=CARTESIAN_POINT('Ctrl Pts',(-13.9197682283587,-16.4123472387391,
0.966171690733698));
#31951=CARTESIAN_POINT('Ctrl Pts',(-13.9197682283587,-15.5,0.92450502406703));
#31952=CARTESIAN_POINT('Ctrl Pts',(-13.9197682283587,-14.587652761261,0.882838357400363));
#31953=CARTESIAN_POINT('Ctrl Pts',(-14.7098841141793,-14.1314791418915,
0.841171690733696));
#31954=CARTESIAN_POINT('Ctrl Pts',(-15.5,-13.6753055225219,0.799505024067029));
#31955=CARTESIAN_POINT('Ctrl Pts',(-16.2901158858206,-14.1314791418915,
0.757838357400361));
#31956=CARTESIAN_POINT('Ctrl Pts',(-17.0802317716412,-14.587652761261,0.716171690733694));
#31957=CARTESIAN_POINT('Ctrl Pts',(-17.0802317716412,-15.5000000000001,
0.674505024067027));
#31958=CARTESIAN_POINT('Ctrl Pts',(-17.0802317716412,-16.4123472387391,
0.632838357400359));
#31959=CARTESIAN_POINT('Ctrl Pts',(-16.2901158858206,-16.8685208581087,
0.591171690733692));
#31960=CARTESIAN_POINT('Ctrl Pts',(-15.4999999999999,-17.3246944774782,
0.549505024067025));
#31961=CARTESIAN_POINT('Ctrl Pts',(-14.7098841141793,-16.8685208581087,
0.507838357400358));
#31962=CARTESIAN_POINT('Ctrl Pts',(-13.9197682283587,-16.4123472387391,
0.46617169073369));
#31963=CARTESIAN_POINT('Ctrl Pts',(-13.9197682283587,-15.5,0.424505024067023));
#31964=CARTESIAN_POINT('Ctrl Pts',(-13.9197682283587,-14.587652761261,0.382838357400356));
#31965=CARTESIAN_POINT('Ctrl Pts',(-14.7098841141793,-14.1314791418915,
0.341171690733688));
#31966=CARTESIAN_POINT('Ctrl Pts',(-15.5,-13.6753055225219,0.299505024067021));
#31967=CARTESIAN_POINT('Ctrl Pts',(-16.2901158858206,-14.1314791418915,
0.257838357400354));
#31968=CARTESIAN_POINT('Ctrl Pts',(-17.0802317716412,-14.587652761261,0.216171690733687));
#31969=CARTESIAN_POINT('Ctrl Pts',(-17.0802317716412,-15.5000000000001,
0.174505024067019));
#31970=CARTESIAN_POINT('Ctrl Pts',(-17.0802317716412,-16.4123472387391,
0.132838357400352));
#31971=CARTESIAN_POINT('Ctrl Pts',(-16.2901158858206,-16.8685208581087,
0.0911716907336848));
#31972=CARTESIAN_POINT('Ctrl Pts',(-15.4999999999999,-17.3246944774782,
0.0495050240670175));
#31973=CARTESIAN_POINT('Ctrl Pts',(-14.7098841141793,-16.8685208581087,
0.0078383574003502));
#31974=CARTESIAN_POINT('Ctrl Pts',(-13.9197682283587,-16.4123472387391,
-0.0338283092663171));
#31975=CARTESIAN_POINT('Ctrl Pts',(-13.9197682283587,-15.5,-0.0754949759329844));
#31976=CARTESIAN_POINT('Ctrl Pts',(-13.9197682283587,-14.587652761261,-0.11716164259965));
#31977=CARTESIAN_POINT('Ctrl Pts',(-14.7098841141793,-14.1314791418915,
-0.158828309266317));
#31978=CARTESIAN_POINT('Ctrl Pts',(-15.5,-13.6753055225219,-0.200494975932985));
#31979=CARTESIAN_POINT('Ctrl Pts',(-16.2901158858206,-14.1314791418915,
-0.242161642599652));
#31980=CARTESIAN_POINT('Ctrl Pts',(-17.0802317716412,-14.587652761261,-0.283828309266319));
#31981=CARTESIAN_POINT('Ctrl Pts',(-17.0802317716412,-15.5000000000001,
-0.325494975932986));
#31982=CARTESIAN_POINT('Ctrl Pts',(-17.0802317716412,-16.4123472387391,
-0.367161642599654));
#31983=CARTESIAN_POINT('Ctrl Pts',(-16.2901158858206,-16.8685208581087,
-0.408828309266321));
#31984=CARTESIAN_POINT('Ctrl Pts',(-15.4999999999999,-17.3246944774782,
-0.450494975932988));
#31985=CARTESIAN_POINT('Ctrl Pts',(-14.7098841141793,-16.8685208581087,
-0.492161642599655));
#31986=CARTESIAN_POINT('Ctrl Pts',(-13.9197682283587,-16.4123472387391,
-0.533828309266323));
#31987=CARTESIAN_POINT('Ctrl Pts',(-13.9197682283587,-15.5,-0.57549497593299));
#31988=CARTESIAN_POINT('Ctrl Pts',(-13.9197682283587,-14.587652761261,-0.617161642599657));
#31989=CARTESIAN_POINT('Ctrl Pts',(-14.7098841141793,-14.1314791418915,
-0.658828309266325));
#31990=CARTESIAN_POINT('Ctrl Pts',(-15.5,-13.6753055225219,-0.700494975932992));
#31991=CARTESIAN_POINT('Ctrl Pts',(-16.2901158858206,-14.1314791418915,
-0.742161642599659));
#31992=CARTESIAN_POINT('Ctrl Pts',(-17.0802317716412,-14.587652761261,-0.783828309266327));
#31993=CARTESIAN_POINT('Ctrl Pts',(-17.0802317716412,-15.5000000000001,
-0.825494975932993));
#31994=CARTESIAN_POINT('Ctrl Pts',(-17.0802317716412,-16.4123472387391,
-0.867161642599661));
#31995=CARTESIAN_POINT('Ctrl Pts',(-16.2901158858206,-16.8685208581087,
-0.908828309266328));
#31996=CARTESIAN_POINT('Ctrl Pts',(-15.4999999999999,-17.3246944774782,
-0.950494975932996));
#31997=CARTESIAN_POINT('Ctrl Pts',(-14.7098841141793,-16.8685208581087,
-0.992161642599663));
#31998=CARTESIAN_POINT('Ctrl Pts',(-13.9197682283587,-16.4123472387391,
-1.03382830926633));
#31999=CARTESIAN_POINT('Ctrl Pts',(-13.9197682283587,-15.5,-1.075494975933));
#32000=CARTESIAN_POINT('Ctrl Pts',(-13.9197682283587,-14.587652761261,-1.11716164259966));
#32001=CARTESIAN_POINT('Ctrl Pts',(-14.7098841141793,-14.1314791418915,
-1.15882830926633));
#32002=CARTESIAN_POINT('Ctrl Pts',(-15.5,-13.6753055225219,-1.200494975933));
#32003=CARTESIAN_POINT('Ctrl Pts',(-16.2901158858206,-14.1314791418915,
-1.24216164259967));
#32004=CARTESIAN_POINT('Ctrl Pts',(-17.0802317716412,-14.587652761261,-1.28382830926633));
#32005=CARTESIAN_POINT('Ctrl Pts',(-17.0802317716412,-15.5000000000001,
-1.325494975933));
#32006=CARTESIAN_POINT('Ctrl Pts',(-17.0802317716412,-16.4123472387391,
-1.36716164259967));
#32007=CARTESIAN_POINT('Ctrl Pts',(-16.2901158858206,-16.8685208581087,
-1.40882830926633));
#32008=CARTESIAN_POINT('Ctrl Pts',(-15.4999999999999,-17.3246944774782,
-1.450494975933));
#32009=CARTESIAN_POINT('Ctrl Pts',(-14.7098841141793,-16.8685208581087,
-1.49216164259967));
#32010=CARTESIAN_POINT('Ctrl Pts',(-13.9197682283587,-16.4123472387391,
-1.53382830926634));
#32011=CARTESIAN_POINT('Ctrl Pts',(-13.9197682283587,-15.5,-1.575494975933));
#32012=CARTESIAN_POINT('Ctrl Pts',(-13.9197682283587,-14.587652761261,-1.61716164259967));
#32013=CARTESIAN_POINT('Ctrl Pts',(-14.7098841141793,-14.1314791418915,
-1.65882830926634));
#32014=CARTESIAN_POINT('Ctrl Pts',(-15.5,-13.6753055225219,-1.70049497593301));
#32015=CARTESIAN_POINT('Ctrl Pts',(-16.2901158858206,-14.1314791418915,
-1.74216164259967));
#32016=CARTESIAN_POINT('Ctrl Pts',(-17.0802317716412,-14.587652761261,-1.78382830926634));
#32017=CARTESIAN_POINT('Ctrl Pts',(-17.0802317716412,-15.5000000000001,
-1.82549497593301));
#32018=CARTESIAN_POINT('Ctrl Pts',(-17.0802317716412,-16.4123472387391,
-1.86716164259967));
#32019=CARTESIAN_POINT('Ctrl Pts',(-16.2901158858206,-16.8685208581087,
-1.90882830926634));
#32020=CARTESIAN_POINT('Ctrl Pts',(-15.4999999999999,-17.3246944774782,
-1.95049497593301));
#32021=CARTESIAN_POINT('Ctrl Pts',(-14.7098841141793,-16.8685208581087,
-1.99216164259968));
#32022=CARTESIAN_POINT('Ctrl Pts',(-14.4189893226643,-16.7005726719216,
-2.00750194461187));
#32023=CARTESIAN_POINT('Ctrl Pts',(-14.2215569357651,-16.4288249477778,
-2.02511838079831));
#32024=CARTESIAN_POINT('Ctrl Pts',(-17.4320632938682,-15.5000000000001,
10.971375));
#32025=CARTESIAN_POINT('Ctrl Pts',(-17.4320632938682,-16.6154772628063,
10.9297083333333));
#32026=CARTESIAN_POINT('Ctrl Pts',(-16.4660316469341,-17.1732158942094,
10.8880416666667));
#32027=CARTESIAN_POINT('Ctrl Pts',(-15.4999999999999,-17.7309545256125,
10.846375));
#32028=CARTESIAN_POINT('Ctrl Pts',(-14.5339683530658,-17.1732158942094,
10.8047083333333));
#32029=CARTESIAN_POINT('Ctrl Pts',(-13.5679367061317,-16.6154772628063,
10.7630416666667));
#32030=CARTESIAN_POINT('Ctrl Pts',(-13.5679367061317,-15.5,10.721375));
#32031=CARTESIAN_POINT('Ctrl Pts',(-13.5679367061317,-14.3845227371938,
10.6797083333333));
#32032=CARTESIAN_POINT('Ctrl Pts',(-14.5339683530658,-13.8267841057907,
10.6380416666667));
#32033=CARTESIAN_POINT('Ctrl Pts',(-15.5,-13.2690454743876,10.596375));
#32034=CARTESIAN_POINT('Ctrl Pts',(-16.4660316469341,-13.8267841057907,
10.5547083333333));
#32035=CARTESIAN_POINT('Ctrl Pts',(-17.4320632938682,-14.3845227371938,
10.5130416666667));
#32036=CARTESIAN_POINT('Ctrl Pts',(-17.4320632938682,-15.5000000000001,
10.471375));
#32037=CARTESIAN_POINT('Ctrl Pts',(-17.4320632938682,-16.6154772628063,
10.4297083333333));
#32038=CARTESIAN_POINT('Ctrl Pts',(-16.4660316469341,-17.1732158942094,
10.3880416666667));
#32039=CARTESIAN_POINT('Ctrl Pts',(-15.4999999999999,-17.7309545256125,
10.346375));
#32040=CARTESIAN_POINT('Ctrl Pts',(-14.5339683530658,-17.1732158942094,
10.3047083333333));
#32041=CARTESIAN_POINT('Ctrl Pts',(-13.5679367061317,-16.6154772628063,
10.2630416666667));
#32042=CARTESIAN_POINT('Ctrl Pts',(-13.5679367061317,-15.5,10.221375));
#32043=CARTESIAN_POINT('Ctrl Pts',(-13.5679367061317,-14.3845227371938,
10.1797083333333));
#32044=CARTESIAN_POINT('Ctrl Pts',(-14.5339683530658,-13.8267841057907,
10.1380416666667));
#32045=CARTESIAN_POINT('Ctrl Pts',(-15.5,-13.2690454743876,10.096375));
#32046=CARTESIAN_POINT('Ctrl Pts',(-16.4660316469341,-13.8267841057907,
10.0547083333333));
#32047=CARTESIAN_POINT('Ctrl Pts',(-17.4320632938682,-14.3845227371938,
10.0130416666666));
#32048=CARTESIAN_POINT('Ctrl Pts',(-17.4320632938682,-15.5000000000001,
9.97137499999998));
#32049=CARTESIAN_POINT('Ctrl Pts',(-17.4320632938682,-16.6154772628063,
9.92970833333332));
#32050=CARTESIAN_POINT('Ctrl Pts',(-16.4660316469341,-17.1732158942094,
9.88804166666665));
#32051=CARTESIAN_POINT('Ctrl Pts',(-15.4999999999999,-17.7309545256125,
9.84637499999998));
#32052=CARTESIAN_POINT('Ctrl Pts',(-14.5339683530658,-17.1732158942094,
9.80470833333331));
#32053=CARTESIAN_POINT('Ctrl Pts',(-13.5679367061317,-16.6154772628063,
9.76304166666665));
#32054=CARTESIAN_POINT('Ctrl Pts',(-13.5679367061317,-15.5,9.72137499999998));
#32055=CARTESIAN_POINT('Ctrl Pts',(-13.5679367061317,-14.3845227371938,
9.67970833333331));
#32056=CARTESIAN_POINT('Ctrl Pts',(-14.5339683530658,-13.8267841057907,
9.63804166666664));
#32057=CARTESIAN_POINT('Ctrl Pts',(-15.5,-13.2690454743876,9.59637499999998));
#32058=CARTESIAN_POINT('Ctrl Pts',(-16.4660316469341,-13.8267841057907,
9.55470833333331));
#32059=CARTESIAN_POINT('Ctrl Pts',(-17.4320632938682,-14.3845227371938,
9.51304166666664));
#32060=CARTESIAN_POINT('Ctrl Pts',(-17.4320632938682,-15.5000000000001,
9.47137499999998));
#32061=CARTESIAN_POINT('Ctrl Pts',(-17.4320632938682,-16.6154772628063,
9.42970833333331));
#32062=CARTESIAN_POINT('Ctrl Pts',(-16.4660316469341,-17.1732158942094,
9.38804166666664));
#32063=CARTESIAN_POINT('Ctrl Pts',(-15.4999999999999,-17.7309545256125,
9.34637499999997));
#32064=CARTESIAN_POINT('Ctrl Pts',(-14.5339683530658,-17.1732158942094,
9.30470833333331));
#32065=CARTESIAN_POINT('Ctrl Pts',(-13.5679367061317,-16.6154772628063,
9.26304166666664));
#32066=CARTESIAN_POINT('Ctrl Pts',(-13.5679367061317,-15.5,9.22137499999997));
#32067=CARTESIAN_POINT('Ctrl Pts',(-13.5679367061317,-14.3845227371938,
9.1797083333333));
#32068=CARTESIAN_POINT('Ctrl Pts',(-14.5339683530658,-13.8267841057907,
9.13804166666664));
#32069=CARTESIAN_POINT('Ctrl Pts',(-15.5,-13.2690454743876,9.09637499999997));
#32070=CARTESIAN_POINT('Ctrl Pts',(-16.4660316469341,-13.8267841057907,
9.0547083333333));
#32071=CARTESIAN_POINT('Ctrl Pts',(-17.4320632938682,-14.3845227371938,
9.01304166666664));
#32072=CARTESIAN_POINT('Ctrl Pts',(-17.4320632938682,-15.5000000000001,
8.97137499999997));
#32073=CARTESIAN_POINT('Ctrl Pts',(-17.4320632938682,-16.6154772628063,
8.9297083333333));
#32074=CARTESIAN_POINT('Ctrl Pts',(-16.4660316469341,-17.1732158942094,
8.88804166666663));
#32075=CARTESIAN_POINT('Ctrl Pts',(-15.4999999999999,-17.7309545256125,
8.84637499999997));
#32076=CARTESIAN_POINT('Ctrl Pts',(-14.5339683530658,-17.1732158942094,
8.8047083333333));
#32077=CARTESIAN_POINT('Ctrl Pts',(-13.5679367061317,-16.6154772628063,
8.76304166666663));
#32078=CARTESIAN_POINT('Ctrl Pts',(-13.5679367061317,-15.5,8.72137499999997));
#32079=CARTESIAN_POINT('Ctrl Pts',(-13.5679367061317,-14.3845227371938,
8.6797083333333));
#32080=CARTESIAN_POINT('Ctrl Pts',(-14.5339683530658,-13.8267841057907,
8.63804166666663));
#32081=CARTESIAN_POINT('Ctrl Pts',(-15.5,-13.2690454743876,8.59637499999996));
#32082=CARTESIAN_POINT('Ctrl Pts',(-16.4660316469341,-13.8267841057907,
8.5547083333333));
#32083=CARTESIAN_POINT('Ctrl Pts',(-17.4320632938682,-14.3845227371938,
8.51304166666663));
#32084=CARTESIAN_POINT('Ctrl Pts',(-17.4320632938682,-15.5000000000001,
8.47137499999996));
#32085=CARTESIAN_POINT('Ctrl Pts',(-17.4320632938682,-16.6154772628063,
8.42970833333329));
#32086=CARTESIAN_POINT('Ctrl Pts',(-16.4660316469341,-17.1732158942094,
8.38804166666663));
#32087=CARTESIAN_POINT('Ctrl Pts',(-15.4999999999999,-17.7309545256125,
8.34637499999996));
#32088=CARTESIAN_POINT('Ctrl Pts',(-14.5339683530658,-17.1732158942094,
8.30470833333329));
#32089=CARTESIAN_POINT('Ctrl Pts',(-13.5679367061317,-16.6154772628063,
8.26304166666663));
#32090=CARTESIAN_POINT('Ctrl Pts',(-13.5679367061317,-15.5,8.22137499999996));
#32091=CARTESIAN_POINT('Ctrl Pts',(-13.5679367061317,-14.3845227371938,
8.17970833333329));
#32092=CARTESIAN_POINT('Ctrl Pts',(-14.5339683530658,-13.8267841057907,
8.13804166666662));
#32093=CARTESIAN_POINT('Ctrl Pts',(-15.5,-13.2690454743876,8.09637499999996));
#32094=CARTESIAN_POINT('Ctrl Pts',(-16.4660316469341,-13.8267841057907,
8.05470833333329));
#32095=CARTESIAN_POINT('Ctrl Pts',(-17.4320632938682,-14.3845227371938,
8.01304166666662));
#32096=CARTESIAN_POINT('Ctrl Pts',(-17.4320632938682,-15.5000000000001,
7.97137499999995));
#32097=CARTESIAN_POINT('Ctrl Pts',(-17.4320632938682,-16.6154772628063,
7.92970833333329));
#32098=CARTESIAN_POINT('Ctrl Pts',(-16.4660316469341,-17.1732158942094,
7.88804166666662));
#32099=CARTESIAN_POINT('Ctrl Pts',(-15.4999999999999,-17.7309545256125,
7.84637499999995));
#32100=CARTESIAN_POINT('Ctrl Pts',(-14.5339683530658,-17.1732158942094,
7.80470833333329));
#32101=CARTESIAN_POINT('Ctrl Pts',(-13.5679367061317,-16.6154772628063,
7.76304166666662));
#32102=CARTESIAN_POINT('Ctrl Pts',(-13.5679367061317,-15.5,7.72137499999995));
#32103=CARTESIAN_POINT('Ctrl Pts',(-13.5679367061317,-14.3845227371938,
7.67970833333329));
#32104=CARTESIAN_POINT('Ctrl Pts',(-14.5339683530658,-13.8267841057907,
7.63804166666662));
#32105=CARTESIAN_POINT('Ctrl Pts',(-15.5,-13.2690454743876,7.59637499999995));
#32106=CARTESIAN_POINT('Ctrl Pts',(-16.4660316469341,-13.8267841057907,
7.55470833333328));
#32107=CARTESIAN_POINT('Ctrl Pts',(-17.4320632938682,-14.3845227371938,
7.51304166666662));
#32108=CARTESIAN_POINT('Ctrl Pts',(-17.4320632938682,-15.5000000000001,
7.47137499999995));
#32109=CARTESIAN_POINT('Ctrl Pts',(-17.4320632938682,-16.6154772628063,
7.42970833333328));
#32110=CARTESIAN_POINT('Ctrl Pts',(-16.4660316469341,-17.1732158942094,
7.38804166666661));
#32111=CARTESIAN_POINT('Ctrl Pts',(-15.4999999999999,-17.7309545256125,
7.34637499999995));
#32112=CARTESIAN_POINT('Ctrl Pts',(-14.5339683530658,-17.1732158942094,
7.30470833333328));
#32113=CARTESIAN_POINT('Ctrl Pts',(-13.5679367061317,-16.6154772628063,
7.26304166666661));
#32114=CARTESIAN_POINT('Ctrl Pts',(-13.5679367061317,-15.5,7.22137499999994));
#32115=CARTESIAN_POINT('Ctrl Pts',(-13.5679367061317,-14.3845227371938,
7.17970833333328));
#32116=CARTESIAN_POINT('Ctrl Pts',(-14.5339683530658,-13.8267841057907,
7.13804166666661));
#32117=CARTESIAN_POINT('Ctrl Pts',(-15.5,-13.2690454743876,7.09637499999995));
#32118=CARTESIAN_POINT('Ctrl Pts',(-16.4660316469341,-13.8267841057907,
7.05470833333328));
#32119=CARTESIAN_POINT('Ctrl Pts',(-17.4320632938682,-14.3845227371938,
7.01304166666661));
#32120=CARTESIAN_POINT('Ctrl Pts',(-17.4320632938682,-15.5000000000001,
6.97137499999994));
#32121=CARTESIAN_POINT('Ctrl Pts',(-17.4320632938682,-16.6154772628063,
6.92970833333328));
#32122=CARTESIAN_POINT('Ctrl Pts',(-16.4660316469341,-17.1732158942094,
6.88804166666661));
#32123=CARTESIAN_POINT('Ctrl Pts',(-15.4999999999999,-17.7309545256125,
6.84637499999994));
#32124=CARTESIAN_POINT('Ctrl Pts',(-14.5339683530658,-17.1732158942094,
6.80470833333327));
#32125=CARTESIAN_POINT('Ctrl Pts',(-13.5679367061317,-16.6154772628063,
6.76304166666661));
#32126=CARTESIAN_POINT('Ctrl Pts',(-13.5679367061317,-15.5,6.72137499999994));
#32127=CARTESIAN_POINT('Ctrl Pts',(-13.5679367061317,-14.3845227371938,
6.67970833333327));
#32128=CARTESIAN_POINT('Ctrl Pts',(-14.5339683530658,-13.8267841057907,
6.6380416666666));
#32129=CARTESIAN_POINT('Ctrl Pts',(-15.5,-13.2690454743876,6.59637499999994));
#32130=CARTESIAN_POINT('Ctrl Pts',(-16.4660316469341,-13.8267841057907,
6.55470833333327));
#32131=CARTESIAN_POINT('Ctrl Pts',(-17.4320632938682,-14.3845227371938,
6.5130416666666));
#32132=CARTESIAN_POINT('Ctrl Pts',(-17.4320632938682,-15.5000000000001,
6.47137499999994));
#32133=CARTESIAN_POINT('Ctrl Pts',(-17.4320632938682,-16.6154772628063,
6.42970833333327));
#32134=CARTESIAN_POINT('Ctrl Pts',(-16.4660316469341,-17.1732158942094,
6.3880416666666));
#32135=CARTESIAN_POINT('Ctrl Pts',(-15.4999999999999,-17.7309545256125,
6.34637499999993));
#32136=CARTESIAN_POINT('Ctrl Pts',(-14.5339683530658,-17.1732158942094,
6.30470833333327));
#32137=CARTESIAN_POINT('Ctrl Pts',(-13.5679367061317,-16.6154772628063,
6.2630416666666));
#32138=CARTESIAN_POINT('Ctrl Pts',(-13.5679367061317,-15.5,6.22137499999993));
#32139=CARTESIAN_POINT('Ctrl Pts',(-13.5679367061317,-14.3845227371938,
6.17970833333327));
#32140=CARTESIAN_POINT('Ctrl Pts',(-14.5339683530658,-13.8267841057907,
6.1380416666666));
#32141=CARTESIAN_POINT('Ctrl Pts',(-15.5,-13.2690454743876,6.09637499999993));
#32142=CARTESIAN_POINT('Ctrl Pts',(-16.4660316469341,-13.8267841057907,
6.05470833333326));
#32143=CARTESIAN_POINT('Ctrl Pts',(-17.4320632938682,-14.3845227371938,
6.0130416666666));
#32144=CARTESIAN_POINT('Ctrl Pts',(-17.4320632938682,-15.5000000000001,
5.97137499999993));
#32145=CARTESIAN_POINT('Ctrl Pts',(-17.4320632938682,-16.6154772628063,
5.92970833333326));
#32146=CARTESIAN_POINT('Ctrl Pts',(-16.4660316469341,-17.1732158942094,
5.8880416666666));
#32147=CARTESIAN_POINT('Ctrl Pts',(-15.4999999999999,-17.7309545256125,
5.84637499999993));
#32148=CARTESIAN_POINT('Ctrl Pts',(-14.5339683530658,-17.1732158942094,
5.80470833333326));
#32149=CARTESIAN_POINT('Ctrl Pts',(-13.5679367061317,-16.6154772628063,
5.76304166666659));
#32150=CARTESIAN_POINT('Ctrl Pts',(-13.5679367061317,-15.5,5.72137499999993));
#32151=CARTESIAN_POINT('Ctrl Pts',(-13.5679367061317,-14.3845227371938,
5.67970833333326));
#32152=CARTESIAN_POINT('Ctrl Pts',(-14.5339683530658,-13.8267841057907,
5.63804166666659));
#32153=CARTESIAN_POINT('Ctrl Pts',(-15.5,-13.2690454743876,5.59637499999992));
#32154=CARTESIAN_POINT('Ctrl Pts',(-16.4660316469341,-13.8267841057907,
5.55470833333326));
#32155=CARTESIAN_POINT('Ctrl Pts',(-17.4320632938682,-14.3845227371938,
5.51304166666659));
#32156=CARTESIAN_POINT('Ctrl Pts',(-17.4320632938682,-15.5000000000001,
5.47137499999992));
#32157=CARTESIAN_POINT('Ctrl Pts',(-17.4320632938682,-16.6154772628063,
5.42970833333325));
#32158=CARTESIAN_POINT('Ctrl Pts',(-16.4660316469341,-17.1732158942094,
5.38804166666659));
#32159=CARTESIAN_POINT('Ctrl Pts',(-15.4999999999999,-17.7309545256125,
5.34637499999992));
#32160=CARTESIAN_POINT('Ctrl Pts',(-14.5339683530658,-17.1732158942094,
5.30470833333325));
#32161=CARTESIAN_POINT('Ctrl Pts',(-13.5679367061317,-16.6154772628063,
5.26304166666659));
#32162=CARTESIAN_POINT('Ctrl Pts',(-13.5679367061317,-15.5,5.22137499999992));
#32163=CARTESIAN_POINT('Ctrl Pts',(-13.5679367061317,-14.3845227371938,
5.17970833333325));
#32164=CARTESIAN_POINT('Ctrl Pts',(-14.5339683530658,-13.8267841057907,
5.13804166666659));
#32165=CARTESIAN_POINT('Ctrl Pts',(-15.5,-13.2690454743876,5.09637499999992));
#32166=CARTESIAN_POINT('Ctrl Pts',(-16.4660316469341,-13.8267841057907,
5.05470833333325));
#32167=CARTESIAN_POINT('Ctrl Pts',(-17.4320632938682,-14.3845227371938,
5.01304166666658));
#32168=CARTESIAN_POINT('Ctrl Pts',(-17.4320632938682,-15.5000000000001,
4.97137499999991));
#32169=CARTESIAN_POINT('Ctrl Pts',(-17.4320632938682,-16.6154772628063,
4.92970833333325));
#32170=CARTESIAN_POINT('Ctrl Pts',(-16.4660316469341,-17.1732158942094,
4.88804166666658));
#32171=CARTESIAN_POINT('Ctrl Pts',(-15.4999999999999,-17.7309545256125,
4.84637499999991));
#32172=CARTESIAN_POINT('Ctrl Pts',(-14.5339683530658,-17.1732158942094,
4.80470833333325));
#32173=CARTESIAN_POINT('Ctrl Pts',(-13.5679367061317,-16.6154772628063,
4.76304166666658));
#32174=CARTESIAN_POINT('Ctrl Pts',(-13.5679367061317,-15.5,4.72137499999991));
#32175=CARTESIAN_POINT('Ctrl Pts',(-13.5679367061317,-14.3845227371938,
4.67970833333325));
#32176=CARTESIAN_POINT('Ctrl Pts',(-14.5339683530658,-13.8267841057907,
4.63804166666658));
#32177=CARTESIAN_POINT('Ctrl Pts',(-15.5,-13.2690454743876,4.59637499999991));
#32178=CARTESIAN_POINT('Ctrl Pts',(-16.4660316469341,-13.8267841057907,
4.55470833333324));
#32179=CARTESIAN_POINT('Ctrl Pts',(-17.4320632938682,-14.3845227371938,
4.51304166666658));
#32180=CARTESIAN_POINT('Ctrl Pts',(-17.4320632938682,-15.5000000000001,
4.47137499999991));
#32181=CARTESIAN_POINT('Ctrl Pts',(-17.4320632938682,-16.6154772628063,
4.42970833333324));
#32182=CARTESIAN_POINT('Ctrl Pts',(-16.4660316469341,-17.1732158942094,
4.38804166666657));
#32183=CARTESIAN_POINT('Ctrl Pts',(-15.4999999999999,-17.7309545256125,
4.34637499999991));
#32184=CARTESIAN_POINT('Ctrl Pts',(-14.5339683530658,-17.1732158942094,
4.30470833333324));
#32185=CARTESIAN_POINT('Ctrl Pts',(-13.5679367061317,-16.6154772628063,
4.26304166666657));
#32186=CARTESIAN_POINT('Ctrl Pts',(-13.5679367061317,-15.5,4.22137499999991));
#32187=CARTESIAN_POINT('Ctrl Pts',(-13.5679367061317,-14.3845227371938,
4.17970833333324));
#32188=CARTESIAN_POINT('Ctrl Pts',(-14.5339683530658,-13.8267841057907,
4.13804166666657));
#32189=CARTESIAN_POINT('Ctrl Pts',(-15.5,-13.2690454743876,4.0963749999999));
#32190=CARTESIAN_POINT('Ctrl Pts',(-16.4660316469341,-13.8267841057907,
4.05470833333324));
#32191=CARTESIAN_POINT('Ctrl Pts',(-17.4320632938682,-14.3845227371938,
4.01304166666657));
#32192=CARTESIAN_POINT('Ctrl Pts',(-17.4320632938682,-15.5000000000001,
3.9713749999999));
#32193=CARTESIAN_POINT('Ctrl Pts',(-17.4320632938682,-16.6154772628063,
3.92970833333323));
#32194=CARTESIAN_POINT('Ctrl Pts',(-16.4660316469341,-17.1732158942094,
3.88804166666657));
#32195=CARTESIAN_POINT('Ctrl Pts',(-15.4999999999999,-17.7309545256125,
3.8463749999999));
#32196=CARTESIAN_POINT('Ctrl Pts',(-14.5339683530658,-17.1732158942094,
3.80470833333323));
#32197=CARTESIAN_POINT('Ctrl Pts',(-13.5679367061317,-16.6154772628063,
3.76304166666656));
#32198=CARTESIAN_POINT('Ctrl Pts',(-13.5679367061317,-15.5,3.7213749999999));
#32199=CARTESIAN_POINT('Ctrl Pts',(-13.5679367061317,-14.3845227371938,
3.67970833333323));
#32200=CARTESIAN_POINT('Ctrl Pts',(-14.5339683530658,-13.8267841057907,
3.63804166666656));
#32201=CARTESIAN_POINT('Ctrl Pts',(-15.5,-13.2690454743876,3.5963749999999));
#32202=CARTESIAN_POINT('Ctrl Pts',(-16.4660316469341,-13.8267841057907,
3.55470833333323));
#32203=CARTESIAN_POINT('Ctrl Pts',(-17.4320632938682,-14.3845227371938,
3.51304166666656));
#32204=CARTESIAN_POINT('Ctrl Pts',(-17.4320632938682,-15.5000000000001,
3.4713749999999));
#32205=CARTESIAN_POINT('Ctrl Pts',(-17.4320632938682,-16.6154772628063,
3.42970833333323));
#32206=CARTESIAN_POINT('Ctrl Pts',(-16.4660316469341,-17.1732158942094,
3.38804166666656));
#32207=CARTESIAN_POINT('Ctrl Pts',(-15.4999999999999,-17.7309545256125,
3.34637499999989));
#32208=CARTESIAN_POINT('Ctrl Pts',(-14.5339683530658,-17.1732158942094,
3.30470833333323));
#32209=CARTESIAN_POINT('Ctrl Pts',(-13.5679367061317,-16.6154772628063,
3.26304166666656));
#32210=CARTESIAN_POINT('Ctrl Pts',(-13.5679367061317,-15.5,3.22137499999989));
#32211=CARTESIAN_POINT('Ctrl Pts',(-13.5679367061317,-14.3845227371938,
3.17970833333322));
#32212=CARTESIAN_POINT('Ctrl Pts',(-14.5339683530658,-13.8267841057907,
3.13804166666656));
#32213=CARTESIAN_POINT('Ctrl Pts',(-15.5,-13.2690454743876,3.09637499999989));
#32214=CARTESIAN_POINT('Ctrl Pts',(-16.4660316469341,-13.8267841057907,
3.05470833333322));
#32215=CARTESIAN_POINT('Ctrl Pts',(-17.4320632938682,-14.3845227371938,
3.01304166666656));
#32216=CARTESIAN_POINT('Ctrl Pts',(-17.4320632938682,-15.5000000000001,
2.97137499999989));
#32217=CARTESIAN_POINT('Ctrl Pts',(-17.4320632938682,-16.6154772628063,
2.92970833333322));
#32218=CARTESIAN_POINT('Ctrl Pts',(-16.4660316469341,-17.1732158942094,
2.88804166666655));
#32219=CARTESIAN_POINT('Ctrl Pts',(-15.4999999999999,-17.7309545256125,
2.84637499999989));
#32220=CARTESIAN_POINT('Ctrl Pts',(-14.5339683530658,-17.1732158942094,
2.80470833333322));
#32221=CARTESIAN_POINT('Ctrl Pts',(-13.5679367061317,-16.6154772628063,
2.76304166666655));
#32222=CARTESIAN_POINT('Ctrl Pts',(-13.5679367061317,-15.5,2.72137499999989));
#32223=CARTESIAN_POINT('Ctrl Pts',(-13.5679367061317,-14.3845227371938,
2.67970833333322));
#32224=CARTESIAN_POINT('Ctrl Pts',(-14.5339683530658,-13.8267841057907,
2.63804166666655));
#32225=CARTESIAN_POINT('Ctrl Pts',(-15.5,-13.2690454743876,2.59637499999988));
#32226=CARTESIAN_POINT('Ctrl Pts',(-16.4660316469341,-13.8267841057907,
2.55470833333322));
#32227=CARTESIAN_POINT('Ctrl Pts',(-17.4320632938682,-14.3845227371938,
2.51304166666655));
#32228=CARTESIAN_POINT('Ctrl Pts',(-17.4320632938682,-15.5000000000001,
2.47137499999988));
#32229=CARTESIAN_POINT('Ctrl Pts',(-17.4320632938682,-16.6154772628063,
2.42970833333321));
#32230=CARTESIAN_POINT('Ctrl Pts',(-16.4660316469341,-17.1732158942094,
2.38804166666655));
#32231=CARTESIAN_POINT('Ctrl Pts',(-15.4999999999999,-17.7309545256125,
2.34637499999988));
#32232=CARTESIAN_POINT('Ctrl Pts',(-14.5339683530658,-17.1732158942094,
2.30470833333321));
#32233=CARTESIAN_POINT('Ctrl Pts',(-13.5679367061317,-16.6154772628063,
2.26304166666655));
#32234=CARTESIAN_POINT('Ctrl Pts',(-13.5679367061317,-15.5,2.22137499999988));
#32235=CARTESIAN_POINT('Ctrl Pts',(-13.5679367061317,-14.3845227371938,
2.17970833333321));
#32236=CARTESIAN_POINT('Ctrl Pts',(-14.5339683530658,-13.8267841057907,
2.13804166666654));
#32237=CARTESIAN_POINT('Ctrl Pts',(-15.5,-13.2690454743876,2.09637499999988));
#32238=CARTESIAN_POINT('Ctrl Pts',(-16.4660316469341,-13.8267841057907,
2.05470833333321));
#32239=CARTESIAN_POINT('Ctrl Pts',(-17.4320632938682,-14.3845227371938,
2.01304166666654));
#32240=CARTESIAN_POINT('Ctrl Pts',(-17.4320632938682,-15.5000000000001,
1.97137499999988));
#32241=CARTESIAN_POINT('Ctrl Pts',(-17.4320632938682,-16.6154772628063,
1.92970833333321));
#32242=CARTESIAN_POINT('Ctrl Pts',(-16.4660316469341,-17.1732158942094,
1.88804166666654));
#32243=CARTESIAN_POINT('Ctrl Pts',(-15.4999999999999,-17.7309545256125,
1.84637499999987));
#32244=CARTESIAN_POINT('Ctrl Pts',(-14.5339683530658,-17.1732158942094,
1.80470833333321));
#32245=CARTESIAN_POINT('Ctrl Pts',(-13.5679367061317,-16.6154772628063,
1.76304166666654));
#32246=CARTESIAN_POINT('Ctrl Pts',(-13.5679367061317,-15.5,1.72137499999987));
#32247=CARTESIAN_POINT('Ctrl Pts',(-13.5679367061317,-14.3845227371938,
1.67970833333321));
#32248=CARTESIAN_POINT('Ctrl Pts',(-14.5339683530658,-13.8267841057907,
1.63804166666654));
#32249=CARTESIAN_POINT('Ctrl Pts',(-15.5,-13.2690454743876,1.59637499999987));
#32250=CARTESIAN_POINT('Ctrl Pts',(-16.4660316469341,-13.8267841057907,
1.5547083333332));
#32251=CARTESIAN_POINT('Ctrl Pts',(-17.4320632938682,-14.3845227371938,
1.51304166666654));
#32252=CARTESIAN_POINT('Ctrl Pts',(-17.4320632938682,-15.5000000000001,
1.47137499999987));
#32253=CARTESIAN_POINT('Ctrl Pts',(-17.4320632938682,-16.6154772628063,
1.4297083333332));
#32254=CARTESIAN_POINT('Ctrl Pts',(-16.4660316469341,-17.1732158942094,
1.38804166666653));
#32255=CARTESIAN_POINT('Ctrl Pts',(-15.4999999999999,-17.7309545256125,
1.34637499999987));
#32256=CARTESIAN_POINT('Ctrl Pts',(-14.5339683530658,-17.1732158942094,
1.3047083333332));
#32257=CARTESIAN_POINT('Ctrl Pts',(-13.5679367061317,-16.6154772628063,
1.26304166666653));
#32258=CARTESIAN_POINT('Ctrl Pts',(-13.5679367061317,-15.5,1.22137499999987));
#32259=CARTESIAN_POINT('Ctrl Pts',(-13.5679367061317,-14.3845227371938,
1.1797083333332));
#32260=CARTESIAN_POINT('Ctrl Pts',(-14.5339683530658,-13.8267841057907,
1.13804166666653));
#32261=CARTESIAN_POINT('Ctrl Pts',(-15.5,-13.2690454743876,1.09637499999986));
#32262=CARTESIAN_POINT('Ctrl Pts',(-16.4660316469341,-13.8267841057907,
1.0547083333332));
#32263=CARTESIAN_POINT('Ctrl Pts',(-17.4320632938682,-14.3845227371938,
1.01304166666653));
#32264=CARTESIAN_POINT('Ctrl Pts',(-17.4320632938682,-15.5000000000001,
0.971374999999861));
#32265=CARTESIAN_POINT('Ctrl Pts',(-17.4320632938682,-16.6154772628063,
0.929708333333194));
#32266=CARTESIAN_POINT('Ctrl Pts',(-16.4660316469341,-17.1732158942094,
0.888041666666528));
#32267=CARTESIAN_POINT('Ctrl Pts',(-15.4999999999999,-17.7309545256125,
0.846374999999861));
#32268=CARTESIAN_POINT('Ctrl Pts',(-14.5339683530658,-17.1732158942094,
0.804708333333194));
#32269=CARTESIAN_POINT('Ctrl Pts',(-13.5679367061317,-16.6154772628063,
0.763041666666526));
#32270=CARTESIAN_POINT('Ctrl Pts',(-13.5679367061317,-15.5,0.721374999999859));
#32271=CARTESIAN_POINT('Ctrl Pts',(-13.5679367061317,-14.3845227371938,
0.679708333333192));
#32272=CARTESIAN_POINT('Ctrl Pts',(-14.5339683530658,-13.8267841057907,
0.638041666666525));
#32273=CARTESIAN_POINT('Ctrl Pts',(-15.5,-13.2690454743876,0.596374999999858));
#32274=CARTESIAN_POINT('Ctrl Pts',(-16.4660316469341,-13.8267841057907,
0.55470833333319));
#32275=CARTESIAN_POINT('Ctrl Pts',(-17.4320632938682,-14.3845227371938,
0.513041666666523));
#32276=CARTESIAN_POINT('Ctrl Pts',(-17.4320632938682,-15.5000000000001,
0.471374999999856));
#32277=CARTESIAN_POINT('Ctrl Pts',(-17.4320632938682,-16.6154772628063,
0.429708333333188));
#32278=CARTESIAN_POINT('Ctrl Pts',(-16.4660316469341,-17.1732158942094,
0.388041666666521));
#32279=CARTESIAN_POINT('Ctrl Pts',(-15.4999999999999,-17.7309545256125,
0.346374999999854));
#32280=CARTESIAN_POINT('Ctrl Pts',(-14.5339683530658,-17.1732158942094,
0.304708333333186));
#32281=CARTESIAN_POINT('Ctrl Pts',(-13.5679367061317,-16.6154772628063,
0.263041666666519));
#32282=CARTESIAN_POINT('Ctrl Pts',(-13.5679367061317,-15.5,0.221374999999852));
#32283=CARTESIAN_POINT('Ctrl Pts',(-13.5679367061317,-14.3845227371938,
0.179708333333185));
#32284=CARTESIAN_POINT('Ctrl Pts',(-14.5339683530658,-13.8267841057907,
0.138041666666517));
#32285=CARTESIAN_POINT('Ctrl Pts',(-15.5,-13.2690454743876,0.0963749999998501));
#32286=CARTESIAN_POINT('Ctrl Pts',(-16.4660316469341,-13.8267841057907,
0.0547083333331828));
#32287=CARTESIAN_POINT('Ctrl Pts',(-17.4320632938682,-14.3845227371938,
0.0130416666665155));
#32288=CARTESIAN_POINT('Ctrl Pts',(-17.4320632938682,-15.5000000000001,
-0.0286250000001518));
#32289=CARTESIAN_POINT('Ctrl Pts',(-17.4320632938682,-16.6154772628063,
-0.0702916666668191));
#32290=CARTESIAN_POINT('Ctrl Pts',(-16.4660316469341,-17.1732158942094,
-0.111958333333486));
#32291=CARTESIAN_POINT('Ctrl Pts',(-15.4999999999999,-17.7309545256125,
-0.153625000000154));
#32292=CARTESIAN_POINT('Ctrl Pts',(-14.5339683530658,-17.1732158942094,
-0.195291666666821));
#32293=CARTESIAN_POINT('Ctrl Pts',(-13.5679367061317,-16.6154772628063,
-0.236958333333488));
#32294=CARTESIAN_POINT('Ctrl Pts',(-13.5679367061317,-15.5,-0.278625000000155));
#32295=CARTESIAN_POINT('Ctrl Pts',(-13.5679367061317,-14.3845227371938,
-0.320291666666821));
#32296=CARTESIAN_POINT('Ctrl Pts',(-14.5339683530658,-13.8267841057907,
-0.361958333333488));
#32297=CARTESIAN_POINT('Ctrl Pts',(-15.5,-13.2690454743876,-0.403625000000156));
#32298=CARTESIAN_POINT('Ctrl Pts',(-16.4660316469341,-13.8267841057907,
-0.445291666666823));
#32299=CARTESIAN_POINT('Ctrl Pts',(-17.4320632938682,-14.3845227371938,
-0.48695833333349));
#32300=CARTESIAN_POINT('Ctrl Pts',(-17.4320632938682,-15.5000000000001,
-0.528625000000157));
#32301=CARTESIAN_POINT('Ctrl Pts',(-17.4320632938682,-16.6154772628063,
-0.570291666666825));
#32302=CARTESIAN_POINT('Ctrl Pts',(-16.4660316469341,-17.1732158942094,
-0.611958333333492));
#32303=CARTESIAN_POINT('Ctrl Pts',(-15.4999999999999,-17.7309545256125,
-0.653625000000159));
#32304=CARTESIAN_POINT('Ctrl Pts',(-14.5339683530658,-17.1732158942094,
-0.695291666666827));
#32305=CARTESIAN_POINT('Ctrl Pts',(-13.5679367061317,-16.6154772628063,
-0.736958333333494));
#32306=CARTESIAN_POINT('Ctrl Pts',(-13.5679367061317,-15.5,-0.778625000000161));
#32307=CARTESIAN_POINT('Ctrl Pts',(-13.5679367061317,-14.3845227371938,
-0.820291666666829));
#32308=CARTESIAN_POINT('Ctrl Pts',(-14.5339683530658,-13.8267841057907,
-0.861958333333496));
#32309=CARTESIAN_POINT('Ctrl Pts',(-15.5,-13.2690454743876,-0.903625000000163));
#32310=CARTESIAN_POINT('Ctrl Pts',(-16.4660316469341,-13.8267841057907,
-0.94529166666683));
#32311=CARTESIAN_POINT('Ctrl Pts',(-17.4320632938682,-14.3845227371938,
-0.986958333333498));
#32312=CARTESIAN_POINT('Ctrl Pts',(-17.4320632938682,-15.5000000000001,
-1.02862500000016));
#32313=CARTESIAN_POINT('Ctrl Pts',(-17.4320632938682,-16.6154772628063,
-1.07029166666683));
#32314=CARTESIAN_POINT('Ctrl Pts',(-16.4660316469341,-17.1732158942094,
-1.1119583333335));
#32315=CARTESIAN_POINT('Ctrl Pts',(-15.4999999999999,-17.7309545256125,
-1.15362500000017));
#32316=CARTESIAN_POINT('Ctrl Pts',(-14.5339683530658,-17.1732158942094,
-1.19529166666683));
#32317=CARTESIAN_POINT('Ctrl Pts',(-13.5679367061317,-16.6154772628063,
-1.2369583333335));
#32318=CARTESIAN_POINT('Ctrl Pts',(-13.5679367061317,-15.5,-1.27862500000017));
#32319=CARTESIAN_POINT('Ctrl Pts',(-13.5679367061317,-14.3845227371938,
-1.32029166666684));
#32320=CARTESIAN_POINT('Ctrl Pts',(-14.5339683530658,-13.8267841057907,
-1.3619583333335));
#32321=CARTESIAN_POINT('Ctrl Pts',(-15.5,-13.2690454743876,-1.40362500000017));
#32322=CARTESIAN_POINT('Ctrl Pts',(-16.4660316469341,-13.8267841057907,
-1.44529166666684));
#32323=CARTESIAN_POINT('Ctrl Pts',(-17.4320632938682,-14.3845227371938,
-1.4869583333335));
#32324=CARTESIAN_POINT('Ctrl Pts',(-17.4320632938682,-15.5000000000001,
-1.52862500000017));
#32325=CARTESIAN_POINT('Ctrl Pts',(-17.4320632938682,-16.6154772628063,
-1.57029166666684));
#32326=CARTESIAN_POINT('Ctrl Pts',(-16.4660316469341,-17.1732158942094,
-1.61195833333351));
#32327=CARTESIAN_POINT('Ctrl Pts',(-15.4999999999999,-17.7309545256125,
-1.65362500000017));
#32328=CARTESIAN_POINT('Ctrl Pts',(-14.5339683530658,-17.1732158942094,
-1.69529166666684));
#32329=CARTESIAN_POINT('Ctrl Pts',(-13.5679367061317,-16.6154772628063,
-1.73695833333351));
#32330=CARTESIAN_POINT('Ctrl Pts',(-13.5679367061317,-15.5,-1.77862500000017));
#32331=CARTESIAN_POINT('Ctrl Pts',(-13.5679367061317,-14.3845227371938,
-1.82029166666684));
#32332=CARTESIAN_POINT('Ctrl Pts',(-14.5339683530658,-13.8267841057907,
-1.86195833333351));
#32333=CARTESIAN_POINT('Ctrl Pts',(-15.5,-13.2690454743876,-1.90362500000018));
#32334=CARTESIAN_POINT('Ctrl Pts',(-16.4660316469341,-13.8267841057907,
-1.94529166666684));
#32335=CARTESIAN_POINT('Ctrl Pts',(-17.4320632938682,-14.3845227371938,
-1.98695833333351));
#32336=CARTESIAN_POINT('Ctrl Pts',(-17.4320632938682,-15.5000000000001,
-2.02862500000018));
#32337=CARTESIAN_POINT('Ctrl Pts',(-17.4320632938682,-16.6154772628063,
-2.07029166666685));
#32338=CARTESIAN_POINT('Ctrl Pts',(-16.4660316469341,-17.1732158942094,
-2.11195833333351));
#32339=CARTESIAN_POINT('Ctrl Pts',(-15.4999999999999,-17.7309545256125,
-2.15362500000018));
#32340=CARTESIAN_POINT('Ctrl Pts',(-14.5339683530658,-17.1732158942094,
-2.19529166666685));
#32341=CARTESIAN_POINT('Ctrl Pts',(-14.1783071398503,-16.9678747970191,
-2.21063196867905));
#32342=CARTESIAN_POINT('Ctrl Pts',(-13.9369173167913,-16.6356236599184,
-2.22824840486548));
#32343=CARTESIAN_POINT('',(-14.2215513317126,-16.4288320706154,-2.0251230503213));
#32344=CARTESIAN_POINT('Ctrl Pts',(-13.9406917842496,-15.2436450846258,
10.4122404735808));
#32345=CARTESIAN_POINT('Ctrl Pts',(-14.0620451873461,-14.5054990725558,
10.3753299573543));
#32346=CARTESIAN_POINT('Ctrl Pts',(-14.7098797632095,-14.1314716057907,
10.3411666666667));
#32347=CARTESIAN_POINT('Ctrl Pts',(-15.5,-13.6752954743876,10.2995));
#32348=CARTESIAN_POINT('Ctrl Pts',(-16.2901202367904,-14.1314716057907,
10.2578333333333));
#32349=CARTESIAN_POINT('Ctrl Pts',(-17.0802404735808,-14.5876477371938,
10.2161666666667));
#32350=CARTESIAN_POINT('Ctrl Pts',(-17.0802404735808,-15.5000000000001,
10.1745));
#32351=CARTESIAN_POINT('Ctrl Pts',(-17.0802404735808,-16.4123522628063,
10.1328333333333));
#32352=CARTESIAN_POINT('Ctrl Pts',(-16.2901202367904,-16.8685283942094,
10.0911666666667));
#32353=CARTESIAN_POINT('Ctrl Pts',(-15.4999999999999,-17.3247045256125,
10.0495));
#32354=CARTESIAN_POINT('Ctrl Pts',(-14.7098797632095,-16.8685283942094,
10.0078333333333));
#32355=CARTESIAN_POINT('Ctrl Pts',(-13.9197595264191,-16.4123522628063,
9.96616666666665));
#32356=CARTESIAN_POINT('Ctrl Pts',(-13.9197595264191,-15.5,9.92449999999998));
#32357=CARTESIAN_POINT('Ctrl Pts',(-13.9197595264191,-14.5876477371938,
9.88283333333331));
#32358=CARTESIAN_POINT('Ctrl Pts',(-14.7098797632095,-14.1314716057907,
9.84116666666665));
#32359=CARTESIAN_POINT('Ctrl Pts',(-15.5,-13.6752954743876,9.79949999999998));
#32360=CARTESIAN_POINT('Ctrl Pts',(-16.2901202367904,-14.1314716057907,
9.75783333333331));
#32361=CARTESIAN_POINT('Ctrl Pts',(-17.0802404735808,-14.5876477371938,
9.71616666666665));
#32362=CARTESIAN_POINT('Ctrl Pts',(-17.0802404735808,-15.5000000000001,
9.67449999999998));
#32363=CARTESIAN_POINT('Ctrl Pts',(-17.0802404735808,-16.4123522628063,
9.63283333333331));
#32364=CARTESIAN_POINT('Ctrl Pts',(-16.2901202367904,-16.8685283942094,
9.59116666666664));
#32365=CARTESIAN_POINT('Ctrl Pts',(-15.4999999999999,-17.3247045256125,
9.54949999999998));
#32366=CARTESIAN_POINT('Ctrl Pts',(-14.7098797632095,-16.8685283942094,
9.50783333333331));
#32367=CARTESIAN_POINT('Ctrl Pts',(-13.9197595264191,-16.4123522628063,
9.46616666666664));
#32368=CARTESIAN_POINT('Ctrl Pts',(-13.9197595264191,-15.5,9.42449999999998));
#32369=CARTESIAN_POINT('Ctrl Pts',(-13.9197595264191,-14.5876477371938,
9.38283333333331));
#32370=CARTESIAN_POINT('Ctrl Pts',(-14.7098797632095,-14.1314716057907,
9.34116666666664));
#32371=CARTESIAN_POINT('Ctrl Pts',(-15.5,-13.6752954743876,9.29949999999997));
#32372=CARTESIAN_POINT('Ctrl Pts',(-16.2901202367904,-14.1314716057907,
9.25783333333331));
#32373=CARTESIAN_POINT('Ctrl Pts',(-17.0802404735808,-14.5876477371938,
9.21616666666664));
#32374=CARTESIAN_POINT('Ctrl Pts',(-17.0802404735808,-15.5000000000001,
9.17449999999997));
#32375=CARTESIAN_POINT('Ctrl Pts',(-17.0802404735808,-16.4123522628063,
9.13283333333331));
#32376=CARTESIAN_POINT('Ctrl Pts',(-16.2901202367904,-16.8685283942094,
9.09116666666664));
#32377=CARTESIAN_POINT('Ctrl Pts',(-15.4999999999999,-17.3247045256125,
9.04949999999997));
#32378=CARTESIAN_POINT('Ctrl Pts',(-14.7098797632095,-16.8685283942094,
9.0078333333333));
#32379=CARTESIAN_POINT('Ctrl Pts',(-13.9197595264191,-16.4123522628063,
8.96616666666664));
#32380=CARTESIAN_POINT('Ctrl Pts',(-13.9197595264191,-15.5,8.92449999999997));
#32381=CARTESIAN_POINT('Ctrl Pts',(-13.9197595264191,-14.5876477371938,
8.8828333333333));
#32382=CARTESIAN_POINT('Ctrl Pts',(-14.7098797632095,-14.1314716057907,
8.84116666666664));
#32383=CARTESIAN_POINT('Ctrl Pts',(-15.5,-13.6752954743876,8.79949999999997));
#32384=CARTESIAN_POINT('Ctrl Pts',(-16.2901202367904,-14.1314716057907,
8.7578333333333));
#32385=CARTESIAN_POINT('Ctrl Pts',(-17.0802404735808,-14.5876477371938,
8.71616666666663));
#32386=CARTESIAN_POINT('Ctrl Pts',(-17.0802404735808,-15.5000000000001,
8.67449999999997));
#32387=CARTESIAN_POINT('Ctrl Pts',(-17.0802404735808,-16.4123522628063,
8.6328333333333));
#32388=CARTESIAN_POINT('Ctrl Pts',(-16.2901202367904,-16.8685283942094,
8.59116666666663));
#32389=CARTESIAN_POINT('Ctrl Pts',(-15.4999999999999,-17.3247045256125,
8.54949999999996));
#32390=CARTESIAN_POINT('Ctrl Pts',(-14.7098797632095,-16.8685283942094,
8.50783333333329));
#32391=CARTESIAN_POINT('Ctrl Pts',(-13.9197595264191,-16.4123522628063,
8.46616666666663));
#32392=CARTESIAN_POINT('Ctrl Pts',(-13.9197595264191,-15.5,8.42449999999996));
#32393=CARTESIAN_POINT('Ctrl Pts',(-13.9197595264191,-14.5876477371938,
8.38283333333329));
#32394=CARTESIAN_POINT('Ctrl Pts',(-14.7098797632095,-14.1314716057907,
8.34116666666663));
#32395=CARTESIAN_POINT('Ctrl Pts',(-15.5,-13.6752954743876,8.29949999999996));
#32396=CARTESIAN_POINT('Ctrl Pts',(-16.2901202367904,-14.1314716057907,
8.25783333333329));
#32397=CARTESIAN_POINT('Ctrl Pts',(-17.0802404735808,-14.5876477371938,
8.21616666666663));
#32398=CARTESIAN_POINT('Ctrl Pts',(-17.0802404735808,-15.5000000000001,
8.17449999999996));
#32399=CARTESIAN_POINT('Ctrl Pts',(-17.0802404735808,-16.4123522628063,
8.13283333333329));
#32400=CARTESIAN_POINT('Ctrl Pts',(-16.2901202367904,-16.8685283942094,
8.09116666666663));
#32401=CARTESIAN_POINT('Ctrl Pts',(-15.4999999999999,-17.3247045256125,
8.04949999999996));
#32402=CARTESIAN_POINT('Ctrl Pts',(-14.7098797632095,-16.8685283942094,
8.00783333333329));
#32403=CARTESIAN_POINT('Ctrl Pts',(-13.9197595264191,-16.4123522628063,
7.96616666666662));
#32404=CARTESIAN_POINT('Ctrl Pts',(-13.9197595264191,-15.5,7.92449999999996));
#32405=CARTESIAN_POINT('Ctrl Pts',(-13.9197595264191,-14.5876477371938,
7.88283333333329));
#32406=CARTESIAN_POINT('Ctrl Pts',(-14.7098797632095,-14.1314716057907,
7.84116666666662));
#32407=CARTESIAN_POINT('Ctrl Pts',(-15.5,-13.6752954743876,7.79949999999995));
#32408=CARTESIAN_POINT('Ctrl Pts',(-16.2901202367904,-14.1314716057907,
7.75783333333329));
#32409=CARTESIAN_POINT('Ctrl Pts',(-17.0802404735808,-14.5876477371938,
7.71616666666662));
#32410=CARTESIAN_POINT('Ctrl Pts',(-17.0802404735808,-15.5000000000001,
7.67449999999995));
#32411=CARTESIAN_POINT('Ctrl Pts',(-17.0802404735808,-16.4123522628063,
7.63283333333328));
#32412=CARTESIAN_POINT('Ctrl Pts',(-16.2901202367904,-16.8685283942094,
7.59116666666662));
#32413=CARTESIAN_POINT('Ctrl Pts',(-15.4999999999999,-17.3247045256125,
7.54949999999995));
#32414=CARTESIAN_POINT('Ctrl Pts',(-14.7098797632095,-16.8685283942094,
7.50783333333328));
#32415=CARTESIAN_POINT('Ctrl Pts',(-13.9197595264191,-16.4123522628063,
7.46616666666662));
#32416=CARTESIAN_POINT('Ctrl Pts',(-13.9197595264191,-15.5,7.42449999999995));
#32417=CARTESIAN_POINT('Ctrl Pts',(-13.9197595264191,-14.5876477371938,
7.38283333333328));
#32418=CARTESIAN_POINT('Ctrl Pts',(-14.7098797632095,-14.1314716057907,
7.34116666666661));
#32419=CARTESIAN_POINT('Ctrl Pts',(-15.5,-13.6752954743876,7.29949999999995));
#32420=CARTESIAN_POINT('Ctrl Pts',(-16.2901202367904,-14.1314716057907,
7.25783333333328));
#32421=CARTESIAN_POINT('Ctrl Pts',(-17.0802404735808,-14.5876477371938,
7.21616666666661));
#32422=CARTESIAN_POINT('Ctrl Pts',(-17.0802404735808,-15.5000000000001,
7.17449999999995));
#32423=CARTESIAN_POINT('Ctrl Pts',(-17.0802404735808,-16.4123522628063,
7.13283333333328));
#32424=CARTESIAN_POINT('Ctrl Pts',(-16.2901202367904,-16.8685283942094,
7.09116666666661));
#32425=CARTESIAN_POINT('Ctrl Pts',(-15.4999999999999,-17.3247045256125,
7.04949999999994));
#32426=CARTESIAN_POINT('Ctrl Pts',(-14.7098797632095,-16.8685283942094,
7.00783333333328));
#32427=CARTESIAN_POINT('Ctrl Pts',(-13.9197595264191,-16.4123522628063,
6.96616666666661));
#32428=CARTESIAN_POINT('Ctrl Pts',(-13.9197595264191,-15.5,6.92449999999994));
#32429=CARTESIAN_POINT('Ctrl Pts',(-13.9197595264191,-14.5876477371938,
6.88283333333327));
#32430=CARTESIAN_POINT('Ctrl Pts',(-14.7098797632095,-14.1314716057907,
6.84116666666661));
#32431=CARTESIAN_POINT('Ctrl Pts',(-15.5,-13.6752954743876,6.79949999999994));
#32432=CARTESIAN_POINT('Ctrl Pts',(-16.2901202367904,-14.1314716057907,
6.75783333333327));
#32433=CARTESIAN_POINT('Ctrl Pts',(-17.0802404735808,-14.5876477371938,
6.71616666666661));
#32434=CARTESIAN_POINT('Ctrl Pts',(-17.0802404735808,-15.5000000000001,
6.67449999999994));
#32435=CARTESIAN_POINT('Ctrl Pts',(-17.0802404735808,-16.4123522628063,
6.63283333333327));
#32436=CARTESIAN_POINT('Ctrl Pts',(-16.2901202367904,-16.8685283942094,
6.59116666666661));
#32437=CARTESIAN_POINT('Ctrl Pts',(-15.4999999999999,-17.3247045256125,
6.54949999999994));
#32438=CARTESIAN_POINT('Ctrl Pts',(-14.7098797632095,-16.8685283942094,
6.50783333333327));
#32439=CARTESIAN_POINT('Ctrl Pts',(-13.9197595264191,-16.4123522628063,
6.4661666666666));
#32440=CARTESIAN_POINT('Ctrl Pts',(-13.9197595264191,-15.5,6.42449999999994));
#32441=CARTESIAN_POINT('Ctrl Pts',(-13.9197595264191,-14.5876477371938,
6.38283333333327));
#32442=CARTESIAN_POINT('Ctrl Pts',(-14.7098797632095,-14.1314716057907,
6.3411666666666));
#32443=CARTESIAN_POINT('Ctrl Pts',(-15.5,-13.6752954743876,6.29949999999993));
#32444=CARTESIAN_POINT('Ctrl Pts',(-16.2901202367904,-14.1314716057907,
6.25783333333327));
#32445=CARTESIAN_POINT('Ctrl Pts',(-17.0802404735808,-14.5876477371938,
6.2161666666666));
#32446=CARTESIAN_POINT('Ctrl Pts',(-17.0802404735808,-15.5000000000001,
6.17449999999993));
#32447=CARTESIAN_POINT('Ctrl Pts',(-17.0802404735808,-16.4123522628063,
6.13283333333326));
#32448=CARTESIAN_POINT('Ctrl Pts',(-16.2901202367904,-16.8685283942094,
6.0911666666666));
#32449=CARTESIAN_POINT('Ctrl Pts',(-15.4999999999999,-17.3247045256125,
6.04949999999993));
#32450=CARTESIAN_POINT('Ctrl Pts',(-14.7098797632095,-16.8685283942094,
6.00783333333326));
#32451=CARTESIAN_POINT('Ctrl Pts',(-13.9197595264191,-16.4123522628063,
5.9661666666666));
#32452=CARTESIAN_POINT('Ctrl Pts',(-13.9197595264191,-15.5,5.92449999999993));
#32453=CARTESIAN_POINT('Ctrl Pts',(-13.9197595264191,-14.5876477371938,
5.88283333333326));
#32454=CARTESIAN_POINT('Ctrl Pts',(-14.7098797632095,-14.1314716057907,
5.8411666666666));
#32455=CARTESIAN_POINT('Ctrl Pts',(-15.5,-13.6752954743876,5.79949999999993));
#32456=CARTESIAN_POINT('Ctrl Pts',(-16.2901202367904,-14.1314716057907,
5.75783333333326));
#32457=CARTESIAN_POINT('Ctrl Pts',(-17.0802404735808,-14.5876477371938,
5.71616666666659));
#32458=CARTESIAN_POINT('Ctrl Pts',(-17.0802404735808,-15.5000000000001,
5.67449999999993));
#32459=CARTESIAN_POINT('Ctrl Pts',(-17.0802404735808,-16.4123522628063,
5.63283333333326));
#32460=CARTESIAN_POINT('Ctrl Pts',(-16.2901202367904,-16.8685283942094,
5.59116666666659));
#32461=CARTESIAN_POINT('Ctrl Pts',(-15.4999999999999,-17.3247045256125,
5.54949999999992));
#32462=CARTESIAN_POINT('Ctrl Pts',(-14.7098797632095,-16.8685283942094,
5.50783333333326));
#32463=CARTESIAN_POINT('Ctrl Pts',(-13.9197595264191,-16.4123522628063,
5.46616666666659));
#32464=CARTESIAN_POINT('Ctrl Pts',(-13.9197595264191,-15.5,5.42449999999992));
#32465=CARTESIAN_POINT('Ctrl Pts',(-13.9197595264191,-14.5876477371938,
5.38283333333326));
#32466=CARTESIAN_POINT('Ctrl Pts',(-14.7098797632095,-14.1314716057907,
5.34116666666659));
#32467=CARTESIAN_POINT('Ctrl Pts',(-15.5,-13.6752954743876,5.29949999999992));
#32468=CARTESIAN_POINT('Ctrl Pts',(-16.2901202367904,-14.1314716057907,
5.25783333333325));
#32469=CARTESIAN_POINT('Ctrl Pts',(-17.0802404735808,-14.5876477371938,
5.21616666666659));
#32470=CARTESIAN_POINT('Ctrl Pts',(-17.0802404735808,-15.5000000000001,
5.17449999999992));
#32471=CARTESIAN_POINT('Ctrl Pts',(-17.0802404735808,-16.4123522628063,
5.13283333333325));
#32472=CARTESIAN_POINT('Ctrl Pts',(-16.2901202367904,-16.8685283942094,
5.09116666666658));
#32473=CARTESIAN_POINT('Ctrl Pts',(-15.4999999999999,-17.3247045256125,
5.04949999999992));
#32474=CARTESIAN_POINT('Ctrl Pts',(-14.7098797632095,-16.8685283942094,
5.00783333333325));
#32475=CARTESIAN_POINT('Ctrl Pts',(-13.9197595264191,-16.4123522628063,
4.96616666666658));
#32476=CARTESIAN_POINT('Ctrl Pts',(-13.9197595264191,-15.5,4.92449999999992));
#32477=CARTESIAN_POINT('Ctrl Pts',(-13.9197595264191,-14.5876477371938,
4.88283333333325));
#32478=CARTESIAN_POINT('Ctrl Pts',(-14.7098797632095,-14.1314716057907,
4.84116666666658));
#32479=CARTESIAN_POINT('Ctrl Pts',(-15.5,-13.6752954743876,4.79949999999991));
#32480=CARTESIAN_POINT('Ctrl Pts',(-16.2901202367904,-14.1314716057907,
4.75783333333325));
#32481=CARTESIAN_POINT('Ctrl Pts',(-17.0802404735808,-14.5876477371938,
4.71616666666658));
#32482=CARTESIAN_POINT('Ctrl Pts',(-17.0802404735808,-15.5000000000001,
4.67449999999991));
#32483=CARTESIAN_POINT('Ctrl Pts',(-17.0802404735808,-16.4123522628063,
4.63283333333325));
#32484=CARTESIAN_POINT('Ctrl Pts',(-16.2901202367904,-16.8685283942094,
4.59116666666658));
#32485=CARTESIAN_POINT('Ctrl Pts',(-15.4999999999999,-17.3247045256125,
4.54949999999991));
#32486=CARTESIAN_POINT('Ctrl Pts',(-14.7098797632095,-16.8685283942094,
4.50783333333324));
#32487=CARTESIAN_POINT('Ctrl Pts',(-13.9197595264191,-16.4123522628063,
4.46616666666658));
#32488=CARTESIAN_POINT('Ctrl Pts',(-13.9197595264191,-15.5,4.42449999999991));
#32489=CARTESIAN_POINT('Ctrl Pts',(-13.9197595264191,-14.5876477371938,
4.38283333333324));
#32490=CARTESIAN_POINT('Ctrl Pts',(-14.7098797632095,-14.1314716057907,
4.34116666666657));
#32491=CARTESIAN_POINT('Ctrl Pts',(-15.5,-13.6752954743876,4.29949999999991));
#32492=CARTESIAN_POINT('Ctrl Pts',(-16.2901202367904,-14.1314716057907,
4.25783333333324));
#32493=CARTESIAN_POINT('Ctrl Pts',(-17.0802404735808,-14.5876477371938,
4.21616666666657));
#32494=CARTESIAN_POINT('Ctrl Pts',(-17.0802404735808,-15.5000000000001,
4.17449999999991));
#32495=CARTESIAN_POINT('Ctrl Pts',(-17.0802404735808,-16.4123522628063,
4.13283333333324));
#32496=CARTESIAN_POINT('Ctrl Pts',(-16.2901202367904,-16.8685283942094,
4.09116666666657));
#32497=CARTESIAN_POINT('Ctrl Pts',(-15.4999999999999,-17.3247045256125,
4.0494999999999));
#32498=CARTESIAN_POINT('Ctrl Pts',(-14.7098797632095,-16.8685283942094,
4.00783333333324));
#32499=CARTESIAN_POINT('Ctrl Pts',(-13.9197595264191,-16.4123522628063,
3.96616666666657));
#32500=CARTESIAN_POINT('Ctrl Pts',(-13.9197595264191,-15.5,3.9244999999999));
#32501=CARTESIAN_POINT('Ctrl Pts',(-13.9197595264191,-14.5876477371938,
3.88283333333323));
#32502=CARTESIAN_POINT('Ctrl Pts',(-14.7098797632095,-14.1314716057907,
3.84116666666657));
#32503=CARTESIAN_POINT('Ctrl Pts',(-15.5,-13.6752954743876,3.7994999999999));
#32504=CARTESIAN_POINT('Ctrl Pts',(-16.2901202367904,-14.1314716057907,
3.75783333333323));
#32505=CARTESIAN_POINT('Ctrl Pts',(-17.0802404735808,-14.5876477371938,
3.71616666666657));
#32506=CARTESIAN_POINT('Ctrl Pts',(-17.0802404735808,-15.5000000000001,
3.6744999999999));
#32507=CARTESIAN_POINT('Ctrl Pts',(-17.0802404735808,-16.4123522628063,
3.63283333333323));
#32508=CARTESIAN_POINT('Ctrl Pts',(-16.2901202367904,-16.8685283942094,
3.59116666666656));
#32509=CARTESIAN_POINT('Ctrl Pts',(-15.4999999999999,-17.3247045256125,
3.5494999999999));
#32510=CARTESIAN_POINT('Ctrl Pts',(-14.7098797632095,-16.8685283942094,
3.50783333333323));
#32511=CARTESIAN_POINT('Ctrl Pts',(-13.9197595264191,-16.4123522628063,
3.46616666666656));
#32512=CARTESIAN_POINT('Ctrl Pts',(-13.9197595264191,-15.5,3.4244999999999));
#32513=CARTESIAN_POINT('Ctrl Pts',(-13.9197595264191,-14.5876477371938,
3.38283333333323));
#32514=CARTESIAN_POINT('Ctrl Pts',(-14.7098797632095,-14.1314716057907,
3.34116666666656));
#32515=CARTESIAN_POINT('Ctrl Pts',(-15.5,-13.6752954743876,3.29949999999989));
#32516=CARTESIAN_POINT('Ctrl Pts',(-16.2901202367904,-14.1314716057907,
3.25783333333323));
#32517=CARTESIAN_POINT('Ctrl Pts',(-17.0802404735808,-14.5876477371938,
3.21616666666656));
#32518=CARTESIAN_POINT('Ctrl Pts',(-17.0802404735808,-15.5000000000001,
3.17449999999989));
#32519=CARTESIAN_POINT('Ctrl Pts',(-17.0802404735808,-16.4123522628063,
3.13283333333323));
#32520=CARTESIAN_POINT('Ctrl Pts',(-16.2901202367904,-16.8685283942094,
3.09116666666656));
#32521=CARTESIAN_POINT('Ctrl Pts',(-15.4999999999999,-17.3247045256125,
3.04949999999989));
#32522=CARTESIAN_POINT('Ctrl Pts',(-14.7098797632095,-16.8685283942094,
3.00783333333322));
#32523=CARTESIAN_POINT('Ctrl Pts',(-13.9197595264191,-16.4123522628063,
2.96616666666656));
#32524=CARTESIAN_POINT('Ctrl Pts',(-13.9197595264191,-15.5,2.92449999999989));
#32525=CARTESIAN_POINT('Ctrl Pts',(-13.9197595264191,-14.5876477371938,
2.88283333333322));
#32526=CARTESIAN_POINT('Ctrl Pts',(-14.7098797632095,-14.1314716057907,
2.84116666666655));
#32527=CARTESIAN_POINT('Ctrl Pts',(-15.5,-13.6752954743876,2.79949999999989));
#32528=CARTESIAN_POINT('Ctrl Pts',(-16.2901202367904,-14.1314716057907,
2.75783333333322));
#32529=CARTESIAN_POINT('Ctrl Pts',(-17.0802404735808,-14.5876477371938,
2.71616666666655));
#32530=CARTESIAN_POINT('Ctrl Pts',(-17.0802404735808,-15.5000000000001,
2.67449999999989));
#32531=CARTESIAN_POINT('Ctrl Pts',(-17.0802404735808,-16.4123522628063,
2.63283333333322));
#32532=CARTESIAN_POINT('Ctrl Pts',(-16.2901202367904,-16.8685283942094,
2.59116666666655));
#32533=CARTESIAN_POINT('Ctrl Pts',(-15.4999999999999,-17.3247045256125,
2.54949999999988));
#32534=CARTESIAN_POINT('Ctrl Pts',(-14.7098797632095,-16.8685283942094,
2.50783333333322));
#32535=CARTESIAN_POINT('Ctrl Pts',(-13.9197595264191,-16.4123522628063,
2.46616666666655));
#32536=CARTESIAN_POINT('Ctrl Pts',(-13.9197595264191,-15.5,2.42449999999988));
#32537=CARTESIAN_POINT('Ctrl Pts',(-13.9197595264191,-14.5876477371938,
2.38283333333321));
#32538=CARTESIAN_POINT('Ctrl Pts',(-14.7098797632095,-14.1314716057907,
2.34116666666655));
#32539=CARTESIAN_POINT('Ctrl Pts',(-15.5,-13.6752954743876,2.29949999999988));
#32540=CARTESIAN_POINT('Ctrl Pts',(-16.2901202367904,-14.1314716057907,
2.25783333333321));
#32541=CARTESIAN_POINT('Ctrl Pts',(-17.0802404735808,-14.5876477371938,
2.21616666666655));
#32542=CARTESIAN_POINT('Ctrl Pts',(-17.0802404735808,-15.5000000000001,
2.17449999999988));
#32543=CARTESIAN_POINT('Ctrl Pts',(-17.0802404735808,-16.4123522628063,
2.13283333333321));
#32544=CARTESIAN_POINT('Ctrl Pts',(-16.2901202367904,-16.8685283942094,
2.09116666666655));
#32545=CARTESIAN_POINT('Ctrl Pts',(-15.4999999999999,-17.3247045256125,
2.04949999999988));
#32546=CARTESIAN_POINT('Ctrl Pts',(-14.7098797632095,-16.8685283942094,
2.00783333333321));
#32547=CARTESIAN_POINT('Ctrl Pts',(-13.9197595264191,-16.4123522628063,
1.96616666666654));
#32548=CARTESIAN_POINT('Ctrl Pts',(-13.9197595264191,-15.5,1.92449999999988));
#32549=CARTESIAN_POINT('Ctrl Pts',(-13.9197595264191,-14.5876477371938,
1.88283333333321));
#32550=CARTESIAN_POINT('Ctrl Pts',(-14.7098797632095,-14.1314716057907,
1.84116666666654));
#32551=CARTESIAN_POINT('Ctrl Pts',(-15.5,-13.6752954743876,1.79949999999987));
#32552=CARTESIAN_POINT('Ctrl Pts',(-16.2901202367904,-14.1314716057907,
1.75783333333321));
#32553=CARTESIAN_POINT('Ctrl Pts',(-17.0802404735808,-14.5876477371938,
1.71616666666654));
#32554=CARTESIAN_POINT('Ctrl Pts',(-17.0802404735808,-15.5000000000001,
1.67449999999987));
#32555=CARTESIAN_POINT('Ctrl Pts',(-17.0802404735808,-16.4123522628063,
1.63283333333321));
#32556=CARTESIAN_POINT('Ctrl Pts',(-16.2901202367904,-16.8685283942094,
1.59116666666654));
#32557=CARTESIAN_POINT('Ctrl Pts',(-15.4999999999999,-17.3247045256125,
1.54949999999987));
#32558=CARTESIAN_POINT('Ctrl Pts',(-14.7098797632095,-16.8685283942094,
1.5078333333332));
#32559=CARTESIAN_POINT('Ctrl Pts',(-13.9197595264191,-16.4123522628063,
1.46616666666654));
#32560=CARTESIAN_POINT('Ctrl Pts',(-13.9197595264191,-15.5,1.42449999999987));
#32561=CARTESIAN_POINT('Ctrl Pts',(-13.9197595264191,-14.5876477371938,
1.3828333333332));
#32562=CARTESIAN_POINT('Ctrl Pts',(-14.7098797632095,-14.1314716057907,
1.34116666666653));
#32563=CARTESIAN_POINT('Ctrl Pts',(-15.5,-13.6752954743876,1.29949999999987));
#32564=CARTESIAN_POINT('Ctrl Pts',(-16.2901202367904,-14.1314716057907,
1.2578333333332));
#32565=CARTESIAN_POINT('Ctrl Pts',(-17.0802404735808,-14.5876477371938,
1.21616666666653));
#32566=CARTESIAN_POINT('Ctrl Pts',(-17.0802404735808,-15.5000000000001,
1.17449999999986));
#32567=CARTESIAN_POINT('Ctrl Pts',(-17.0802404735808,-16.4123522628063,
1.1328333333332));
#32568=CARTESIAN_POINT('Ctrl Pts',(-16.2901202367904,-16.8685283942094,
1.09116666666653));
#32569=CARTESIAN_POINT('Ctrl Pts',(-15.4999999999999,-17.3247045256125,
1.04949999999987));
#32570=CARTESIAN_POINT('Ctrl Pts',(-14.7098797632095,-16.8685283942094,
1.0078333333332));
#32571=CARTESIAN_POINT('Ctrl Pts',(-13.9197595264191,-16.4123522628063,
0.96616666666653));
#32572=CARTESIAN_POINT('Ctrl Pts',(-13.9197595264191,-15.5,0.924499999999863));
#32573=CARTESIAN_POINT('Ctrl Pts',(-13.9197595264191,-14.5876477371938,
0.882833333333196));
#32574=CARTESIAN_POINT('Ctrl Pts',(-14.7098797632095,-14.1314716057907,
0.841166666666529));
#32575=CARTESIAN_POINT('Ctrl Pts',(-15.5,-13.6752954743876,0.799499999999861));
#32576=CARTESIAN_POINT('Ctrl Pts',(-16.2901202367904,-14.1314716057907,
0.757833333333194));
#32577=CARTESIAN_POINT('Ctrl Pts',(-17.0802404735808,-14.5876477371938,
0.716166666666527));
#32578=CARTESIAN_POINT('Ctrl Pts',(-17.0802404735808,-15.5000000000001,
0.674499999999859));
#32579=CARTESIAN_POINT('Ctrl Pts',(-17.0802404735808,-16.4123522628063,
0.632833333333192));
#32580=CARTESIAN_POINT('Ctrl Pts',(-16.2901202367904,-16.8685283942094,
0.591166666666525));
#32581=CARTESIAN_POINT('Ctrl Pts',(-15.4999999999999,-17.3247045256125,
0.549499999999857));
#32582=CARTESIAN_POINT('Ctrl Pts',(-14.7098797632095,-16.8685283942094,
0.50783333333319));
#32583=CARTESIAN_POINT('Ctrl Pts',(-13.9197595264191,-16.4123522628063,
0.466166666666523));
#32584=CARTESIAN_POINT('Ctrl Pts',(-13.9197595264191,-15.5,0.424499999999856));
#32585=CARTESIAN_POINT('Ctrl Pts',(-13.9197595264191,-14.5876477371938,
0.382833333333188));
#32586=CARTESIAN_POINT('Ctrl Pts',(-14.7098797632095,-14.1314716057907,
0.341166666666521));
#32587=CARTESIAN_POINT('Ctrl Pts',(-15.5,-13.6752954743876,0.299499999999854));
#32588=CARTESIAN_POINT('Ctrl Pts',(-16.2901202367904,-14.1314716057907,
0.257833333333186));
#32589=CARTESIAN_POINT('Ctrl Pts',(-17.0802404735808,-14.5876477371938,
0.216166666666519));
#32590=CARTESIAN_POINT('Ctrl Pts',(-17.0802404735808,-15.5000000000001,
0.174499999999852));
#32591=CARTESIAN_POINT('Ctrl Pts',(-17.0802404735808,-16.4123522628063,
0.132833333333185));
#32592=CARTESIAN_POINT('Ctrl Pts',(-16.2901202367904,-16.8685283942094,
0.0911666666665173));
#32593=CARTESIAN_POINT('Ctrl Pts',(-15.4999999999999,-17.3247045256125,
0.04949999999985));
#32594=CARTESIAN_POINT('Ctrl Pts',(-14.7098797632095,-16.8685283942094,
0.00783333333318273));
#32595=CARTESIAN_POINT('Ctrl Pts',(-13.9197595264191,-16.4123522628063,
-0.0338333333334846));
#32596=CARTESIAN_POINT('Ctrl Pts',(-13.9197595264191,-15.5,-0.0755000000001518));
#32597=CARTESIAN_POINT('Ctrl Pts',(-13.9197595264191,-14.5876477371938,
-0.117166666666817));
#32598=CARTESIAN_POINT('Ctrl Pts',(-14.7098797632095,-14.1314716057907,
-0.158833333333485));
#32599=CARTESIAN_POINT('Ctrl Pts',(-15.5,-13.6752954743876,-0.200500000000152));
#32600=CARTESIAN_POINT('Ctrl Pts',(-16.2901202367904,-14.1314716057907,
-0.242166666666819));
#32601=CARTESIAN_POINT('Ctrl Pts',(-17.0802404735808,-14.5876477371938,
-0.283833333333487));
#32602=CARTESIAN_POINT('Ctrl Pts',(-17.0802404735808,-15.5000000000001,
-0.325500000000154));
#32603=CARTESIAN_POINT('Ctrl Pts',(-17.0802404735808,-16.4123522628063,
-0.367166666666821));
#32604=CARTESIAN_POINT('Ctrl Pts',(-16.2901202367904,-16.8685283942094,
-0.408833333333488));
#32605=CARTESIAN_POINT('Ctrl Pts',(-15.4999999999999,-17.3247045256125,
-0.450500000000156));
#32606=CARTESIAN_POINT('Ctrl Pts',(-14.7098797632095,-16.8685283942094,
-0.492166666666823));
#32607=CARTESIAN_POINT('Ctrl Pts',(-13.9197595264191,-16.4123522628063,
-0.53383333333349));
#32608=CARTESIAN_POINT('Ctrl Pts',(-13.9197595264191,-15.5,-0.575500000000157));
#32609=CARTESIAN_POINT('Ctrl Pts',(-13.9197595264191,-14.5876477371938,
-0.617166666666825));
#32610=CARTESIAN_POINT('Ctrl Pts',(-14.7098797632095,-14.1314716057907,
-0.658833333333492));
#32611=CARTESIAN_POINT('Ctrl Pts',(-15.5,-13.6752954743876,-0.700500000000159));
#32612=CARTESIAN_POINT('Ctrl Pts',(-16.2901202367904,-14.1314716057907,
-0.742166666666827));
#32613=CARTESIAN_POINT('Ctrl Pts',(-17.0802404735808,-14.5876477371938,
-0.783833333333494));
#32614=CARTESIAN_POINT('Ctrl Pts',(-17.0802404735808,-15.5000000000001,
-0.825500000000161));
#32615=CARTESIAN_POINT('Ctrl Pts',(-17.0802404735808,-16.4123522628063,
-0.867166666666829));
#32616=CARTESIAN_POINT('Ctrl Pts',(-16.2901202367904,-16.8685283942094,
-0.908833333333496));
#32617=CARTESIAN_POINT('Ctrl Pts',(-15.4999999999999,-17.3247045256125,
-0.950500000000163));
#32618=CARTESIAN_POINT('Ctrl Pts',(-14.7098797632095,-16.8685283942094,
-0.99216666666683));
#32619=CARTESIAN_POINT('Ctrl Pts',(-13.9197595264191,-16.4123522628063,
-1.0338333333335));
#32620=CARTESIAN_POINT('Ctrl Pts',(-13.9197595264191,-15.5,-1.07550000000016));
#32621=CARTESIAN_POINT('Ctrl Pts',(-13.9197595264191,-14.5876477371938,
-1.11716666666683));
#32622=CARTESIAN_POINT('Ctrl Pts',(-14.7098797632095,-14.1314716057907,
-1.1588333333335));
#32623=CARTESIAN_POINT('Ctrl Pts',(-15.5,-13.6752954743876,-1.20050000000017));
#32624=CARTESIAN_POINT('Ctrl Pts',(-16.2901202367904,-14.1314716057907,
-1.24216666666683));
#32625=CARTESIAN_POINT('Ctrl Pts',(-17.0802404735808,-14.5876477371938,
-1.2838333333335));
#32626=CARTESIAN_POINT('Ctrl Pts',(-17.0802404735808,-15.5000000000001,
-1.32550000000017));
#32627=CARTESIAN_POINT('Ctrl Pts',(-17.0802404735808,-16.4123522628063,
-1.36716666666683));
#32628=CARTESIAN_POINT('Ctrl Pts',(-16.2901202367904,-16.8685283942094,
-1.4088333333335));
#32629=CARTESIAN_POINT('Ctrl Pts',(-15.4999999999999,-17.3247045256125,
-1.45050000000017));
#32630=CARTESIAN_POINT('Ctrl Pts',(-14.7098797632095,-16.8685283942094,
-1.49216666666684));
#32631=CARTESIAN_POINT('Ctrl Pts',(-13.9197595264191,-16.4123522628063,
-1.5338333333335));
#32632=CARTESIAN_POINT('Ctrl Pts',(-13.9197595264191,-15.5,-1.57550000000017));
#32633=CARTESIAN_POINT('Ctrl Pts',(-13.9197595264191,-14.5876477371938,
-1.61716666666684));
#32634=CARTESIAN_POINT('Ctrl Pts',(-14.7098797632095,-14.1314716057907,
-1.65883333333351));
#32635=CARTESIAN_POINT('Ctrl Pts',(-15.5,-13.6752954743876,-1.70050000000017));
#32636=CARTESIAN_POINT('Ctrl Pts',(-16.2901202367904,-14.1314716057907,
-1.74216666666684));
#32637=CARTESIAN_POINT('Ctrl Pts',(-17.0802404735808,-14.5876477371938,
-1.78383333333351));
#32638=CARTESIAN_POINT('Ctrl Pts',(-17.0802404735808,-15.5000000000001,
-1.82550000000017));
#32639=CARTESIAN_POINT('Ctrl Pts',(-17.0802404735808,-16.4123522628063,
-1.86716666666684));
#32640=CARTESIAN_POINT('Ctrl Pts',(-16.2901202367904,-16.8685283942094,
-1.90883333333351));
#32641=CARTESIAN_POINT('Ctrl Pts',(-15.4999999999999,-17.3247045256125,
-1.95050000000018));
#32642=CARTESIAN_POINT('Ctrl Pts',(-14.7098797632095,-16.8685283942094,
-1.99216666666684));
#32643=CARTESIAN_POINT('Ctrl Pts',(-14.4189900731849,-16.7005831533692,
-2.00750661517932));
#32644=CARTESIAN_POINT('Ctrl Pts',(-14.2215542486879,-16.4288360540162,
-2.02512301646327));
#32645=CARTESIAN_POINT('',(-13.9369173167913,-16.6356236599184,-2.22824840486548));
#32646=CARTESIAN_POINT('Ctrl Pts',(-17.4320632938682,-15.5000000000001,
11.440125));
#32647=CARTESIAN_POINT('Ctrl Pts',(-17.4320632938682,-16.6154772628063,
11.3984583333333));
#32648=CARTESIAN_POINT('Ctrl Pts',(-16.4660316469341,-17.1732158942094,
11.3567916666667));
#32649=CARTESIAN_POINT('Ctrl Pts',(-15.4999999999999,-17.7309545256125,
11.315125));
#32650=CARTESIAN_POINT('Ctrl Pts',(-14.5339683530658,-17.1732158942094,
11.2734583333333));
#32651=CARTESIAN_POINT('Ctrl Pts',(-13.5679367061317,-16.6154772628063,
11.2317916666667));
#32652=CARTESIAN_POINT('Ctrl Pts',(-13.5679367061317,-15.5,11.190125));
#32653=CARTESIAN_POINT('Ctrl Pts',(-13.5679367061317,-14.3845227371938,
11.1484583333333));
#32654=CARTESIAN_POINT('Ctrl Pts',(-14.5339683530658,-13.8267841057907,
11.1067916666667));
#32655=CARTESIAN_POINT('Ctrl Pts',(-15.5,-13.2690454743876,11.065125));
#32656=CARTESIAN_POINT('Ctrl Pts',(-16.4660316469341,-13.8267841057907,
11.0234583333333));
#32657=CARTESIAN_POINT('Ctrl Pts',(-17.4320632938682,-14.3845227371938,
10.9817916666667));
#32658=CARTESIAN_POINT('Ctrl Pts',(-17.4320632938682,-15.5000000000001,
10.940125));
#32659=CARTESIAN_POINT('Ctrl Pts',(-17.4320632938682,-16.6154772628063,
10.8984583333333));
#32660=CARTESIAN_POINT('Ctrl Pts',(-16.4660316469341,-17.1732158942094,
10.8567916666667));
#32661=CARTESIAN_POINT('Ctrl Pts',(-15.4999999999999,-17.7309545256125,
10.815125));
#32662=CARTESIAN_POINT('Ctrl Pts',(-14.5339683530658,-17.1732158942094,
10.7734583333333));
#32663=CARTESIAN_POINT('Ctrl Pts',(-13.5679367061317,-16.6154772628063,
10.7317916666667));
#32664=CARTESIAN_POINT('Ctrl Pts',(-13.5679367061317,-15.5,10.690125));
#32665=CARTESIAN_POINT('Ctrl Pts',(-13.5679367061317,-14.3845227371938,
10.6484583333333));
#32666=CARTESIAN_POINT('Ctrl Pts',(-14.5339683530658,-13.8267841057907,
10.6067916666667));
#32667=CARTESIAN_POINT('Ctrl Pts',(-15.5,-13.2690454743876,10.565125));
#32668=CARTESIAN_POINT('Ctrl Pts',(-16.4660316469341,-13.8267841057907,
10.5234583333333));
#32669=CARTESIAN_POINT('Ctrl Pts',(-17.4320632938682,-14.3845227371938,
10.4817916666667));
#32670=CARTESIAN_POINT('Ctrl Pts',(-17.4320632938682,-15.5000000000001,
10.440125));
#32671=CARTESIAN_POINT('Ctrl Pts',(-17.4320632938682,-16.6154772628063,
10.3984583333333));
#32672=CARTESIAN_POINT('Ctrl Pts',(-16.4660316469341,-17.1732158942094,
10.3567916666667));
#32673=CARTESIAN_POINT('Ctrl Pts',(-15.4999999999999,-17.7309545256125,
10.315125));
#32674=CARTESIAN_POINT('Ctrl Pts',(-14.5339683530658,-17.1732158942094,
10.2734583333333));
#32675=CARTESIAN_POINT('Ctrl Pts',(-13.5679367061317,-16.6154772628063,
10.2317916666667));
#32676=CARTESIAN_POINT('Ctrl Pts',(-13.5679367061317,-15.5,10.190125));
#32677=CARTESIAN_POINT('Ctrl Pts',(-13.5679367061317,-14.3845227371938,
10.1484583333333));
#32678=CARTESIAN_POINT('Ctrl Pts',(-14.5339683530658,-13.8267841057907,
10.1067916666666));
#32679=CARTESIAN_POINT('Ctrl Pts',(-15.5,-13.2690454743876,10.065125));
#32680=CARTESIAN_POINT('Ctrl Pts',(-16.4660316469341,-13.8267841057907,
10.0234583333333));
#32681=CARTESIAN_POINT('Ctrl Pts',(-17.4320632938682,-14.3845227371938,
9.98179166666664));
#32682=CARTESIAN_POINT('Ctrl Pts',(-17.4320632938682,-15.5000000000001,
9.94012499999998));
#32683=CARTESIAN_POINT('Ctrl Pts',(-17.4320632938682,-16.6154772628063,
9.89845833333331));
#32684=CARTESIAN_POINT('Ctrl Pts',(-16.4660316469341,-17.1732158942094,
9.85679166666664));
#32685=CARTESIAN_POINT('Ctrl Pts',(-15.4999999999999,-17.7309545256125,
9.81512499999998));
#32686=CARTESIAN_POINT('Ctrl Pts',(-14.5339683530658,-17.1732158942094,
9.77345833333331));
#32687=CARTESIAN_POINT('Ctrl Pts',(-13.5679367061317,-16.6154772628063,
9.73179166666664));
#32688=CARTESIAN_POINT('Ctrl Pts',(-13.5679367061317,-15.5,9.69012499999998));
#32689=CARTESIAN_POINT('Ctrl Pts',(-13.5679367061317,-14.3845227371938,
9.64845833333331));
#32690=CARTESIAN_POINT('Ctrl Pts',(-14.5339683530658,-13.8267841057907,
9.60679166666664));
#32691=CARTESIAN_POINT('Ctrl Pts',(-15.5,-13.2690454743876,9.56512499999998));
#32692=CARTESIAN_POINT('Ctrl Pts',(-16.4660316469341,-13.8267841057907,
9.52345833333331));
#32693=CARTESIAN_POINT('Ctrl Pts',(-17.4320632938682,-14.3845227371938,
9.48179166666664));
#32694=CARTESIAN_POINT('Ctrl Pts',(-17.4320632938682,-15.5000000000001,
9.44012499999997));
#32695=CARTESIAN_POINT('Ctrl Pts',(-17.4320632938682,-16.6154772628063,
9.39845833333331));
#32696=CARTESIAN_POINT('Ctrl Pts',(-16.4660316469341,-17.1732158942094,
9.35679166666664));
#32697=CARTESIAN_POINT('Ctrl Pts',(-15.4999999999999,-17.7309545256125,
9.31512499999997));
#32698=CARTESIAN_POINT('Ctrl Pts',(-14.5339683530658,-17.1732158942094,
9.2734583333333));
#32699=CARTESIAN_POINT('Ctrl Pts',(-13.5679367061317,-16.6154772628063,
9.23179166666664));
#32700=CARTESIAN_POINT('Ctrl Pts',(-13.5679367061317,-15.5,9.19012499999997));
#32701=CARTESIAN_POINT('Ctrl Pts',(-13.5679367061317,-14.3845227371938,
9.1484583333333));
#32702=CARTESIAN_POINT('Ctrl Pts',(-14.5339683530658,-13.8267841057907,
9.10679166666664));
#32703=CARTESIAN_POINT('Ctrl Pts',(-15.5,-13.2690454743876,9.06512499999997));
#32704=CARTESIAN_POINT('Ctrl Pts',(-16.4660316469341,-13.8267841057907,
9.0234583333333));
#32705=CARTESIAN_POINT('Ctrl Pts',(-17.4320632938682,-14.3845227371938,
8.98179166666663));
#32706=CARTESIAN_POINT('Ctrl Pts',(-17.4320632938682,-15.5000000000001,
8.94012499999997));
#32707=CARTESIAN_POINT('Ctrl Pts',(-17.4320632938682,-16.6154772628063,
8.8984583333333));
#32708=CARTESIAN_POINT('Ctrl Pts',(-16.4660316469341,-17.1732158942094,
8.85679166666663));
#32709=CARTESIAN_POINT('Ctrl Pts',(-15.4999999999999,-17.7309545256125,
8.81512499999996));
#32710=CARTESIAN_POINT('Ctrl Pts',(-14.5339683530658,-17.1732158942094,
8.7734583333333));
#32711=CARTESIAN_POINT('Ctrl Pts',(-13.5679367061317,-16.6154772628063,
8.73179166666663));
#32712=CARTESIAN_POINT('Ctrl Pts',(-13.5679367061317,-15.5,8.69012499999996));
#32713=CARTESIAN_POINT('Ctrl Pts',(-13.5679367061317,-14.3845227371938,
8.64845833333329));
#32714=CARTESIAN_POINT('Ctrl Pts',(-14.5339683530658,-13.8267841057907,
8.60679166666663));
#32715=CARTESIAN_POINT('Ctrl Pts',(-15.5,-13.2690454743876,8.56512499999996));
#32716=CARTESIAN_POINT('Ctrl Pts',(-16.4660316469341,-13.8267841057907,
8.52345833333329));
#32717=CARTESIAN_POINT('Ctrl Pts',(-17.4320632938682,-14.3845227371938,
8.48179166666663));
#32718=CARTESIAN_POINT('Ctrl Pts',(-17.4320632938682,-15.5000000000001,
8.44012499999996));
#32719=CARTESIAN_POINT('Ctrl Pts',(-17.4320632938682,-16.6154772628063,
8.39845833333329));
#32720=CARTESIAN_POINT('Ctrl Pts',(-16.4660316469341,-17.1732158942094,
8.35679166666662));
#32721=CARTESIAN_POINT('Ctrl Pts',(-15.4999999999999,-17.7309545256125,
8.31512499999996));
#32722=CARTESIAN_POINT('Ctrl Pts',(-14.5339683530658,-17.1732158942094,
8.27345833333329));
#32723=CARTESIAN_POINT('Ctrl Pts',(-13.5679367061317,-16.6154772628063,
8.23179166666662));
#32724=CARTESIAN_POINT('Ctrl Pts',(-13.5679367061317,-15.5,8.19012499999996));
#32725=CARTESIAN_POINT('Ctrl Pts',(-13.5679367061317,-14.3845227371938,
8.14845833333329));
#32726=CARTESIAN_POINT('Ctrl Pts',(-14.5339683530658,-13.8267841057907,
8.10679166666662));
#32727=CARTESIAN_POINT('Ctrl Pts',(-15.5,-13.2690454743876,8.06512499999995));
#32728=CARTESIAN_POINT('Ctrl Pts',(-16.4660316469341,-13.8267841057907,
8.02345833333329));
#32729=CARTESIAN_POINT('Ctrl Pts',(-17.4320632938682,-14.3845227371938,
7.98179166666662));
#32730=CARTESIAN_POINT('Ctrl Pts',(-17.4320632938682,-15.5000000000001,
7.94012499999995));
#32731=CARTESIAN_POINT('Ctrl Pts',(-17.4320632938682,-16.6154772628063,
7.89845833333329));
#32732=CARTESIAN_POINT('Ctrl Pts',(-16.4660316469341,-17.1732158942094,
7.85679166666662));
#32733=CARTESIAN_POINT('Ctrl Pts',(-15.4999999999999,-17.7309545256125,
7.81512499999995));
#32734=CARTESIAN_POINT('Ctrl Pts',(-14.5339683530658,-17.1732158942094,
7.77345833333328));
#32735=CARTESIAN_POINT('Ctrl Pts',(-13.5679367061317,-16.6154772628063,
7.73179166666662));
#32736=CARTESIAN_POINT('Ctrl Pts',(-13.5679367061317,-15.5,7.69012499999995));
#32737=CARTESIAN_POINT('Ctrl Pts',(-13.5679367061317,-14.3845227371938,
7.64845833333328));
#32738=CARTESIAN_POINT('Ctrl Pts',(-14.5339683530658,-13.8267841057907,
7.60679166666661));
#32739=CARTESIAN_POINT('Ctrl Pts',(-15.5,-13.2690454743876,7.56512499999995));
#32740=CARTESIAN_POINT('Ctrl Pts',(-16.4660316469341,-13.8267841057907,
7.52345833333328));
#32741=CARTESIAN_POINT('Ctrl Pts',(-17.4320632938682,-14.3845227371938,
7.48179166666661));
#32742=CARTESIAN_POINT('Ctrl Pts',(-17.4320632938682,-15.5000000000001,
7.44012499999995));
#32743=CARTESIAN_POINT('Ctrl Pts',(-17.4320632938682,-16.6154772628063,
7.39845833333328));
#32744=CARTESIAN_POINT('Ctrl Pts',(-16.4660316469341,-17.1732158942094,
7.35679166666661));
#32745=CARTESIAN_POINT('Ctrl Pts',(-15.4999999999999,-17.7309545256125,
7.31512499999995));
#32746=CARTESIAN_POINT('Ctrl Pts',(-14.5339683530658,-17.1732158942094,
7.27345833333328));
#32747=CARTESIAN_POINT('Ctrl Pts',(-13.5679367061317,-16.6154772628063,
7.23179166666661));
#32748=CARTESIAN_POINT('Ctrl Pts',(-13.5679367061317,-15.5,7.19012499999994));
#32749=CARTESIAN_POINT('Ctrl Pts',(-13.5679367061317,-14.3845227371938,
7.14845833333328));
#32750=CARTESIAN_POINT('Ctrl Pts',(-14.5339683530658,-13.8267841057907,
7.10679166666661));
#32751=CARTESIAN_POINT('Ctrl Pts',(-15.5,-13.2690454743876,7.06512499999994));
#32752=CARTESIAN_POINT('Ctrl Pts',(-16.4660316469341,-13.8267841057907,
7.02345833333327));
#32753=CARTESIAN_POINT('Ctrl Pts',(-17.4320632938682,-14.3845227371938,
6.98179166666661));
#32754=CARTESIAN_POINT('Ctrl Pts',(-17.4320632938682,-15.5000000000001,
6.94012499999994));
#32755=CARTESIAN_POINT('Ctrl Pts',(-17.4320632938682,-16.6154772628063,
6.89845833333327));
#32756=CARTESIAN_POINT('Ctrl Pts',(-16.4660316469341,-17.1732158942094,
6.8567916666666));
#32757=CARTESIAN_POINT('Ctrl Pts',(-15.4999999999999,-17.7309545256125,
6.81512499999994));
#32758=CARTESIAN_POINT('Ctrl Pts',(-14.5339683530658,-17.1732158942094,
6.77345833333327));
#32759=CARTESIAN_POINT('Ctrl Pts',(-13.5679367061317,-16.6154772628063,
6.7317916666666));
#32760=CARTESIAN_POINT('Ctrl Pts',(-13.5679367061317,-15.5,6.69012499999994));
#32761=CARTESIAN_POINT('Ctrl Pts',(-13.5679367061317,-14.3845227371938,
6.64845833333327));
#32762=CARTESIAN_POINT('Ctrl Pts',(-14.5339683530658,-13.8267841057907,
6.6067916666666));
#32763=CARTESIAN_POINT('Ctrl Pts',(-15.5,-13.2690454743876,6.56512499999993));
#32764=CARTESIAN_POINT('Ctrl Pts',(-16.4660316469341,-13.8267841057907,
6.52345833333327));
#32765=CARTESIAN_POINT('Ctrl Pts',(-17.4320632938682,-14.3845227371938,
6.4817916666666));
#32766=CARTESIAN_POINT('Ctrl Pts',(-17.4320632938682,-15.5000000000001,
6.44012499999993));
#32767=CARTESIAN_POINT('Ctrl Pts',(-17.4320632938682,-16.6154772628063,
6.39845833333327));
#32768=CARTESIAN_POINT('Ctrl Pts',(-16.4660316469341,-17.1732158942094,
6.3567916666666));
#32769=CARTESIAN_POINT('Ctrl Pts',(-15.4999999999999,-17.7309545256125,
6.31512499999993));
#32770=CARTESIAN_POINT('Ctrl Pts',(-14.5339683530658,-17.1732158942094,
6.27345833333326));
#32771=CARTESIAN_POINT('Ctrl Pts',(-13.5679367061317,-16.6154772628063,
6.2317916666666));
#32772=CARTESIAN_POINT('Ctrl Pts',(-13.5679367061317,-15.5,6.19012499999993));
#32773=CARTESIAN_POINT('Ctrl Pts',(-13.5679367061317,-14.3845227371938,
6.14845833333326));
#32774=CARTESIAN_POINT('Ctrl Pts',(-14.5339683530658,-13.8267841057907,
6.10679166666659));
#32775=CARTESIAN_POINT('Ctrl Pts',(-15.5,-13.2690454743876,6.06512499999993));
#32776=CARTESIAN_POINT('Ctrl Pts',(-16.4660316469341,-13.8267841057907,
6.02345833333326));
#32777=CARTESIAN_POINT('Ctrl Pts',(-17.4320632938682,-14.3845227371938,
5.98179166666659));
#32778=CARTESIAN_POINT('Ctrl Pts',(-17.4320632938682,-15.5000000000001,
5.94012499999993));
#32779=CARTESIAN_POINT('Ctrl Pts',(-17.4320632938682,-16.6154772628063,
5.89845833333326));
#32780=CARTESIAN_POINT('Ctrl Pts',(-16.4660316469341,-17.1732158942094,
5.85679166666659));
#32781=CARTESIAN_POINT('Ctrl Pts',(-15.4999999999999,-17.7309545256125,
5.81512499999992));
#32782=CARTESIAN_POINT('Ctrl Pts',(-14.5339683530658,-17.1732158942094,
5.77345833333326));
#32783=CARTESIAN_POINT('Ctrl Pts',(-13.5679367061317,-16.6154772628063,
5.73179166666659));
#32784=CARTESIAN_POINT('Ctrl Pts',(-13.5679367061317,-15.5,5.69012499999992));
#32785=CARTESIAN_POINT('Ctrl Pts',(-13.5679367061317,-14.3845227371938,
5.64845833333326));
#32786=CARTESIAN_POINT('Ctrl Pts',(-14.5339683530658,-13.8267841057907,
5.60679166666659));
#32787=CARTESIAN_POINT('Ctrl Pts',(-15.5,-13.2690454743876,5.56512499999992));
#32788=CARTESIAN_POINT('Ctrl Pts',(-16.4660316469341,-13.8267841057907,
5.52345833333325));
#32789=CARTESIAN_POINT('Ctrl Pts',(-17.4320632938682,-14.3845227371938,
5.48179166666659));
#32790=CARTESIAN_POINT('Ctrl Pts',(-17.4320632938682,-15.5000000000001,
5.44012499999992));
#32791=CARTESIAN_POINT('Ctrl Pts',(-17.4320632938682,-16.6154772628063,
5.39845833333325));
#32792=CARTESIAN_POINT('Ctrl Pts',(-16.4660316469341,-17.1732158942094,
5.35679166666658));
#32793=CARTESIAN_POINT('Ctrl Pts',(-15.4999999999999,-17.7309545256125,
5.31512499999992));
#32794=CARTESIAN_POINT('Ctrl Pts',(-14.5339683530658,-17.1732158942094,
5.27345833333325));
#32795=CARTESIAN_POINT('Ctrl Pts',(-13.5679367061317,-16.6154772628063,
5.23179166666658));
#32796=CARTESIAN_POINT('Ctrl Pts',(-13.5679367061317,-15.5,5.19012499999992));
#32797=CARTESIAN_POINT('Ctrl Pts',(-13.5679367061317,-14.3845227371938,
5.14845833333325));
#32798=CARTESIAN_POINT('Ctrl Pts',(-14.5339683530658,-13.8267841057907,
5.10679166666658));
#32799=CARTESIAN_POINT('Ctrl Pts',(-15.5,-13.2690454743876,5.06512499999991));
#32800=CARTESIAN_POINT('Ctrl Pts',(-16.4660316469341,-13.8267841057907,
5.02345833333325));
#32801=CARTESIAN_POINT('Ctrl Pts',(-17.4320632938682,-14.3845227371938,
4.98179166666658));
#32802=CARTESIAN_POINT('Ctrl Pts',(-17.4320632938682,-15.5000000000001,
4.94012499999991));
#32803=CARTESIAN_POINT('Ctrl Pts',(-17.4320632938682,-16.6154772628063,
4.89845833333325));
#32804=CARTESIAN_POINT('Ctrl Pts',(-16.4660316469341,-17.1732158942094,
4.85679166666658));
#32805=CARTESIAN_POINT('Ctrl Pts',(-15.4999999999999,-17.7309545256125,
4.81512499999991));
#32806=CARTESIAN_POINT('Ctrl Pts',(-14.5339683530658,-17.1732158942094,
4.77345833333324));
#32807=CARTESIAN_POINT('Ctrl Pts',(-13.5679367061317,-16.6154772628063,
4.73179166666658));
#32808=CARTESIAN_POINT('Ctrl Pts',(-13.5679367061317,-15.5,4.69012499999991));
#32809=CARTESIAN_POINT('Ctrl Pts',(-13.5679367061317,-14.3845227371938,
4.64845833333324));
#32810=CARTESIAN_POINT('Ctrl Pts',(-14.5339683530658,-13.8267841057907,
4.60679166666657));
#32811=CARTESIAN_POINT('Ctrl Pts',(-15.5,-13.2690454743876,4.56512499999991));
#32812=CARTESIAN_POINT('Ctrl Pts',(-16.4660316469341,-13.8267841057907,
4.52345833333324));
#32813=CARTESIAN_POINT('Ctrl Pts',(-17.4320632938682,-14.3845227371938,
4.48179166666657));
#32814=CARTESIAN_POINT('Ctrl Pts',(-17.4320632938682,-15.5000000000001,
4.44012499999991));
#32815=CARTESIAN_POINT('Ctrl Pts',(-17.4320632938682,-16.6154772628063,
4.39845833333324));
#32816=CARTESIAN_POINT('Ctrl Pts',(-16.4660316469341,-17.1732158942094,
4.35679166666657));
#32817=CARTESIAN_POINT('Ctrl Pts',(-15.4999999999999,-17.7309545256125,
4.31512499999991));
#32818=CARTESIAN_POINT('Ctrl Pts',(-14.5339683530658,-17.1732158942094,
4.27345833333324));
#32819=CARTESIAN_POINT('Ctrl Pts',(-13.5679367061317,-16.6154772628063,
4.23179166666657));
#32820=CARTESIAN_POINT('Ctrl Pts',(-13.5679367061317,-15.5,4.1901249999999));
#32821=CARTESIAN_POINT('Ctrl Pts',(-13.5679367061317,-14.3845227371938,
4.14845833333324));
#32822=CARTESIAN_POINT('Ctrl Pts',(-14.5339683530658,-13.8267841057907,
4.10679166666657));
#32823=CARTESIAN_POINT('Ctrl Pts',(-15.5,-13.2690454743876,4.0651249999999));
#32824=CARTESIAN_POINT('Ctrl Pts',(-16.4660316469341,-13.8267841057907,
4.02345833333323));
#32825=CARTESIAN_POINT('Ctrl Pts',(-17.4320632938682,-14.3845227371938,
3.98179166666657));
#32826=CARTESIAN_POINT('Ctrl Pts',(-17.4320632938682,-15.5000000000001,
3.9401249999999));
#32827=CARTESIAN_POINT('Ctrl Pts',(-17.4320632938682,-16.6154772628063,
3.89845833333323));
#32828=CARTESIAN_POINT('Ctrl Pts',(-16.4660316469341,-17.1732158942094,
3.85679166666657));
#32829=CARTESIAN_POINT('Ctrl Pts',(-15.4999999999999,-17.7309545256125,
3.8151249999999));
#32830=CARTESIAN_POINT('Ctrl Pts',(-14.5339683530658,-17.1732158942094,
3.77345833333323));
#32831=CARTESIAN_POINT('Ctrl Pts',(-13.5679367061317,-16.6154772628063,
3.73179166666656));
#32832=CARTESIAN_POINT('Ctrl Pts',(-13.5679367061317,-15.5,3.6901249999999));
#32833=CARTESIAN_POINT('Ctrl Pts',(-13.5679367061317,-14.3845227371938,
3.64845833333323));
#32834=CARTESIAN_POINT('Ctrl Pts',(-14.5339683530658,-13.8267841057907,
3.60679166666656));
#32835=CARTESIAN_POINT('Ctrl Pts',(-15.5,-13.2690454743876,3.5651249999999));
#32836=CARTESIAN_POINT('Ctrl Pts',(-16.4660316469341,-13.8267841057907,
3.52345833333323));
#32837=CARTESIAN_POINT('Ctrl Pts',(-17.4320632938682,-14.3845227371938,
3.48179166666656));
#32838=CARTESIAN_POINT('Ctrl Pts',(-17.4320632938682,-15.5000000000001,
3.44012499999989));
#32839=CARTESIAN_POINT('Ctrl Pts',(-17.4320632938682,-16.6154772628063,
3.39845833333323));
#32840=CARTESIAN_POINT('Ctrl Pts',(-16.4660316469341,-17.1732158942094,
3.35679166666656));
#32841=CARTESIAN_POINT('Ctrl Pts',(-15.4999999999999,-17.7309545256125,
3.31512499999989));
#32842=CARTESIAN_POINT('Ctrl Pts',(-14.5339683530658,-17.1732158942094,
3.27345833333322));
#32843=CARTESIAN_POINT('Ctrl Pts',(-13.5679367061317,-16.6154772628063,
3.23179166666656));
#32844=CARTESIAN_POINT('Ctrl Pts',(-13.5679367061317,-15.5,3.19012499999989));
#32845=CARTESIAN_POINT('Ctrl Pts',(-13.5679367061317,-14.3845227371938,
3.14845833333322));
#32846=CARTESIAN_POINT('Ctrl Pts',(-14.5339683530658,-13.8267841057907,
3.10679166666655));
#32847=CARTESIAN_POINT('Ctrl Pts',(-15.5,-13.2690454743876,3.06512499999989));
#32848=CARTESIAN_POINT('Ctrl Pts',(-16.4660316469341,-13.8267841057907,
3.02345833333322));
#32849=CARTESIAN_POINT('Ctrl Pts',(-17.4320632938682,-14.3845227371938,
2.98179166666655));
#32850=CARTESIAN_POINT('Ctrl Pts',(-17.4320632938682,-15.5000000000001,
2.94012499999989));
#32851=CARTESIAN_POINT('Ctrl Pts',(-17.4320632938682,-16.6154772628063,
2.89845833333322));
#32852=CARTESIAN_POINT('Ctrl Pts',(-16.4660316469341,-17.1732158942094,
2.85679166666655));
#32853=CARTESIAN_POINT('Ctrl Pts',(-15.4999999999999,-17.7309545256125,
2.81512499999988));
#32854=CARTESIAN_POINT('Ctrl Pts',(-14.5339683530658,-17.1732158942094,
2.77345833333322));
#32855=CARTESIAN_POINT('Ctrl Pts',(-13.5679367061317,-16.6154772628063,
2.73179166666655));
#32856=CARTESIAN_POINT('Ctrl Pts',(-13.5679367061317,-15.5,2.69012499999988));
#32857=CARTESIAN_POINT('Ctrl Pts',(-13.5679367061317,-14.3845227371938,
2.64845833333321));
#32858=CARTESIAN_POINT('Ctrl Pts',(-14.5339683530658,-13.8267841057907,
2.60679166666655));
#32859=CARTESIAN_POINT('Ctrl Pts',(-15.5,-13.2690454743876,2.56512499999988));
#32860=CARTESIAN_POINT('Ctrl Pts',(-16.4660316469341,-13.8267841057907,
2.52345833333321));
#32861=CARTESIAN_POINT('Ctrl Pts',(-17.4320632938682,-14.3845227371938,
2.48179166666655));
#32862=CARTESIAN_POINT('Ctrl Pts',(-17.4320632938682,-15.5000000000001,
2.44012499999988));
#32863=CARTESIAN_POINT('Ctrl Pts',(-17.4320632938682,-16.6154772628063,
2.39845833333321));
#32864=CARTESIAN_POINT('Ctrl Pts',(-16.4660316469341,-17.1732158942094,
2.35679166666655));
#32865=CARTESIAN_POINT('Ctrl Pts',(-15.4999999999999,-17.7309545256125,
2.31512499999988));
#32866=CARTESIAN_POINT('Ctrl Pts',(-14.5339683530658,-17.1732158942094,
2.27345833333321));
#32867=CARTESIAN_POINT('Ctrl Pts',(-13.5679367061317,-16.6154772628063,
2.23179166666654));
#32868=CARTESIAN_POINT('Ctrl Pts',(-13.5679367061317,-15.5,2.19012499999988));
#32869=CARTESIAN_POINT('Ctrl Pts',(-13.5679367061317,-14.3845227371938,
2.14845833333321));
#32870=CARTESIAN_POINT('Ctrl Pts',(-14.5339683530658,-13.8267841057907,
2.10679166666654));
#32871=CARTESIAN_POINT('Ctrl Pts',(-15.5,-13.2690454743876,2.06512499999987));
#32872=CARTESIAN_POINT('Ctrl Pts',(-16.4660316469341,-13.8267841057907,
2.02345833333321));
#32873=CARTESIAN_POINT('Ctrl Pts',(-17.4320632938682,-14.3845227371938,
1.98179166666654));
#32874=CARTESIAN_POINT('Ctrl Pts',(-17.4320632938682,-15.5000000000001,
1.94012499999987));
#32875=CARTESIAN_POINT('Ctrl Pts',(-17.4320632938682,-16.6154772628063,
1.89845833333321));
#32876=CARTESIAN_POINT('Ctrl Pts',(-16.4660316469341,-17.1732158942094,
1.85679166666654));
#32877=CARTESIAN_POINT('Ctrl Pts',(-15.4999999999999,-17.7309545256125,
1.81512499999987));
#32878=CARTESIAN_POINT('Ctrl Pts',(-14.5339683530658,-17.1732158942094,
1.7734583333332));
#32879=CARTESIAN_POINT('Ctrl Pts',(-13.5679367061317,-16.6154772628063,
1.73179166666654));
#32880=CARTESIAN_POINT('Ctrl Pts',(-13.5679367061317,-15.5,1.69012499999987));
#32881=CARTESIAN_POINT('Ctrl Pts',(-13.5679367061317,-14.3845227371938,
1.6484583333332));
#32882=CARTESIAN_POINT('Ctrl Pts',(-14.5339683530658,-13.8267841057907,
1.60679166666653));
#32883=CARTESIAN_POINT('Ctrl Pts',(-15.5,-13.2690454743876,1.56512499999987));
#32884=CARTESIAN_POINT('Ctrl Pts',(-16.4660316469341,-13.8267841057907,
1.5234583333332));
#32885=CARTESIAN_POINT('Ctrl Pts',(-17.4320632938682,-14.3845227371938,
1.48179166666653));
#32886=CARTESIAN_POINT('Ctrl Pts',(-17.4320632938682,-15.5000000000001,
1.44012499999987));
#32887=CARTESIAN_POINT('Ctrl Pts',(-17.4320632938682,-16.6154772628063,
1.3984583333332));
#32888=CARTESIAN_POINT('Ctrl Pts',(-16.4660316469341,-17.1732158942094,
1.35679166666653));
#32889=CARTESIAN_POINT('Ctrl Pts',(-15.4999999999999,-17.7309545256125,
1.31512499999987));
#32890=CARTESIAN_POINT('Ctrl Pts',(-14.5339683530658,-17.1732158942094,
1.2734583333332));
#32891=CARTESIAN_POINT('Ctrl Pts',(-13.5679367061317,-16.6154772628063,
1.23179166666653));
#32892=CARTESIAN_POINT('Ctrl Pts',(-13.5679367061317,-15.5,1.19012499999986));
#32893=CARTESIAN_POINT('Ctrl Pts',(-13.5679367061317,-14.3845227371938,
1.1484583333332));
#32894=CARTESIAN_POINT('Ctrl Pts',(-14.5339683530658,-13.8267841057907,
1.10679166666653));
#32895=CARTESIAN_POINT('Ctrl Pts',(-15.5,-13.2690454743876,1.06512499999986));
#32896=CARTESIAN_POINT('Ctrl Pts',(-16.4660316469341,-13.8267841057907,
1.02345833333319));
#32897=CARTESIAN_POINT('Ctrl Pts',(-17.4320632938682,-14.3845227371938,
0.981791666666527));
#32898=CARTESIAN_POINT('Ctrl Pts',(-17.4320632938682,-15.5000000000001,
0.94012499999986));
#32899=CARTESIAN_POINT('Ctrl Pts',(-17.4320632938682,-16.6154772628063,
0.898458333333192));
#32900=CARTESIAN_POINT('Ctrl Pts',(-16.4660316469341,-17.1732158942094,
0.856791666666525));
#32901=CARTESIAN_POINT('Ctrl Pts',(-15.4999999999999,-17.7309545256125,
0.815124999999858));
#32902=CARTESIAN_POINT('Ctrl Pts',(-14.5339683530658,-17.1732158942094,
0.77345833333319));
#32903=CARTESIAN_POINT('Ctrl Pts',(-13.5679367061317,-16.6154772628063,
0.731791666666523));
#32904=CARTESIAN_POINT('Ctrl Pts',(-13.5679367061317,-15.5,0.690124999999856));
#32905=CARTESIAN_POINT('Ctrl Pts',(-13.5679367061317,-14.3845227371938,
0.648458333333188));
#32906=CARTESIAN_POINT('Ctrl Pts',(-14.5339683530658,-13.8267841057907,
0.606791666666521));
#32907=CARTESIAN_POINT('Ctrl Pts',(-15.5,-13.2690454743876,0.565124999999854));
#32908=CARTESIAN_POINT('Ctrl Pts',(-16.4660316469341,-13.8267841057907,
0.523458333333187));
#32909=CARTESIAN_POINT('Ctrl Pts',(-17.4320632938682,-14.3845227371938,
0.481791666666519));
#32910=CARTESIAN_POINT('Ctrl Pts',(-17.4320632938682,-15.5000000000001,
0.440124999999852));
#32911=CARTESIAN_POINT('Ctrl Pts',(-17.4320632938682,-16.6154772628063,
0.398458333333185));
#32912=CARTESIAN_POINT('Ctrl Pts',(-16.4660316469341,-17.1732158942094,
0.356791666666518));
#32913=CARTESIAN_POINT('Ctrl Pts',(-15.4999999999999,-17.7309545256125,
0.31512499999985));
#32914=CARTESIAN_POINT('Ctrl Pts',(-14.5339683530658,-17.1732158942094,
0.273458333333183));
#32915=CARTESIAN_POINT('Ctrl Pts',(-13.5679367061317,-16.6154772628063,
0.231791666666516));
#32916=CARTESIAN_POINT('Ctrl Pts',(-13.5679367061317,-15.5,0.190124999999848));
#32917=CARTESIAN_POINT('Ctrl Pts',(-13.5679367061317,-14.3845227371938,
0.148458333333183));
#32918=CARTESIAN_POINT('Ctrl Pts',(-14.5339683530658,-13.8267841057907,
0.106791666666516));
#32919=CARTESIAN_POINT('Ctrl Pts',(-15.5,-13.2690454743876,0.0651249999998483));
#32920=CARTESIAN_POINT('Ctrl Pts',(-16.4660316469341,-13.8267841057907,
0.023458333333181));
#32921=CARTESIAN_POINT('Ctrl Pts',(-17.4320632938682,-14.3845227371938,
-0.0182083333334863));
#32922=CARTESIAN_POINT('Ctrl Pts',(-17.4320632938682,-15.5000000000001,
-0.0598750000001536));
#32923=CARTESIAN_POINT('Ctrl Pts',(-17.4320632938682,-16.6154772628063,
-0.101541666666821));
#32924=CARTESIAN_POINT('Ctrl Pts',(-16.4660316469341,-17.1732158942094,
-0.143208333333488));
#32925=CARTESIAN_POINT('Ctrl Pts',(-15.4999999999999,-17.7309545256125,
-0.184875000000155));
#32926=CARTESIAN_POINT('Ctrl Pts',(-14.5339683530658,-17.1732158942094,
-0.226541666666823));
#32927=CARTESIAN_POINT('Ctrl Pts',(-13.5679367061317,-16.6154772628063,
-0.26820833333349));
#32928=CARTESIAN_POINT('Ctrl Pts',(-13.5679367061317,-15.5,-0.309875000000157));
#32929=CARTESIAN_POINT('Ctrl Pts',(-13.5679367061317,-14.3845227371938,
-0.351541666666825));
#32930=CARTESIAN_POINT('Ctrl Pts',(-14.5339683530658,-13.8267841057907,
-0.393208333333492));
#32931=CARTESIAN_POINT('Ctrl Pts',(-15.5,-13.2690454743876,-0.434875000000159));
#32932=CARTESIAN_POINT('Ctrl Pts',(-16.4660316469341,-13.8267841057907,
-0.476541666666826));
#32933=CARTESIAN_POINT('Ctrl Pts',(-17.4320632938682,-14.3845227371938,
-0.518208333333494));
#32934=CARTESIAN_POINT('Ctrl Pts',(-17.4320632938682,-15.5000000000001,
-0.559875000000161));
#32935=CARTESIAN_POINT('Ctrl Pts',(-17.4320632938682,-16.6154772628063,
-0.601541666666828));
#32936=CARTESIAN_POINT('Ctrl Pts',(-16.4660316469341,-17.1732158942094,
-0.643208333333495));
#32937=CARTESIAN_POINT('Ctrl Pts',(-15.4999999999999,-17.7309545256125,
-0.684875000000163));
#32938=CARTESIAN_POINT('Ctrl Pts',(-14.5339683530658,-17.1732158942094,
-0.72654166666683));
#32939=CARTESIAN_POINT('Ctrl Pts',(-13.5679367061317,-16.6154772628063,
-0.768208333333497));
#32940=CARTESIAN_POINT('Ctrl Pts',(-13.5679367061317,-15.5,-0.809875000000165));
#32941=CARTESIAN_POINT('Ctrl Pts',(-13.5679367061317,-14.3845227371938,
-0.851541666666832));
#32942=CARTESIAN_POINT('Ctrl Pts',(-14.5339683530658,-13.8267841057907,
-0.893208333333499));
#32943=CARTESIAN_POINT('Ctrl Pts',(-15.5,-13.2690454743876,-0.934875000000167));
#32944=CARTESIAN_POINT('Ctrl Pts',(-16.4660316469341,-13.8267841057907,
-0.976541666666834));
#32945=CARTESIAN_POINT('Ctrl Pts',(-17.4320632938682,-14.3845227371938,
-1.0182083333335));
#32946=CARTESIAN_POINT('Ctrl Pts',(-17.4320632938682,-15.5000000000001,
-1.05987500000017));
#32947=CARTESIAN_POINT('Ctrl Pts',(-17.4320632938682,-16.6154772628063,
-1.10154166666683));
#32948=CARTESIAN_POINT('Ctrl Pts',(-16.4660316469341,-17.1732158942094,
-1.1432083333335));
#32949=CARTESIAN_POINT('Ctrl Pts',(-15.4999999999999,-17.7309545256125,
-1.18487500000017));
#32950=CARTESIAN_POINT('Ctrl Pts',(-14.5339683530658,-17.1732158942094,
-1.22654166666684));
#32951=CARTESIAN_POINT('Ctrl Pts',(-13.5679367061317,-16.6154772628063,
-1.2682083333335));
#32952=CARTESIAN_POINT('Ctrl Pts',(-13.5679367061317,-15.5,-1.30987500000017));
#32953=CARTESIAN_POINT('Ctrl Pts',(-13.5679367061317,-14.3845227371938,
-1.35154166666684));
#32954=CARTESIAN_POINT('Ctrl Pts',(-14.5339683530658,-13.8267841057907,
-1.3932083333335));
#32955=CARTESIAN_POINT('Ctrl Pts',(-15.5,-13.2690454743876,-1.43487500000017));
#32956=CARTESIAN_POINT('Ctrl Pts',(-16.4660316469341,-13.8267841057907,
-1.47654166666684));
#32957=CARTESIAN_POINT('Ctrl Pts',(-17.4320632938682,-14.3845227371938,
-1.51820833333351));
#32958=CARTESIAN_POINT('Ctrl Pts',(-17.4320632938682,-15.5000000000001,
-1.55987500000017));
#32959=CARTESIAN_POINT('Ctrl Pts',(-17.4320632938682,-16.6154772628063,
-1.60154166666684));
#32960=CARTESIAN_POINT('Ctrl Pts',(-16.4660316469341,-17.1732158942094,
-1.64320833333351));
#32961=CARTESIAN_POINT('Ctrl Pts',(-15.4999999999999,-17.7309545256125,
-1.68487500000018));
#32962=CARTESIAN_POINT('Ctrl Pts',(-14.5339683530658,-17.1732158942094,
-1.72654166666684));
#32963=CARTESIAN_POINT('Ctrl Pts',(-14.1783081829977,-16.9678753992806,
-1.74188192368624));
#32964=CARTESIAN_POINT('Ctrl Pts',(-13.9369186715641,-16.6356255246376,
-1.75949830599533));
#32965=CARTESIAN_POINT('Ctrl Pts',(-17.0802357869868,-15.5000000000001,
11.2369972941937));
#32966=CARTESIAN_POINT('Ctrl Pts',(-17.0802357869868,-16.412349557,11.195330627527));
#32967=CARTESIAN_POINT('Ctrl Pts',(-16.2901178934934,-16.8685243355,11.1536639608604));
#32968=CARTESIAN_POINT('Ctrl Pts',(-15.4999999999999,-17.324699114,11.1119972941937));
#32969=CARTESIAN_POINT('Ctrl Pts',(-14.7098821065065,-16.8685243355,11.070330627527));
#32970=CARTESIAN_POINT('Ctrl Pts',(-13.9197642130131,-16.412349557,11.0286639608604));
#32971=CARTESIAN_POINT('Ctrl Pts',(-13.9197642130131,-15.5,10.9869972941937));
#32972=CARTESIAN_POINT('Ctrl Pts',(-13.9197642130131,-14.5876504430001,
10.945330627527));
#32973=CARTESIAN_POINT('Ctrl Pts',(-14.7098821065065,-14.1314756645001,
10.9036639608604));
#32974=CARTESIAN_POINT('Ctrl Pts',(-15.5,-13.6753008860002,10.8619972941937));
#32975=CARTESIAN_POINT('Ctrl Pts',(-16.2901178934934,-14.1314756645001,
10.820330627527));
#32976=CARTESIAN_POINT('Ctrl Pts',(-17.0802357869868,-14.5876504430001,
10.7786639608604));
#32977=CARTESIAN_POINT('Ctrl Pts',(-17.0802357869868,-15.5000000000001,
10.7369972941937));
#32978=CARTESIAN_POINT('Ctrl Pts',(-17.0802357869868,-16.412349557,10.695330627527));
#32979=CARTESIAN_POINT('Ctrl Pts',(-16.2901178934934,-16.8685243355,10.6536639608604));
#32980=CARTESIAN_POINT('Ctrl Pts',(-15.4999999999999,-17.324699114,10.6119972941937));
#32981=CARTESIAN_POINT('Ctrl Pts',(-14.7098821065065,-16.8685243355,10.570330627527));
#32982=CARTESIAN_POINT('Ctrl Pts',(-13.9197642130131,-16.412349557,10.5286639608604));
#32983=CARTESIAN_POINT('Ctrl Pts',(-13.9197642130131,-15.5,10.4869972941937));
#32984=CARTESIAN_POINT('Ctrl Pts',(-13.9197642130131,-14.5876504430001,
10.445330627527));
#32985=CARTESIAN_POINT('Ctrl Pts',(-14.7098821065065,-14.1314756645001,
10.4036639608604));
#32986=CARTESIAN_POINT('Ctrl Pts',(-15.5,-13.6753008860002,10.3619972941937));
#32987=CARTESIAN_POINT('Ctrl Pts',(-16.2901178934934,-14.1314756645001,
10.320330627527));
#32988=CARTESIAN_POINT('Ctrl Pts',(-17.0802357869868,-14.5876504430001,
10.2786639608604));
#32989=CARTESIAN_POINT('Ctrl Pts',(-17.0802357869868,-15.5000000000001,
10.2369972941937));
#32990=CARTESIAN_POINT('Ctrl Pts',(-17.0802357869868,-16.412349557,10.195330627527));
#32991=CARTESIAN_POINT('Ctrl Pts',(-16.2901178934934,-16.8685243355,10.1536639608604));
#32992=CARTESIAN_POINT('Ctrl Pts',(-15.4999999999999,-17.324699114,10.1119972941937));
#32993=CARTESIAN_POINT('Ctrl Pts',(-14.7098821065065,-16.8685243355,10.070330627527));
#32994=CARTESIAN_POINT('Ctrl Pts',(-13.9197642130131,-16.412349557,10.0286639608604));
#32995=CARTESIAN_POINT('Ctrl Pts',(-13.9197642130131,-15.5,9.98699729419369));
#32996=CARTESIAN_POINT('Ctrl Pts',(-13.9197642130131,-14.5876504430001,
9.94533062752702));
#32997=CARTESIAN_POINT('Ctrl Pts',(-14.7098821065065,-14.1314756645001,
9.90366396086035));
#32998=CARTESIAN_POINT('Ctrl Pts',(-15.5,-13.6753008860002,9.86199729419368));
#32999=CARTESIAN_POINT('Ctrl Pts',(-16.2901178934934,-14.1314756645001,
9.82033062752702));
#33000=CARTESIAN_POINT('Ctrl Pts',(-17.0802357869868,-14.5876504430001,
9.77866396086035));
#33001=CARTESIAN_POINT('Ctrl Pts',(-17.0802357869868,-15.5000000000001,
9.73699729419368));
#33002=CARTESIAN_POINT('Ctrl Pts',(-17.0802357869868,-16.412349557,9.69533062752702));
#33003=CARTESIAN_POINT('Ctrl Pts',(-16.2901178934934,-16.8685243355,9.65366396086035));
#33004=CARTESIAN_POINT('Ctrl Pts',(-15.4999999999999,-17.324699114,9.61199729419368));
#33005=CARTESIAN_POINT('Ctrl Pts',(-14.7098821065065,-16.8685243355,9.57033062752701));
#33006=CARTESIAN_POINT('Ctrl Pts',(-13.9197642130131,-16.412349557,9.52866396086034));
#33007=CARTESIAN_POINT('Ctrl Pts',(-13.9197642130131,-15.5,9.48699729419368));
#33008=CARTESIAN_POINT('Ctrl Pts',(-13.9197642130131,-14.5876504430001,
9.44533062752701));
#33009=CARTESIAN_POINT('Ctrl Pts',(-14.7098821065065,-14.1314756645001,
9.40366396086034));
#33010=CARTESIAN_POINT('Ctrl Pts',(-15.5,-13.6753008860002,9.36199729419368));
#33011=CARTESIAN_POINT('Ctrl Pts',(-16.2901178934934,-14.1314756645001,
9.32033062752701));
#33012=CARTESIAN_POINT('Ctrl Pts',(-17.0802357869868,-14.5876504430001,
9.27866396086035));
#33013=CARTESIAN_POINT('Ctrl Pts',(-17.0802357869868,-15.5000000000001,
9.23699729419368));
#33014=CARTESIAN_POINT('Ctrl Pts',(-17.0802357869868,-16.412349557,9.19533062752701));
#33015=CARTESIAN_POINT('Ctrl Pts',(-16.2901178934934,-16.8685243355,9.15366396086034));
#33016=CARTESIAN_POINT('Ctrl Pts',(-15.4999999999999,-17.324699114,9.11199729419368));
#33017=CARTESIAN_POINT('Ctrl Pts',(-14.7098821065065,-16.8685243355,9.07033062752701));
#33018=CARTESIAN_POINT('Ctrl Pts',(-13.9197642130131,-16.412349557,9.02866396086034));
#33019=CARTESIAN_POINT('Ctrl Pts',(-13.9197642130131,-15.5,8.98699729419367));
#33020=CARTESIAN_POINT('Ctrl Pts',(-13.9197642130131,-14.5876504430001,
8.94533062752701));
#33021=CARTESIAN_POINT('Ctrl Pts',(-14.7098821065065,-14.1314756645001,
8.90366396086034));
#33022=CARTESIAN_POINT('Ctrl Pts',(-15.5,-13.6753008860002,8.86199729419367));
#33023=CARTESIAN_POINT('Ctrl Pts',(-16.2901178934934,-14.1314756645001,
8.820330627527));
#33024=CARTESIAN_POINT('Ctrl Pts',(-17.0802357869868,-14.5876504430001,
8.77866396086034));
#33025=CARTESIAN_POINT('Ctrl Pts',(-17.0802357869868,-15.5000000000001,
8.73699729419367));
#33026=CARTESIAN_POINT('Ctrl Pts',(-17.0802357869868,-16.412349557,8.695330627527));
#33027=CARTESIAN_POINT('Ctrl Pts',(-16.2901178934934,-16.8685243355,8.65366396086033));
#33028=CARTESIAN_POINT('Ctrl Pts',(-15.4999999999999,-17.324699114,8.61199729419367));
#33029=CARTESIAN_POINT('Ctrl Pts',(-14.7098821065065,-16.8685243355,8.570330627527));
#33030=CARTESIAN_POINT('Ctrl Pts',(-13.9197642130131,-16.412349557,8.52866396086033));
#33031=CARTESIAN_POINT('Ctrl Pts',(-13.9197642130131,-15.5,8.48699729419366));
#33032=CARTESIAN_POINT('Ctrl Pts',(-13.9197642130131,-14.5876504430001,
8.445330627527));
#33033=CARTESIAN_POINT('Ctrl Pts',(-14.7098821065065,-14.1314756645001,
8.40366396086033));
#33034=CARTESIAN_POINT('Ctrl Pts',(-15.5,-13.6753008860002,8.36199729419366));
#33035=CARTESIAN_POINT('Ctrl Pts',(-16.2901178934934,-14.1314756645001,
8.320330627527));
#33036=CARTESIAN_POINT('Ctrl Pts',(-17.0802357869868,-14.5876504430001,
8.27866396086033));
#33037=CARTESIAN_POINT('Ctrl Pts',(-17.0802357869868,-15.5000000000001,
8.23699729419366));
#33038=CARTESIAN_POINT('Ctrl Pts',(-17.0802357869868,-16.412349557,8.19533062752699));
#33039=CARTESIAN_POINT('Ctrl Pts',(-16.2901178934934,-16.8685243355,8.15366396086033));
#33040=CARTESIAN_POINT('Ctrl Pts',(-15.4999999999999,-17.324699114,8.11199729419366));
#33041=CARTESIAN_POINT('Ctrl Pts',(-14.7098821065065,-16.8685243355,8.07033062752699));
#33042=CARTESIAN_POINT('Ctrl Pts',(-13.9197642130131,-16.412349557,8.02866396086033));
#33043=CARTESIAN_POINT('Ctrl Pts',(-13.9197642130131,-15.5,7.98699729419366));
#33044=CARTESIAN_POINT('Ctrl Pts',(-13.9197642130131,-14.5876504430001,
7.94533062752699));
#33045=CARTESIAN_POINT('Ctrl Pts',(-14.7098821065065,-14.1314756645001,
7.90366396086032));
#33046=CARTESIAN_POINT('Ctrl Pts',(-15.5,-13.6753008860002,7.86199729419366));
#33047=CARTESIAN_POINT('Ctrl Pts',(-16.2901178934934,-14.1314756645001,
7.82033062752699));
#33048=CARTESIAN_POINT('Ctrl Pts',(-17.0802357869868,-14.5876504430001,
7.77866396086032));
#33049=CARTESIAN_POINT('Ctrl Pts',(-17.0802357869868,-15.5000000000001,
7.73699729419366));
#33050=CARTESIAN_POINT('Ctrl Pts',(-17.0802357869868,-16.412349557,7.69533062752699));
#33051=CARTESIAN_POINT('Ctrl Pts',(-16.2901178934934,-16.8685243355,7.65366396086032));
#33052=CARTESIAN_POINT('Ctrl Pts',(-15.4999999999999,-17.324699114,7.61199729419365));
#33053=CARTESIAN_POINT('Ctrl Pts',(-14.7098821065065,-16.8685243355,7.57033062752699));
#33054=CARTESIAN_POINT('Ctrl Pts',(-13.9197642130131,-16.412349557,7.52866396086032));
#33055=CARTESIAN_POINT('Ctrl Pts',(-13.9197642130131,-15.5,7.48699729419365));
#33056=CARTESIAN_POINT('Ctrl Pts',(-13.9197642130131,-14.5876504430001,
7.44533062752699));
#33057=CARTESIAN_POINT('Ctrl Pts',(-14.7098821065065,-14.1314756645001,
7.40366396086032));
#33058=CARTESIAN_POINT('Ctrl Pts',(-15.5,-13.6753008860002,7.36199729419365));
#33059=CARTESIAN_POINT('Ctrl Pts',(-16.2901178934934,-14.1314756645001,
7.32033062752699));
#33060=CARTESIAN_POINT('Ctrl Pts',(-17.0802357869868,-14.5876504430001,
7.27866396086032));
#33061=CARTESIAN_POINT('Ctrl Pts',(-17.0802357869868,-15.5000000000001,
7.23699729419365));
#33062=CARTESIAN_POINT('Ctrl Pts',(-17.0802357869868,-16.412349557,7.19533062752698));
#33063=CARTESIAN_POINT('Ctrl Pts',(-16.2901178934934,-16.8685243355,7.15366396086031));
#33064=CARTESIAN_POINT('Ctrl Pts',(-15.4999999999999,-17.324699114,7.11199729419365));
#33065=CARTESIAN_POINT('Ctrl Pts',(-14.7098821065065,-16.8685243355,7.07033062752698));
#33066=CARTESIAN_POINT('Ctrl Pts',(-13.9197642130131,-16.412349557,7.02866396086031));
#33067=CARTESIAN_POINT('Ctrl Pts',(-13.9197642130131,-15.5,6.98699729419364));
#33068=CARTESIAN_POINT('Ctrl Pts',(-13.9197642130131,-14.5876504430001,
6.94533062752698));
#33069=CARTESIAN_POINT('Ctrl Pts',(-14.7098821065065,-14.1314756645001,
6.90366396086031));
#33070=CARTESIAN_POINT('Ctrl Pts',(-15.5,-13.6753008860002,6.86199729419364));
#33071=CARTESIAN_POINT('Ctrl Pts',(-16.2901178934934,-14.1314756645001,
6.82033062752698));
#33072=CARTESIAN_POINT('Ctrl Pts',(-17.0802357869868,-14.5876504430001,
6.77866396086031));
#33073=CARTESIAN_POINT('Ctrl Pts',(-17.0802357869868,-15.5000000000001,
6.73699729419364));
#33074=CARTESIAN_POINT('Ctrl Pts',(-17.0802357869868,-16.412349557,6.69533062752697));
#33075=CARTESIAN_POINT('Ctrl Pts',(-16.2901178934934,-16.8685243355,6.65366396086031));
#33076=CARTESIAN_POINT('Ctrl Pts',(-15.4999999999999,-17.324699114,6.61199729419364));
#33077=CARTESIAN_POINT('Ctrl Pts',(-14.7098821065065,-16.8685243355,6.57033062752697));
#33078=CARTESIAN_POINT('Ctrl Pts',(-13.9197642130131,-16.412349557,6.52866396086031));
#33079=CARTESIAN_POINT('Ctrl Pts',(-13.9197642130131,-15.5,6.48699729419364));
#33080=CARTESIAN_POINT('Ctrl Pts',(-13.9197642130131,-14.5876504430001,
6.44533062752697));
#33081=CARTESIAN_POINT('Ctrl Pts',(-14.7098821065065,-14.1314756645001,
6.40366396086031));
#33082=CARTESIAN_POINT('Ctrl Pts',(-15.5,-13.6753008860002,6.36199729419364));
#33083=CARTESIAN_POINT('Ctrl Pts',(-16.2901178934934,-14.1314756645001,
6.32033062752697));
#33084=CARTESIAN_POINT('Ctrl Pts',(-17.0802357869868,-14.5876504430001,
6.2786639608603));
#33085=CARTESIAN_POINT('Ctrl Pts',(-17.0802357869868,-15.5000000000001,
6.23699729419364));
#33086=CARTESIAN_POINT('Ctrl Pts',(-17.0802357869868,-16.412349557,6.19533062752697));
#33087=CARTESIAN_POINT('Ctrl Pts',(-16.2901178934934,-16.8685243355,6.1536639608603));
#33088=CARTESIAN_POINT('Ctrl Pts',(-15.4999999999999,-17.324699114,6.11199729419363));
#33089=CARTESIAN_POINT('Ctrl Pts',(-14.7098821065065,-16.8685243355,6.07033062752697));
#33090=CARTESIAN_POINT('Ctrl Pts',(-13.9197642130131,-16.412349557,6.0286639608603));
#33091=CARTESIAN_POINT('Ctrl Pts',(-13.9197642130131,-15.5,5.98699729419363));
#33092=CARTESIAN_POINT('Ctrl Pts',(-13.9197642130131,-14.5876504430001,
5.94533062752696));
#33093=CARTESIAN_POINT('Ctrl Pts',(-14.7098821065065,-14.1314756645001,
5.9036639608603));
#33094=CARTESIAN_POINT('Ctrl Pts',(-15.5,-13.6753008860002,5.86199729419363));
#33095=CARTESIAN_POINT('Ctrl Pts',(-16.2901178934934,-14.1314756645001,
5.82033062752696));
#33096=CARTESIAN_POINT('Ctrl Pts',(-17.0802357869868,-14.5876504430001,
5.7786639608603));
#33097=CARTESIAN_POINT('Ctrl Pts',(-17.0802357869868,-15.5000000000001,
5.73699729419363));
#33098=CARTESIAN_POINT('Ctrl Pts',(-17.0802357869868,-16.412349557,5.69533062752696));
#33099=CARTESIAN_POINT('Ctrl Pts',(-16.2901178934934,-16.8685243355,5.65366396086029));
#33100=CARTESIAN_POINT('Ctrl Pts',(-15.4999999999999,-17.324699114,5.61199729419363));
#33101=CARTESIAN_POINT('Ctrl Pts',(-14.7098821065065,-16.8685243355,5.57033062752696));
#33102=CARTESIAN_POINT('Ctrl Pts',(-13.9197642130131,-16.412349557,5.52866396086029));
#33103=CARTESIAN_POINT('Ctrl Pts',(-13.9197642130131,-15.5,5.48699729419363));
#33104=CARTESIAN_POINT('Ctrl Pts',(-13.9197642130131,-14.5876504430001,
5.44533062752696));
#33105=CARTESIAN_POINT('Ctrl Pts',(-14.7098821065065,-14.1314756645001,
5.40366396086029));
#33106=CARTESIAN_POINT('Ctrl Pts',(-15.5,-13.6753008860002,5.36199729419362));
#33107=CARTESIAN_POINT('Ctrl Pts',(-16.2901178934934,-14.1314756645001,
5.32033062752696));
#33108=CARTESIAN_POINT('Ctrl Pts',(-17.0802357869868,-14.5876504430001,
5.27866396086029));
#33109=CARTESIAN_POINT('Ctrl Pts',(-17.0802357869868,-15.5000000000001,
5.23699729419362));
#33110=CARTESIAN_POINT('Ctrl Pts',(-17.0802357869868,-16.412349557,5.19533062752695));
#33111=CARTESIAN_POINT('Ctrl Pts',(-16.2901178934934,-16.8685243355,5.15366396086029));
#33112=CARTESIAN_POINT('Ctrl Pts',(-15.4999999999999,-17.324699114,5.11199729419362));
#33113=CARTESIAN_POINT('Ctrl Pts',(-14.7098821065065,-16.8685243355,5.07033062752695));
#33114=CARTESIAN_POINT('Ctrl Pts',(-13.9197642130131,-16.412349557,5.02866396086029));
#33115=CARTESIAN_POINT('Ctrl Pts',(-13.9197642130131,-15.5,4.98699729419362));
#33116=CARTESIAN_POINT('Ctrl Pts',(-13.9197642130131,-14.5876504430001,
4.94533062752695));
#33117=CARTESIAN_POINT('Ctrl Pts',(-14.7098821065065,-14.1314756645001,
4.90366396086028));
#33118=CARTESIAN_POINT('Ctrl Pts',(-15.5,-13.6753008860002,4.86199729419362));
#33119=CARTESIAN_POINT('Ctrl Pts',(-16.2901178934934,-14.1314756645001,
4.82033062752695));
#33120=CARTESIAN_POINT('Ctrl Pts',(-17.0802357869868,-14.5876504430001,
4.77866396086028));
#33121=CARTESIAN_POINT('Ctrl Pts',(-17.0802357869868,-15.5000000000001,
4.73699729419362));
#33122=CARTESIAN_POINT('Ctrl Pts',(-17.0802357869868,-16.412349557,4.69533062752695));
#33123=CARTESIAN_POINT('Ctrl Pts',(-16.2901178934934,-16.8685243355,4.65366396086028));
#33124=CARTESIAN_POINT('Ctrl Pts',(-15.4999999999999,-17.324699114,4.61199729419361));
#33125=CARTESIAN_POINT('Ctrl Pts',(-14.7098821065065,-16.8685243355,4.57033062752695));
#33126=CARTESIAN_POINT('Ctrl Pts',(-13.9197642130131,-16.412349557,4.52866396086028));
#33127=CARTESIAN_POINT('Ctrl Pts',(-13.9197642130131,-15.5,4.48699729419361));
#33128=CARTESIAN_POINT('Ctrl Pts',(-13.9197642130131,-14.5876504430001,
4.44533062752694));
#33129=CARTESIAN_POINT('Ctrl Pts',(-14.7098821065065,-14.1314756645001,
4.40366396086028));
#33130=CARTESIAN_POINT('Ctrl Pts',(-15.5,-13.6753008860002,4.36199729419361));
#33131=CARTESIAN_POINT('Ctrl Pts',(-16.2901178934934,-14.1314756645001,
4.32033062752694));
#33132=CARTESIAN_POINT('Ctrl Pts',(-17.0802357869868,-14.5876504430001,
4.27866396086028));
#33133=CARTESIAN_POINT('Ctrl Pts',(-17.0802357869868,-15.5000000000001,
4.23699729419361));
#33134=CARTESIAN_POINT('Ctrl Pts',(-17.0802357869868,-16.412349557,4.19533062752694));
#33135=CARTESIAN_POINT('Ctrl Pts',(-16.2901178934934,-16.8685243355,4.15366396086027));
#33136=CARTESIAN_POINT('Ctrl Pts',(-15.4999999999999,-17.324699114,4.11199729419361));
#33137=CARTESIAN_POINT('Ctrl Pts',(-14.7098821065065,-16.8685243355,4.07033062752694));
#33138=CARTESIAN_POINT('Ctrl Pts',(-13.9197642130131,-16.412349557,4.02866396086027));
#33139=CARTESIAN_POINT('Ctrl Pts',(-13.9197642130131,-15.5,3.9869972941936));
#33140=CARTESIAN_POINT('Ctrl Pts',(-13.9197642130131,-14.5876504430001,
3.94533062752694));
#33141=CARTESIAN_POINT('Ctrl Pts',(-14.7098821065065,-14.1314756645001,
3.90366396086027));
#33142=CARTESIAN_POINT('Ctrl Pts',(-15.5,-13.6753008860002,3.8619972941936));
#33143=CARTESIAN_POINT('Ctrl Pts',(-16.2901178934934,-14.1314756645001,
3.82033062752694));
#33144=CARTESIAN_POINT('Ctrl Pts',(-17.0802357869868,-14.5876504430001,
3.77866396086027));
#33145=CARTESIAN_POINT('Ctrl Pts',(-17.0802357869868,-15.5000000000001,
3.7369972941936));
#33146=CARTESIAN_POINT('Ctrl Pts',(-17.0802357869868,-16.412349557,3.69533062752693));
#33147=CARTESIAN_POINT('Ctrl Pts',(-16.2901178934934,-16.8685243355,3.65366396086027));
#33148=CARTESIAN_POINT('Ctrl Pts',(-15.4999999999999,-17.324699114,3.6119972941936));
#33149=CARTESIAN_POINT('Ctrl Pts',(-14.7098821065065,-16.8685243355,3.57033062752693));
#33150=CARTESIAN_POINT('Ctrl Pts',(-13.9197642130131,-16.412349557,3.52866396086027));
#33151=CARTESIAN_POINT('Ctrl Pts',(-13.9197642130131,-15.5,3.4869972941936));
#33152=CARTESIAN_POINT('Ctrl Pts',(-13.9197642130131,-14.5876504430001,
3.44533062752693));
#33153=CARTESIAN_POINT('Ctrl Pts',(-14.7098821065065,-14.1314756645001,
3.40366396086026));
#33154=CARTESIAN_POINT('Ctrl Pts',(-15.5,-13.6753008860002,3.3619972941936));
#33155=CARTESIAN_POINT('Ctrl Pts',(-16.2901178934934,-14.1314756645001,
3.32033062752693));
#33156=CARTESIAN_POINT('Ctrl Pts',(-17.0802357869868,-14.5876504430001,
3.27866396086026));
#33157=CARTESIAN_POINT('Ctrl Pts',(-17.0802357869868,-15.5000000000001,
3.2369972941936));
#33158=CARTESIAN_POINT('Ctrl Pts',(-17.0802357869868,-16.412349557,3.19533062752693));
#33159=CARTESIAN_POINT('Ctrl Pts',(-16.2901178934934,-16.8685243355,3.15366396086026));
#33160=CARTESIAN_POINT('Ctrl Pts',(-15.4999999999999,-17.324699114,3.11199729419359));
#33161=CARTESIAN_POINT('Ctrl Pts',(-14.7098821065065,-16.8685243355,3.07033062752693));
#33162=CARTESIAN_POINT('Ctrl Pts',(-13.9197642130131,-16.412349557,3.02866396086026));
#33163=CARTESIAN_POINT('Ctrl Pts',(-13.9197642130131,-15.5,2.98699729419359));
#33164=CARTESIAN_POINT('Ctrl Pts',(-13.9197642130131,-14.5876504430001,
2.94533062752692));
#33165=CARTESIAN_POINT('Ctrl Pts',(-14.7098821065065,-14.1314756645001,
2.90366396086026));
#33166=CARTESIAN_POINT('Ctrl Pts',(-15.5,-13.6753008860002,2.86199729419359));
#33167=CARTESIAN_POINT('Ctrl Pts',(-16.2901178934934,-14.1314756645001,
2.82033062752692));
#33168=CARTESIAN_POINT('Ctrl Pts',(-17.0802357869868,-14.5876504430001,
2.77866396086026));
#33169=CARTESIAN_POINT('Ctrl Pts',(-17.0802357869868,-15.5000000000001,
2.73699729419359));
#33170=CARTESIAN_POINT('Ctrl Pts',(-17.0802357869868,-16.412349557,2.69533062752692));
#33171=CARTESIAN_POINT('Ctrl Pts',(-16.2901178934934,-16.8685243355,2.65366396086025));
#33172=CARTESIAN_POINT('Ctrl Pts',(-15.4999999999999,-17.324699114,2.61199729419359));
#33173=CARTESIAN_POINT('Ctrl Pts',(-14.7098821065065,-16.8685243355,2.57033062752692));
#33174=CARTESIAN_POINT('Ctrl Pts',(-13.9197642130131,-16.412349557,2.52866396086025));
#33175=CARTESIAN_POINT('Ctrl Pts',(-13.9197642130131,-15.5,2.48699729419358));
#33176=CARTESIAN_POINT('Ctrl Pts',(-13.9197642130131,-14.5876504430001,
2.44533062752692));
#33177=CARTESIAN_POINT('Ctrl Pts',(-14.7098821065065,-14.1314756645001,
2.40366396086025));
#33178=CARTESIAN_POINT('Ctrl Pts',(-15.5,-13.6753008860002,2.36199729419358));
#33179=CARTESIAN_POINT('Ctrl Pts',(-16.2901178934934,-14.1314756645001,
2.32033062752692));
#33180=CARTESIAN_POINT('Ctrl Pts',(-17.0802357869868,-14.5876504430001,
2.27866396086025));
#33181=CARTESIAN_POINT('Ctrl Pts',(-17.0802357869868,-15.5000000000001,
2.23699729419358));
#33182=CARTESIAN_POINT('Ctrl Pts',(-17.0802357869868,-16.412349557,2.19533062752692));
#33183=CARTESIAN_POINT('Ctrl Pts',(-16.2901178934934,-16.8685243355,2.15366396086025));
#33184=CARTESIAN_POINT('Ctrl Pts',(-15.4999999999999,-17.324699114,2.11199729419358));
#33185=CARTESIAN_POINT('Ctrl Pts',(-14.7098821065065,-16.8685243355,2.07033062752691));
#33186=CARTESIAN_POINT('Ctrl Pts',(-13.9197642130131,-16.412349557,2.02866396086025));
#33187=CARTESIAN_POINT('Ctrl Pts',(-13.9197642130131,-15.5,1.98699729419358));
#33188=CARTESIAN_POINT('Ctrl Pts',(-13.9197642130131,-14.5876504430001,
1.94533062752691));
#33189=CARTESIAN_POINT('Ctrl Pts',(-14.7098821065065,-14.1314756645001,
1.90366396086024));
#33190=CARTESIAN_POINT('Ctrl Pts',(-15.5,-13.6753008860002,1.86199729419358));
#33191=CARTESIAN_POINT('Ctrl Pts',(-16.2901178934934,-14.1314756645001,
1.82033062752691));
#33192=CARTESIAN_POINT('Ctrl Pts',(-17.0802357869868,-14.5876504430001,
1.77866396086024));
#33193=CARTESIAN_POINT('Ctrl Pts',(-17.0802357869868,-15.5000000000001,
1.73699729419358));
#33194=CARTESIAN_POINT('Ctrl Pts',(-17.0802357869868,-16.412349557,1.69533062752691));
#33195=CARTESIAN_POINT('Ctrl Pts',(-16.2901178934934,-16.8685243355,1.65366396086024));
#33196=CARTESIAN_POINT('Ctrl Pts',(-15.4999999999999,-17.324699114,1.61199729419357));
#33197=CARTESIAN_POINT('Ctrl Pts',(-14.7098821065065,-16.8685243355,1.57033062752691));
#33198=CARTESIAN_POINT('Ctrl Pts',(-13.9197642130131,-16.412349557,1.52866396086024));
#33199=CARTESIAN_POINT('Ctrl Pts',(-13.9197642130131,-15.5,1.48699729419357));
#33200=CARTESIAN_POINT('Ctrl Pts',(-13.9197642130131,-14.5876504430001,
1.4453306275269));
#33201=CARTESIAN_POINT('Ctrl Pts',(-14.7098821065065,-14.1314756645001,
1.40366396086024));
#33202=CARTESIAN_POINT('Ctrl Pts',(-15.5,-13.6753008860002,1.36199729419357));
#33203=CARTESIAN_POINT('Ctrl Pts',(-16.2901178934934,-14.1314756645001,
1.3203306275269));
#33204=CARTESIAN_POINT('Ctrl Pts',(-17.0802357869868,-14.5876504430001,
1.27866396086024));
#33205=CARTESIAN_POINT('Ctrl Pts',(-17.0802357869868,-15.5000000000001,
1.23699729419357));
#33206=CARTESIAN_POINT('Ctrl Pts',(-17.0802357869868,-16.412349557,1.1953306275269));
#33207=CARTESIAN_POINT('Ctrl Pts',(-16.2901178934934,-16.8685243355,1.15366396086024));
#33208=CARTESIAN_POINT('Ctrl Pts',(-15.4999999999999,-17.324699114,1.11199729419357));
#33209=CARTESIAN_POINT('Ctrl Pts',(-14.7098821065065,-16.8685243355,1.0703306275269));
#33210=CARTESIAN_POINT('Ctrl Pts',(-13.9197642130131,-16.412349557,1.02866396086023));
#33211=CARTESIAN_POINT('Ctrl Pts',(-13.9197642130131,-15.5,0.986997294193569));
#33212=CARTESIAN_POINT('Ctrl Pts',(-13.9197642130131,-14.5876504430001,
0.945330627526902));
#33213=CARTESIAN_POINT('Ctrl Pts',(-14.7098821065065,-14.1314756645001,
0.903663960860235));
#33214=CARTESIAN_POINT('Ctrl Pts',(-15.5,-13.6753008860002,0.861997294193567));
#33215=CARTESIAN_POINT('Ctrl Pts',(-16.2901178934934,-14.1314756645001,
0.8203306275269));
#33216=CARTESIAN_POINT('Ctrl Pts',(-17.0802357869868,-14.5876504430001,
0.778663960860232));
#33217=CARTESIAN_POINT('Ctrl Pts',(-17.0802357869868,-15.5000000000001,
0.736997294193565));
#33218=CARTESIAN_POINT('Ctrl Pts',(-17.0802357869868,-16.412349557,0.695330627526898));
#33219=CARTESIAN_POINT('Ctrl Pts',(-16.2901178934934,-16.8685243355,0.653663960860231));
#33220=CARTESIAN_POINT('Ctrl Pts',(-15.4999999999999,-17.324699114,0.611997294193563));
#33221=CARTESIAN_POINT('Ctrl Pts',(-14.7098821065065,-16.8685243355,0.570330627526896));
#33222=CARTESIAN_POINT('Ctrl Pts',(-13.9197642130131,-16.412349557,0.528663960860229));
#33223=CARTESIAN_POINT('Ctrl Pts',(-13.9197642130131,-15.5,0.486997294193562));
#33224=CARTESIAN_POINT('Ctrl Pts',(-13.9197642130131,-14.5876504430001,
0.445330627526894));
#33225=CARTESIAN_POINT('Ctrl Pts',(-14.7098821065065,-14.1314756645001,
0.403663960860227));
#33226=CARTESIAN_POINT('Ctrl Pts',(-15.5,-13.6753008860002,0.36199729419356));
#33227=CARTESIAN_POINT('Ctrl Pts',(-16.2901178934934,-14.1314756645001,
0.320330627526892));
#33228=CARTESIAN_POINT('Ctrl Pts',(-17.0802357869868,-14.5876504430001,
0.278663960860225));
#33229=CARTESIAN_POINT('Ctrl Pts',(-17.0802357869868,-15.5000000000001,
0.236997294193558));
#33230=CARTESIAN_POINT('Ctrl Pts',(-17.0802357869868,-16.412349557,0.195330627526891));
#33231=CARTESIAN_POINT('Ctrl Pts',(-16.2901178934934,-16.8685243355,0.153663960860223));
#33232=CARTESIAN_POINT('Ctrl Pts',(-15.4999999999999,-17.324699114,0.111997294193556));
#33233=CARTESIAN_POINT('Ctrl Pts',(-14.7098821065065,-16.8685243355,0.0703306275268884));
#33234=CARTESIAN_POINT('Ctrl Pts',(-13.9197642130131,-16.412349557,0.0286639608602211));
#33235=CARTESIAN_POINT('Ctrl Pts',(-13.9197642130131,-15.5,-0.0130027058064461));
#33236=CARTESIAN_POINT('Ctrl Pts',(-13.9197642130131,-14.5876504430001,
-0.0546693724731117));
#33237=CARTESIAN_POINT('Ctrl Pts',(-14.7098821065065,-14.1314756645001,
-0.096336039139779));
#33238=CARTESIAN_POINT('Ctrl Pts',(-15.5,-13.6753008860002,-0.138002705806446));
#33239=CARTESIAN_POINT('Ctrl Pts',(-16.2901178934934,-14.1314756645001,
-0.179669372473113));
#33240=CARTESIAN_POINT('Ctrl Pts',(-17.0802357869868,-14.5876504430001,
-0.221336039139781));
#33241=CARTESIAN_POINT('Ctrl Pts',(-17.0802357869868,-15.5000000000001,
-0.263002705806448));
#33242=CARTESIAN_POINT('Ctrl Pts',(-17.0802357869868,-16.412349557,-0.304669372473115));
#33243=CARTESIAN_POINT('Ctrl Pts',(-16.2901178934934,-16.8685243355,-0.346336039139782));
#33244=CARTESIAN_POINT('Ctrl Pts',(-15.4999999999999,-17.324699114,-0.38800270580645));
#33245=CARTESIAN_POINT('Ctrl Pts',(-14.7098821065065,-16.8685243355,-0.429669372473117));
#33246=CARTESIAN_POINT('Ctrl Pts',(-13.9197642130131,-16.412349557,-0.471336039139784));
#33247=CARTESIAN_POINT('Ctrl Pts',(-13.9197642130131,-15.5,-0.513002705806452));
#33248=CARTESIAN_POINT('Ctrl Pts',(-13.9197642130131,-14.5876504430001,
-0.554669372473119));
#33249=CARTESIAN_POINT('Ctrl Pts',(-14.7098821065065,-14.1314756645001,
-0.596336039139786));
#33250=CARTESIAN_POINT('Ctrl Pts',(-15.5,-13.6753008860002,-0.638002705806453));
#33251=CARTESIAN_POINT('Ctrl Pts',(-16.2901178934934,-14.1314756645001,
-0.679669372473122));
#33252=CARTESIAN_POINT('Ctrl Pts',(-17.0802357869868,-14.5876504430001,
-0.721336039139788));
#33253=CARTESIAN_POINT('Ctrl Pts',(-17.0802357869868,-15.5000000000001,
-0.763002705806455));
#33254=CARTESIAN_POINT('Ctrl Pts',(-17.0802357869868,-16.412349557,-0.804669372473123));
#33255=CARTESIAN_POINT('Ctrl Pts',(-16.2901178934934,-16.8685243355,-0.84633603913979));
#33256=CARTESIAN_POINT('Ctrl Pts',(-15.4999999999999,-17.324699114,-0.888002705806457));
#33257=CARTESIAN_POINT('Ctrl Pts',(-14.7098821065065,-16.8685243355,-0.929669372473124));
#33258=CARTESIAN_POINT('Ctrl Pts',(-13.9197642130131,-16.412349557,-0.971336039139791));
#33259=CARTESIAN_POINT('Ctrl Pts',(-13.9197642130131,-15.5,-1.01300270580646));
#33260=CARTESIAN_POINT('Ctrl Pts',(-13.9197642130131,-14.5876504430001,
-1.05466937247313));
#33261=CARTESIAN_POINT('Ctrl Pts',(-14.7098821065065,-14.1314756645001,
-1.0963360391398));
#33262=CARTESIAN_POINT('Ctrl Pts',(-15.5,-13.6753008860002,-1.13800270580646));
#33263=CARTESIAN_POINT('Ctrl Pts',(-16.2901178934934,-14.1314756645001,
-1.17966937247313));
#33264=CARTESIAN_POINT('Ctrl Pts',(-17.0802357869868,-14.5876504430001,
-1.2213360391398));
#33265=CARTESIAN_POINT('Ctrl Pts',(-17.0802357869868,-15.5000000000001,
-1.26300270580646));
#33266=CARTESIAN_POINT('Ctrl Pts',(-17.0802357869868,-16.412349557,-1.30466937247313));
#33267=CARTESIAN_POINT('Ctrl Pts',(-16.2901178934934,-16.8685243355,-1.3463360391398));
#33268=CARTESIAN_POINT('Ctrl Pts',(-15.4999999999999,-17.324699114,-1.38800270580647));
#33269=CARTESIAN_POINT('Ctrl Pts',(-14.7098821065065,-16.8685243355,-1.42966937247313));
#33270=CARTESIAN_POINT('Ctrl Pts',(-13.9197642130131,-16.412349557,-1.4713360391398));
#33271=CARTESIAN_POINT('Ctrl Pts',(-13.9197642130131,-15.5,-1.51300270580647));
#33272=CARTESIAN_POINT('Ctrl Pts',(-13.9197642130131,-14.5876504430001,
-1.55466937247313));
#33273=CARTESIAN_POINT('Ctrl Pts',(-14.7098821065065,-14.1314756645001,
-1.5963360391398));
#33274=CARTESIAN_POINT('Ctrl Pts',(-15.5,-13.6753008860002,-1.63800270580647));
#33275=CARTESIAN_POINT('Ctrl Pts',(-16.2901178934934,-14.1314756645001,
-1.67966937247314));
#33276=CARTESIAN_POINT('Ctrl Pts',(-17.0802357869868,-14.5876504430001,
-1.7213360391398));
#33277=CARTESIAN_POINT('Ctrl Pts',(-17.0802357869868,-15.5000000000001,
-1.76300270580647));
#33278=CARTESIAN_POINT('Ctrl Pts',(-17.0802357869868,-16.412349557,-1.80466937247314));
#33279=CARTESIAN_POINT('Ctrl Pts',(-16.2901178934934,-16.8685243355,-1.84633603913981));
#33280=CARTESIAN_POINT('Ctrl Pts',(-15.4999999999999,-17.324699114,-1.88800270580647));
#33281=CARTESIAN_POINT('Ctrl Pts',(-14.7098821065065,-16.8685243355,-1.92966937247314));
#33282=CARTESIAN_POINT('Ctrl Pts',(-14.4189874290231,-16.700576215149,-1.94500962949253));
#33283=CARTESIAN_POINT('Ctrl Pts',(-14.2215547953297,-16.4288288330633,
-1.96262601180163));
#33284=CARTESIAN_POINT('',(-14.2215509627456,-16.4288315898517,-1.96262324186735));
#33285=CARTESIAN_POINT('',(-14.2215500160356,-16.4288304039466,-1.96262332703659));
#33286=CARTESIAN_POINT('Ctrl Pts',(-14.5577749122402,-14.2313898004749,
10.4122404735808));
#33287=CARTESIAN_POINT('Ctrl Pts',(-14.6309457974487,-14.1770441521709,
10.407829216981));
#33288=CARTESIAN_POINT('Ctrl Pts',(-14.7098797632095,-14.1314716057907,
10.4036666666667));
#33289=CARTESIAN_POINT('Ctrl Pts',(-15.5,-13.6752954743876,10.362));
#33290=CARTESIAN_POINT('Ctrl Pts',(-16.2901202367904,-14.1314716057907,
10.3203333333333));
#33291=CARTESIAN_POINT('Ctrl Pts',(-17.0802404735808,-14.5876477371938,
10.2786666666667));
#33292=CARTESIAN_POINT('Ctrl Pts',(-17.0802404735808,-15.5000000000001,
10.237));
#33293=CARTESIAN_POINT('Ctrl Pts',(-17.0802404735808,-16.4123522628063,
10.1953333333333));
#33294=CARTESIAN_POINT('Ctrl Pts',(-16.2901202367904,-16.8685283942094,
10.1536666666667));
#33295=CARTESIAN_POINT('Ctrl Pts',(-15.4999999999999,-17.3247045256125,
10.112));
#33296=CARTESIAN_POINT('Ctrl Pts',(-14.7098797632095,-16.8685283942094,
10.0703333333333));
#33297=CARTESIAN_POINT('Ctrl Pts',(-13.9197595264191,-16.4123522628063,
10.0286666666667));
#33298=CARTESIAN_POINT('Ctrl Pts',(-13.9197595264191,-15.5,9.98699999999998));
#33299=CARTESIAN_POINT('Ctrl Pts',(-13.9197595264191,-14.5876477371938,
9.94533333333331));
#33300=CARTESIAN_POINT('Ctrl Pts',(-14.7098797632095,-14.1314716057907,
9.90366666666665));
#33301=CARTESIAN_POINT('Ctrl Pts',(-15.5,-13.6752954743876,9.86199999999998));
#33302=CARTESIAN_POINT('Ctrl Pts',(-16.2901202367904,-14.1314716057907,
9.82033333333331));
#33303=CARTESIAN_POINT('Ctrl Pts',(-17.0802404735808,-14.5876477371938,
9.77866666666665));
#33304=CARTESIAN_POINT('Ctrl Pts',(-17.0802404735808,-15.5000000000001,
9.73699999999998));
#33305=CARTESIAN_POINT('Ctrl Pts',(-17.0802404735808,-16.4123522628063,
9.69533333333331));
#33306=CARTESIAN_POINT('Ctrl Pts',(-16.2901202367904,-16.8685283942094,
9.65366666666664));
#33307=CARTESIAN_POINT('Ctrl Pts',(-15.4999999999999,-17.3247045256125,
9.61199999999998));
#33308=CARTESIAN_POINT('Ctrl Pts',(-14.7098797632095,-16.8685283942094,
9.57033333333331));
#33309=CARTESIAN_POINT('Ctrl Pts',(-13.9197595264191,-16.4123522628063,
9.52866666666664));
#33310=CARTESIAN_POINT('Ctrl Pts',(-13.9197595264191,-15.5,9.48699999999998));
#33311=CARTESIAN_POINT('Ctrl Pts',(-13.9197595264191,-14.5876477371938,
9.44533333333331));
#33312=CARTESIAN_POINT('Ctrl Pts',(-14.7098797632095,-14.1314716057907,
9.40366666666664));
#33313=CARTESIAN_POINT('Ctrl Pts',(-15.5,-13.6752954743876,9.36199999999998));
#33314=CARTESIAN_POINT('Ctrl Pts',(-16.2901202367904,-14.1314716057907,
9.32033333333331));
#33315=CARTESIAN_POINT('Ctrl Pts',(-17.0802404735808,-14.5876477371938,
9.27866666666664));
#33316=CARTESIAN_POINT('Ctrl Pts',(-17.0802404735808,-15.5000000000001,
9.23699999999997));
#33317=CARTESIAN_POINT('Ctrl Pts',(-17.0802404735808,-16.4123522628063,
9.19533333333331));
#33318=CARTESIAN_POINT('Ctrl Pts',(-16.2901202367904,-16.8685283942094,
9.15366666666664));
#33319=CARTESIAN_POINT('Ctrl Pts',(-15.4999999999999,-17.3247045256125,
9.11199999999997));
#33320=CARTESIAN_POINT('Ctrl Pts',(-14.7098797632095,-16.8685283942094,
9.0703333333333));
#33321=CARTESIAN_POINT('Ctrl Pts',(-13.9197595264191,-16.4123522628063,
9.02866666666664));
#33322=CARTESIAN_POINT('Ctrl Pts',(-13.9197595264191,-15.5,8.98699999999997));
#33323=CARTESIAN_POINT('Ctrl Pts',(-13.9197595264191,-14.5876477371938,
8.9453333333333));
#33324=CARTESIAN_POINT('Ctrl Pts',(-14.7098797632095,-14.1314716057907,
8.90366666666664));
#33325=CARTESIAN_POINT('Ctrl Pts',(-15.5,-13.6752954743876,8.86199999999997));
#33326=CARTESIAN_POINT('Ctrl Pts',(-16.2901202367904,-14.1314716057907,
8.8203333333333));
#33327=CARTESIAN_POINT('Ctrl Pts',(-17.0802404735808,-14.5876477371938,
8.77866666666663));
#33328=CARTESIAN_POINT('Ctrl Pts',(-17.0802404735808,-15.5000000000001,
8.73699999999997));
#33329=CARTESIAN_POINT('Ctrl Pts',(-17.0802404735808,-16.4123522628063,
8.6953333333333));
#33330=CARTESIAN_POINT('Ctrl Pts',(-16.2901202367904,-16.8685283942094,
8.65366666666663));
#33331=CARTESIAN_POINT('Ctrl Pts',(-15.4999999999999,-17.3247045256125,
8.61199999999996));
#33332=CARTESIAN_POINT('Ctrl Pts',(-14.7098797632095,-16.8685283942094,
8.57033333333329));
#33333=CARTESIAN_POINT('Ctrl Pts',(-13.9197595264191,-16.4123522628063,
8.52866666666663));
#33334=CARTESIAN_POINT('Ctrl Pts',(-13.9197595264191,-15.5,8.48699999999996));
#33335=CARTESIAN_POINT('Ctrl Pts',(-13.9197595264191,-14.5876477371938,
8.44533333333329));
#33336=CARTESIAN_POINT('Ctrl Pts',(-14.7098797632095,-14.1314716057907,
8.40366666666663));
#33337=CARTESIAN_POINT('Ctrl Pts',(-15.5,-13.6752954743876,8.36199999999996));
#33338=CARTESIAN_POINT('Ctrl Pts',(-16.2901202367904,-14.1314716057907,
8.32033333333329));
#33339=CARTESIAN_POINT('Ctrl Pts',(-17.0802404735808,-14.5876477371938,
8.27866666666663));
#33340=CARTESIAN_POINT('Ctrl Pts',(-17.0802404735808,-15.5000000000001,
8.23699999999996));
#33341=CARTESIAN_POINT('Ctrl Pts',(-17.0802404735808,-16.4123522628063,
8.19533333333329));
#33342=CARTESIAN_POINT('Ctrl Pts',(-16.2901202367904,-16.8685283942094,
8.15366666666663));
#33343=CARTESIAN_POINT('Ctrl Pts',(-15.4999999999999,-17.3247045256125,
8.11199999999996));
#33344=CARTESIAN_POINT('Ctrl Pts',(-14.7098797632095,-16.8685283942094,
8.07033333333329));
#33345=CARTESIAN_POINT('Ctrl Pts',(-13.9197595264191,-16.4123522628063,
8.02866666666662));
#33346=CARTESIAN_POINT('Ctrl Pts',(-13.9197595264191,-15.5,7.98699999999996));
#33347=CARTESIAN_POINT('Ctrl Pts',(-13.9197595264191,-14.5876477371938,
7.94533333333329));
#33348=CARTESIAN_POINT('Ctrl Pts',(-14.7098797632095,-14.1314716057907,
7.90366666666662));
#33349=CARTESIAN_POINT('Ctrl Pts',(-15.5,-13.6752954743876,7.86199999999995));
#33350=CARTESIAN_POINT('Ctrl Pts',(-16.2901202367904,-14.1314716057907,
7.82033333333329));
#33351=CARTESIAN_POINT('Ctrl Pts',(-17.0802404735808,-14.5876477371938,
7.77866666666662));
#33352=CARTESIAN_POINT('Ctrl Pts',(-17.0802404735808,-15.5000000000001,
7.73699999999995));
#33353=CARTESIAN_POINT('Ctrl Pts',(-17.0802404735808,-16.4123522628063,
7.69533333333329));
#33354=CARTESIAN_POINT('Ctrl Pts',(-16.2901202367904,-16.8685283942094,
7.65366666666662));
#33355=CARTESIAN_POINT('Ctrl Pts',(-15.4999999999999,-17.3247045256125,
7.61199999999995));
#33356=CARTESIAN_POINT('Ctrl Pts',(-14.7098797632095,-16.8685283942094,
7.57033333333328));
#33357=CARTESIAN_POINT('Ctrl Pts',(-13.9197595264191,-16.4123522628063,
7.52866666666662));
#33358=CARTESIAN_POINT('Ctrl Pts',(-13.9197595264191,-15.5,7.48699999999995));
#33359=CARTESIAN_POINT('Ctrl Pts',(-13.9197595264191,-14.5876477371938,
7.44533333333328));
#33360=CARTESIAN_POINT('Ctrl Pts',(-14.7098797632095,-14.1314716057907,
7.40366666666661));
#33361=CARTESIAN_POINT('Ctrl Pts',(-15.5,-13.6752954743876,7.36199999999995));
#33362=CARTESIAN_POINT('Ctrl Pts',(-16.2901202367904,-14.1314716057907,
7.32033333333328));
#33363=CARTESIAN_POINT('Ctrl Pts',(-17.0802404735808,-14.5876477371938,
7.27866666666661));
#33364=CARTESIAN_POINT('Ctrl Pts',(-17.0802404735808,-15.5000000000001,
7.23699999999995));
#33365=CARTESIAN_POINT('Ctrl Pts',(-17.0802404735808,-16.4123522628063,
7.19533333333328));
#33366=CARTESIAN_POINT('Ctrl Pts',(-16.2901202367904,-16.8685283942094,
7.15366666666661));
#33367=CARTESIAN_POINT('Ctrl Pts',(-15.4999999999999,-17.3247045256125,
7.11199999999994));
#33368=CARTESIAN_POINT('Ctrl Pts',(-14.7098797632095,-16.8685283942094,
7.07033333333328));
#33369=CARTESIAN_POINT('Ctrl Pts',(-13.9197595264191,-16.4123522628063,
7.02866666666661));
#33370=CARTESIAN_POINT('Ctrl Pts',(-13.9197595264191,-15.5,6.98699999999994));
#33371=CARTESIAN_POINT('Ctrl Pts',(-13.9197595264191,-14.5876477371938,
6.94533333333327));
#33372=CARTESIAN_POINT('Ctrl Pts',(-14.7098797632095,-14.1314716057907,
6.90366666666661));
#33373=CARTESIAN_POINT('Ctrl Pts',(-15.5,-13.6752954743876,6.86199999999994));
#33374=CARTESIAN_POINT('Ctrl Pts',(-16.2901202367904,-14.1314716057907,
6.82033333333327));
#33375=CARTESIAN_POINT('Ctrl Pts',(-17.0802404735808,-14.5876477371938,
6.77866666666661));
#33376=CARTESIAN_POINT('Ctrl Pts',(-17.0802404735808,-15.5000000000001,
6.73699999999994));
#33377=CARTESIAN_POINT('Ctrl Pts',(-17.0802404735808,-16.4123522628063,
6.69533333333327));
#33378=CARTESIAN_POINT('Ctrl Pts',(-16.2901202367904,-16.8685283942094,
6.65366666666661));
#33379=CARTESIAN_POINT('Ctrl Pts',(-15.4999999999999,-17.3247045256125,
6.61199999999994));
#33380=CARTESIAN_POINT('Ctrl Pts',(-14.7098797632095,-16.8685283942094,
6.57033333333327));
#33381=CARTESIAN_POINT('Ctrl Pts',(-13.9197595264191,-16.4123522628063,
6.5286666666666));
#33382=CARTESIAN_POINT('Ctrl Pts',(-13.9197595264191,-15.5,6.48699999999994));
#33383=CARTESIAN_POINT('Ctrl Pts',(-13.9197595264191,-14.5876477371938,
6.44533333333327));
#33384=CARTESIAN_POINT('Ctrl Pts',(-14.7098797632095,-14.1314716057907,
6.4036666666666));
#33385=CARTESIAN_POINT('Ctrl Pts',(-15.5,-13.6752954743876,6.36199999999993));
#33386=CARTESIAN_POINT('Ctrl Pts',(-16.2901202367904,-14.1314716057907,
6.32033333333327));
#33387=CARTESIAN_POINT('Ctrl Pts',(-17.0802404735808,-14.5876477371938,
6.2786666666666));
#33388=CARTESIAN_POINT('Ctrl Pts',(-17.0802404735808,-15.5000000000001,
6.23699999999993));
#33389=CARTESIAN_POINT('Ctrl Pts',(-17.0802404735808,-16.4123522628063,
6.19533333333326));
#33390=CARTESIAN_POINT('Ctrl Pts',(-16.2901202367904,-16.8685283942094,
6.1536666666666));
#33391=CARTESIAN_POINT('Ctrl Pts',(-15.4999999999999,-17.3247045256125,
6.11199999999993));
#33392=CARTESIAN_POINT('Ctrl Pts',(-14.7098797632095,-16.8685283942094,
6.07033333333326));
#33393=CARTESIAN_POINT('Ctrl Pts',(-13.9197595264191,-16.4123522628063,
6.0286666666666));
#33394=CARTESIAN_POINT('Ctrl Pts',(-13.9197595264191,-15.5,5.98699999999993));
#33395=CARTESIAN_POINT('Ctrl Pts',(-13.9197595264191,-14.5876477371938,
5.94533333333326));
#33396=CARTESIAN_POINT('Ctrl Pts',(-14.7098797632095,-14.1314716057907,
5.9036666666666));
#33397=CARTESIAN_POINT('Ctrl Pts',(-15.5,-13.6752954743876,5.86199999999993));
#33398=CARTESIAN_POINT('Ctrl Pts',(-16.2901202367904,-14.1314716057907,
5.82033333333326));
#33399=CARTESIAN_POINT('Ctrl Pts',(-17.0802404735808,-14.5876477371938,
5.77866666666659));
#33400=CARTESIAN_POINT('Ctrl Pts',(-17.0802404735808,-15.5000000000001,
5.73699999999993));
#33401=CARTESIAN_POINT('Ctrl Pts',(-17.0802404735808,-16.4123522628063,
5.69533333333326));
#33402=CARTESIAN_POINT('Ctrl Pts',(-16.2901202367904,-16.8685283942094,
5.65366666666659));
#33403=CARTESIAN_POINT('Ctrl Pts',(-15.4999999999999,-17.3247045256125,
5.61199999999992));
#33404=CARTESIAN_POINT('Ctrl Pts',(-14.7098797632095,-16.8685283942094,
5.57033333333326));
#33405=CARTESIAN_POINT('Ctrl Pts',(-13.9197595264191,-16.4123522628063,
5.52866666666659));
#33406=CARTESIAN_POINT('Ctrl Pts',(-13.9197595264191,-15.5,5.48699999999992));
#33407=CARTESIAN_POINT('Ctrl Pts',(-13.9197595264191,-14.5876477371938,
5.44533333333326));
#33408=CARTESIAN_POINT('Ctrl Pts',(-14.7098797632095,-14.1314716057907,
5.40366666666659));
#33409=CARTESIAN_POINT('Ctrl Pts',(-15.5,-13.6752954743876,5.36199999999992));
#33410=CARTESIAN_POINT('Ctrl Pts',(-16.2901202367904,-14.1314716057907,
5.32033333333325));
#33411=CARTESIAN_POINT('Ctrl Pts',(-17.0802404735808,-14.5876477371938,
5.27866666666659));
#33412=CARTESIAN_POINT('Ctrl Pts',(-17.0802404735808,-15.5000000000001,
5.23699999999992));
#33413=CARTESIAN_POINT('Ctrl Pts',(-17.0802404735808,-16.4123522628063,
5.19533333333325));
#33414=CARTESIAN_POINT('Ctrl Pts',(-16.2901202367904,-16.8685283942094,
5.15366666666658));
#33415=CARTESIAN_POINT('Ctrl Pts',(-15.4999999999999,-17.3247045256125,
5.11199999999992));
#33416=CARTESIAN_POINT('Ctrl Pts',(-14.7098797632095,-16.8685283942094,
5.07033333333325));
#33417=CARTESIAN_POINT('Ctrl Pts',(-13.9197595264191,-16.4123522628063,
5.02866666666658));
#33418=CARTESIAN_POINT('Ctrl Pts',(-13.9197595264191,-15.5,4.98699999999992));
#33419=CARTESIAN_POINT('Ctrl Pts',(-13.9197595264191,-14.5876477371938,
4.94533333333325));
#33420=CARTESIAN_POINT('Ctrl Pts',(-14.7098797632095,-14.1314716057907,
4.90366666666658));
#33421=CARTESIAN_POINT('Ctrl Pts',(-15.5,-13.6752954743876,4.86199999999991));
#33422=CARTESIAN_POINT('Ctrl Pts',(-16.2901202367904,-14.1314716057907,
4.82033333333325));
#33423=CARTESIAN_POINT('Ctrl Pts',(-17.0802404735808,-14.5876477371938,
4.77866666666658));
#33424=CARTESIAN_POINT('Ctrl Pts',(-17.0802404735808,-15.5000000000001,
4.73699999999991));
#33425=CARTESIAN_POINT('Ctrl Pts',(-17.0802404735808,-16.4123522628063,
4.69533333333325));
#33426=CARTESIAN_POINT('Ctrl Pts',(-16.2901202367904,-16.8685283942094,
4.65366666666658));
#33427=CARTESIAN_POINT('Ctrl Pts',(-15.4999999999999,-17.3247045256125,
4.61199999999991));
#33428=CARTESIAN_POINT('Ctrl Pts',(-14.7098797632095,-16.8685283942094,
4.57033333333324));
#33429=CARTESIAN_POINT('Ctrl Pts',(-13.9197595264191,-16.4123522628063,
4.52866666666658));
#33430=CARTESIAN_POINT('Ctrl Pts',(-13.9197595264191,-15.5,4.48699999999991));
#33431=CARTESIAN_POINT('Ctrl Pts',(-13.9197595264191,-14.5876477371938,
4.44533333333324));
#33432=CARTESIAN_POINT('Ctrl Pts',(-14.7098797632095,-14.1314716057907,
4.40366666666658));
#33433=CARTESIAN_POINT('Ctrl Pts',(-15.5,-13.6752954743876,4.36199999999991));
#33434=CARTESIAN_POINT('Ctrl Pts',(-16.2901202367904,-14.1314716057907,
4.32033333333324));
#33435=CARTESIAN_POINT('Ctrl Pts',(-17.0802404735808,-14.5876477371938,
4.27866666666657));
#33436=CARTESIAN_POINT('Ctrl Pts',(-17.0802404735808,-15.5000000000001,
4.23699999999991));
#33437=CARTESIAN_POINT('Ctrl Pts',(-17.0802404735808,-16.4123522628063,
4.19533333333324));
#33438=CARTESIAN_POINT('Ctrl Pts',(-16.2901202367904,-16.8685283942094,
4.15366666666657));
#33439=CARTESIAN_POINT('Ctrl Pts',(-15.4999999999999,-17.3247045256125,
4.1119999999999));
#33440=CARTESIAN_POINT('Ctrl Pts',(-14.7098797632095,-16.8685283942094,
4.07033333333324));
#33441=CARTESIAN_POINT('Ctrl Pts',(-13.9197595264191,-16.4123522628063,
4.02866666666657));
#33442=CARTESIAN_POINT('Ctrl Pts',(-13.9197595264191,-15.5,3.9869999999999));
#33443=CARTESIAN_POINT('Ctrl Pts',(-13.9197595264191,-14.5876477371938,
3.94533333333323));
#33444=CARTESIAN_POINT('Ctrl Pts',(-14.7098797632095,-14.1314716057907,
3.90366666666657));
#33445=CARTESIAN_POINT('Ctrl Pts',(-15.5,-13.6752954743876,3.8619999999999));
#33446=CARTESIAN_POINT('Ctrl Pts',(-16.2901202367904,-14.1314716057907,
3.82033333333323));
#33447=CARTESIAN_POINT('Ctrl Pts',(-17.0802404735808,-14.5876477371938,
3.77866666666657));
#33448=CARTESIAN_POINT('Ctrl Pts',(-17.0802404735808,-15.5000000000001,
3.7369999999999));
#33449=CARTESIAN_POINT('Ctrl Pts',(-17.0802404735808,-16.4123522628063,
3.69533333333323));
#33450=CARTESIAN_POINT('Ctrl Pts',(-16.2901202367904,-16.8685283942094,
3.65366666666656));
#33451=CARTESIAN_POINT('Ctrl Pts',(-15.4999999999999,-17.3247045256125,
3.6119999999999));
#33452=CARTESIAN_POINT('Ctrl Pts',(-14.7098797632095,-16.8685283942094,
3.57033333333323));
#33453=CARTESIAN_POINT('Ctrl Pts',(-13.9197595264191,-16.4123522628063,
3.52866666666656));
#33454=CARTESIAN_POINT('Ctrl Pts',(-13.9197595264191,-15.5,3.4869999999999));
#33455=CARTESIAN_POINT('Ctrl Pts',(-13.9197595264191,-14.5876477371938,
3.44533333333323));
#33456=CARTESIAN_POINT('Ctrl Pts',(-14.7098797632095,-14.1314716057907,
3.40366666666656));
#33457=CARTESIAN_POINT('Ctrl Pts',(-15.5,-13.6752954743876,3.36199999999989));
#33458=CARTESIAN_POINT('Ctrl Pts',(-16.2901202367904,-14.1314716057907,
3.32033333333323));
#33459=CARTESIAN_POINT('Ctrl Pts',(-17.0802404735808,-14.5876477371938,
3.27866666666656));
#33460=CARTESIAN_POINT('Ctrl Pts',(-17.0802404735808,-15.5000000000001,
3.23699999999989));
#33461=CARTESIAN_POINT('Ctrl Pts',(-17.0802404735808,-16.4123522628063,
3.19533333333323));
#33462=CARTESIAN_POINT('Ctrl Pts',(-16.2901202367904,-16.8685283942094,
3.15366666666656));
#33463=CARTESIAN_POINT('Ctrl Pts',(-15.4999999999999,-17.3247045256125,
3.11199999999989));
#33464=CARTESIAN_POINT('Ctrl Pts',(-14.7098797632095,-16.8685283942094,
3.07033333333322));
#33465=CARTESIAN_POINT('Ctrl Pts',(-13.9197595264191,-16.4123522628063,
3.02866666666656));
#33466=CARTESIAN_POINT('Ctrl Pts',(-13.9197595264191,-15.5,2.98699999999989));
#33467=CARTESIAN_POINT('Ctrl Pts',(-13.9197595264191,-14.5876477371938,
2.94533333333322));
#33468=CARTESIAN_POINT('Ctrl Pts',(-14.7098797632095,-14.1314716057907,
2.90366666666656));
#33469=CARTESIAN_POINT('Ctrl Pts',(-15.5,-13.6752954743876,2.86199999999989));
#33470=CARTESIAN_POINT('Ctrl Pts',(-16.2901202367904,-14.1314716057907,
2.82033333333322));
#33471=CARTESIAN_POINT('Ctrl Pts',(-17.0802404735808,-14.5876477371938,
2.77866666666655));
#33472=CARTESIAN_POINT('Ctrl Pts',(-17.0802404735808,-15.5000000000001,
2.73699999999989));
#33473=CARTESIAN_POINT('Ctrl Pts',(-17.0802404735808,-16.4123522628063,
2.69533333333322));
#33474=CARTESIAN_POINT('Ctrl Pts',(-16.2901202367904,-16.8685283942094,
2.65366666666655));
#33475=CARTESIAN_POINT('Ctrl Pts',(-15.4999999999999,-17.3247045256125,
2.61199999999988));
#33476=CARTESIAN_POINT('Ctrl Pts',(-14.7098797632095,-16.8685283942094,
2.57033333333322));
#33477=CARTESIAN_POINT('Ctrl Pts',(-13.9197595264191,-16.4123522628063,
2.52866666666655));
#33478=CARTESIAN_POINT('Ctrl Pts',(-13.9197595264191,-15.5,2.48699999999988));
#33479=CARTESIAN_POINT('Ctrl Pts',(-13.9197595264191,-14.5876477371938,
2.44533333333321));
#33480=CARTESIAN_POINT('Ctrl Pts',(-14.7098797632095,-14.1314716057907,
2.40366666666655));
#33481=CARTESIAN_POINT('Ctrl Pts',(-15.5,-13.6752954743876,2.36199999999988));
#33482=CARTESIAN_POINT('Ctrl Pts',(-16.2901202367904,-14.1314716057907,
2.32033333333321));
#33483=CARTESIAN_POINT('Ctrl Pts',(-17.0802404735808,-14.5876477371938,
2.27866666666655));
#33484=CARTESIAN_POINT('Ctrl Pts',(-17.0802404735808,-15.5000000000001,
2.23699999999988));
#33485=CARTESIAN_POINT('Ctrl Pts',(-17.0802404735808,-16.4123522628063,
2.19533333333321));
#33486=CARTESIAN_POINT('Ctrl Pts',(-16.2901202367904,-16.8685283942094,
2.15366666666655));
#33487=CARTESIAN_POINT('Ctrl Pts',(-15.4999999999999,-17.3247045256125,
2.11199999999988));
#33488=CARTESIAN_POINT('Ctrl Pts',(-14.7098797632095,-16.8685283942094,
2.07033333333321));
#33489=CARTESIAN_POINT('Ctrl Pts',(-13.9197595264191,-16.4123522628063,
2.02866666666654));
#33490=CARTESIAN_POINT('Ctrl Pts',(-13.9197595264191,-15.5,1.98699999999988));
#33491=CARTESIAN_POINT('Ctrl Pts',(-13.9197595264191,-14.5876477371938,
1.94533333333321));
#33492=CARTESIAN_POINT('Ctrl Pts',(-14.7098797632095,-14.1314716057907,
1.90366666666654));
#33493=CARTESIAN_POINT('Ctrl Pts',(-15.5,-13.6752954743876,1.86199999999987));
#33494=CARTESIAN_POINT('Ctrl Pts',(-16.2901202367904,-14.1314716057907,
1.82033333333321));
#33495=CARTESIAN_POINT('Ctrl Pts',(-17.0802404735808,-14.5876477371938,
1.77866666666654));
#33496=CARTESIAN_POINT('Ctrl Pts',(-17.0802404735808,-15.5000000000001,
1.73699999999987));
#33497=CARTESIAN_POINT('Ctrl Pts',(-17.0802404735808,-16.4123522628063,
1.6953333333332));
#33498=CARTESIAN_POINT('Ctrl Pts',(-16.2901202367904,-16.8685283942094,
1.65366666666654));
#33499=CARTESIAN_POINT('Ctrl Pts',(-15.4999999999999,-17.3247045256125,
1.61199999999987));
#33500=CARTESIAN_POINT('Ctrl Pts',(-14.7098797632095,-16.8685283942094,
1.5703333333332));
#33501=CARTESIAN_POINT('Ctrl Pts',(-13.9197595264191,-16.4123522628063,
1.52866666666654));
#33502=CARTESIAN_POINT('Ctrl Pts',(-13.9197595264191,-15.5,1.48699999999987));
#33503=CARTESIAN_POINT('Ctrl Pts',(-13.9197595264191,-14.5876477371938,
1.4453333333332));
#33504=CARTESIAN_POINT('Ctrl Pts',(-14.7098797632095,-14.1314716057907,
1.40366666666653));
#33505=CARTESIAN_POINT('Ctrl Pts',(-15.5,-13.6752954743876,1.36199999999987));
#33506=CARTESIAN_POINT('Ctrl Pts',(-16.2901202367904,-14.1314716057907,
1.3203333333332));
#33507=CARTESIAN_POINT('Ctrl Pts',(-17.0802404735808,-14.5876477371938,
1.27866666666653));
#33508=CARTESIAN_POINT('Ctrl Pts',(-17.0802404735808,-15.5000000000001,
1.23699999999987));
#33509=CARTESIAN_POINT('Ctrl Pts',(-17.0802404735808,-16.4123522628063,
1.1953333333332));
#33510=CARTESIAN_POINT('Ctrl Pts',(-16.2901202367904,-16.8685283942094,
1.15366666666653));
#33511=CARTESIAN_POINT('Ctrl Pts',(-15.4999999999999,-17.3247045256125,
1.11199999999986));
#33512=CARTESIAN_POINT('Ctrl Pts',(-14.7098797632095,-16.8685283942094,
1.0703333333332));
#33513=CARTESIAN_POINT('Ctrl Pts',(-13.9197595264191,-16.4123522628063,
1.02866666666653));
#33514=CARTESIAN_POINT('Ctrl Pts',(-13.9197595264191,-15.5,0.986999999999863));
#33515=CARTESIAN_POINT('Ctrl Pts',(-13.9197595264191,-14.5876477371938,
0.945333333333196));
#33516=CARTESIAN_POINT('Ctrl Pts',(-14.7098797632095,-14.1314716057907,
0.903666666666529));
#33517=CARTESIAN_POINT('Ctrl Pts',(-15.5,-13.6752954743876,0.861999999999861));
#33518=CARTESIAN_POINT('Ctrl Pts',(-16.2901202367904,-14.1314716057907,
0.820333333333194));
#33519=CARTESIAN_POINT('Ctrl Pts',(-17.0802404735808,-14.5876477371938,
0.778666666666527));
#33520=CARTESIAN_POINT('Ctrl Pts',(-17.0802404735808,-15.5000000000001,
0.736999999999859));
#33521=CARTESIAN_POINT('Ctrl Pts',(-17.0802404735808,-16.4123522628063,
0.695333333333192));
#33522=CARTESIAN_POINT('Ctrl Pts',(-16.2901202367904,-16.8685283942094,
0.653666666666525));
#33523=CARTESIAN_POINT('Ctrl Pts',(-15.4999999999999,-17.3247045256125,
0.611999999999858));
#33524=CARTESIAN_POINT('Ctrl Pts',(-14.7098797632095,-16.8685283942094,
0.57033333333319));
#33525=CARTESIAN_POINT('Ctrl Pts',(-13.9197595264191,-16.4123522628063,
0.528666666666523));
#33526=CARTESIAN_POINT('Ctrl Pts',(-13.9197595264191,-15.5,0.486999999999856));
#33527=CARTESIAN_POINT('Ctrl Pts',(-13.9197595264191,-14.5876477371938,
0.445333333333188));
#33528=CARTESIAN_POINT('Ctrl Pts',(-14.7098797632095,-14.1314716057907,
0.403666666666521));
#33529=CARTESIAN_POINT('Ctrl Pts',(-15.5,-13.6752954743876,0.361999999999854));
#33530=CARTESIAN_POINT('Ctrl Pts',(-16.2901202367904,-14.1314716057907,
0.320333333333186));
#33531=CARTESIAN_POINT('Ctrl Pts',(-17.0802404735808,-14.5876477371938,
0.278666666666519));
#33532=CARTESIAN_POINT('Ctrl Pts',(-17.0802404735808,-15.5000000000001,
0.236999999999852));
#33533=CARTESIAN_POINT('Ctrl Pts',(-17.0802404735808,-16.4123522628063,
0.195333333333185));
#33534=CARTESIAN_POINT('Ctrl Pts',(-16.2901202367904,-16.8685283942094,
0.153666666666517));
#33535=CARTESIAN_POINT('Ctrl Pts',(-15.4999999999999,-17.3247045256125,
0.11199999999985));
#33536=CARTESIAN_POINT('Ctrl Pts',(-14.7098797632095,-16.8685283942094,
0.0703333333331828));
#33537=CARTESIAN_POINT('Ctrl Pts',(-13.9197595264191,-16.4123522628063,
0.0286666666665155));
#33538=CARTESIAN_POINT('Ctrl Pts',(-13.9197595264191,-15.5,-0.0130000000001518));
#33539=CARTESIAN_POINT('Ctrl Pts',(-13.9197595264191,-14.5876477371938,
-0.0546666666668173));
#33540=CARTESIAN_POINT('Ctrl Pts',(-14.7098797632095,-14.1314716057907,
-0.0963333333334846));
#33541=CARTESIAN_POINT('Ctrl Pts',(-15.5,-13.6752954743876,-0.138000000000152));
#33542=CARTESIAN_POINT('Ctrl Pts',(-16.2901202367904,-14.1314716057907,
-0.179666666666819));
#33543=CARTESIAN_POINT('Ctrl Pts',(-17.0802404735808,-14.5876477371938,
-0.221333333333486));
#33544=CARTESIAN_POINT('Ctrl Pts',(-17.0802404735808,-15.5000000000001,
-0.263000000000154));
#33545=CARTESIAN_POINT('Ctrl Pts',(-17.0802404735808,-16.4123522628063,
-0.304666666666821));
#33546=CARTESIAN_POINT('Ctrl Pts',(-16.2901202367904,-16.8685283942094,
-0.346333333333488));
#33547=CARTESIAN_POINT('Ctrl Pts',(-15.4999999999999,-17.3247045256125,
-0.388000000000156));
#33548=CARTESIAN_POINT('Ctrl Pts',(-14.7098797632095,-16.8685283942094,
-0.429666666666823));
#33549=CARTESIAN_POINT('Ctrl Pts',(-13.9197595264191,-16.4123522628063,
-0.47133333333349));
#33550=CARTESIAN_POINT('Ctrl Pts',(-13.9197595264191,-15.5,-0.513000000000157));
#33551=CARTESIAN_POINT('Ctrl Pts',(-13.9197595264191,-14.5876477371938,
-0.554666666666825));
#33552=CARTESIAN_POINT('Ctrl Pts',(-14.7098797632095,-14.1314716057907,
-0.596333333333492));
#33553=CARTESIAN_POINT('Ctrl Pts',(-15.5,-13.6752954743876,-0.638000000000159));
#33554=CARTESIAN_POINT('Ctrl Pts',(-16.2901202367904,-14.1314716057907,
-0.679666666666827));
#33555=CARTESIAN_POINT('Ctrl Pts',(-17.0802404735808,-14.5876477371938,
-0.721333333333494));
#33556=CARTESIAN_POINT('Ctrl Pts',(-17.0802404735808,-15.5000000000001,
-0.763000000000161));
#33557=CARTESIAN_POINT('Ctrl Pts',(-17.0802404735808,-16.4123522628063,
-0.804666666666829));
#33558=CARTESIAN_POINT('Ctrl Pts',(-16.2901202367904,-16.8685283942094,
-0.846333333333496));
#33559=CARTESIAN_POINT('Ctrl Pts',(-15.4999999999999,-17.3247045256125,
-0.888000000000163));
#33560=CARTESIAN_POINT('Ctrl Pts',(-14.7098797632095,-16.8685283942094,
-0.92966666666683));
#33561=CARTESIAN_POINT('Ctrl Pts',(-13.9197595264191,-16.4123522628063,
-0.971333333333498));
#33562=CARTESIAN_POINT('Ctrl Pts',(-13.9197595264191,-15.5,-1.01300000000016));
#33563=CARTESIAN_POINT('Ctrl Pts',(-13.9197595264191,-14.5876477371938,
-1.05466666666683));
#33564=CARTESIAN_POINT('Ctrl Pts',(-14.7098797632095,-14.1314716057907,
-1.0963333333335));
#33565=CARTESIAN_POINT('Ctrl Pts',(-15.5,-13.6752954743876,-1.13800000000017));
#33566=CARTESIAN_POINT('Ctrl Pts',(-16.2901202367904,-14.1314716057907,
-1.17966666666683));
#33567=CARTESIAN_POINT('Ctrl Pts',(-17.0802404735808,-14.5876477371938,
-1.2213333333335));
#33568=CARTESIAN_POINT('Ctrl Pts',(-17.0802404735808,-15.5000000000001,
-1.26300000000017));
#33569=CARTESIAN_POINT('Ctrl Pts',(-17.0802404735808,-16.4123522628063,
-1.30466666666683));
#33570=CARTESIAN_POINT('Ctrl Pts',(-16.2901202367904,-16.8685283942094,
-1.3463333333335));
#33571=CARTESIAN_POINT('Ctrl Pts',(-15.4999999999999,-17.3247045256125,
-1.38800000000017));
#33572=CARTESIAN_POINT('Ctrl Pts',(-14.7098797632095,-16.8685283942094,
-1.42966666666684));
#33573=CARTESIAN_POINT('Ctrl Pts',(-13.9197595264191,-16.4123522628063,
-1.4713333333335));
#33574=CARTESIAN_POINT('Ctrl Pts',(-13.9197595264191,-15.5,-1.51300000000017));
#33575=CARTESIAN_POINT('Ctrl Pts',(-13.9197595264191,-14.5876477371938,
-1.55466666666684));
#33576=CARTESIAN_POINT('Ctrl Pts',(-14.7098797632095,-14.1314716057907,
-1.59633333333351));
#33577=CARTESIAN_POINT('Ctrl Pts',(-15.5,-13.6752954743876,-1.63800000000017));
#33578=CARTESIAN_POINT('Ctrl Pts',(-16.2901202367904,-14.1314716057907,
-1.67966666666684));
#33579=CARTESIAN_POINT('Ctrl Pts',(-17.0802404735808,-14.5876477371938,
-1.72133333333351));
#33580=CARTESIAN_POINT('Ctrl Pts',(-17.0802404735808,-15.5000000000001,
-1.76300000000017));
#33581=CARTESIAN_POINT('Ctrl Pts',(-17.0802404735808,-16.4123522628063,
-1.80466666666684));
#33582=CARTESIAN_POINT('Ctrl Pts',(-16.2901202367904,-16.8685283942094,
-1.84633333333351));
#33583=CARTESIAN_POINT('Ctrl Pts',(-15.4999999999999,-17.3247045256125,
-1.88800000000018));
#33584=CARTESIAN_POINT('Ctrl Pts',(-14.7098797632095,-16.8685283942094,
-1.92966666666684));
#33585=CARTESIAN_POINT('Ctrl Pts',(-14.4189900731898,-16.7005831533721,
-1.94500661517905));
#33586=CARTESIAN_POINT('Ctrl Pts',(-14.2215527726061,-16.42883402237,-1.96262314816781));
#33587=CARTESIAN_POINT('Origin',(-14.0080754615185,-16.5839252605847,-2.17746715486548));
#33588=CARTESIAN_POINT('',(-14.2215498957103,-16.4288300625789,-2.02512301642217));
#33589=CARTESIAN_POINT('Ctrl Pts',(-17.0802404735808,-15.5000000000001,
11.2370201234482));
#33590=CARTESIAN_POINT('Ctrl Pts',(-17.0802404735808,-16.4123522628063,
11.1953534567815));
#33591=CARTESIAN_POINT('Ctrl Pts',(-16.2901202367904,-16.8685283942094,
11.1536867901149));
#33592=CARTESIAN_POINT('Ctrl Pts',(-15.4999999999999,-17.3247045256125,
11.1120201234482));
#33593=CARTESIAN_POINT('Ctrl Pts',(-14.7098797632095,-16.8685283942094,
11.0703534567815));
#33594=CARTESIAN_POINT('Ctrl Pts',(-13.9197595264191,-16.4123522628063,
11.0286867901149));
#33595=CARTESIAN_POINT('Ctrl Pts',(-13.9197595264191,-15.5,10.9870201234482));
#33596=CARTESIAN_POINT('Ctrl Pts',(-13.9197595264191,-14.5876477371938,
10.9453534567815));
#33597=CARTESIAN_POINT('Ctrl Pts',(-14.7098797632095,-14.1314716057907,
10.9036867901149));
#33598=CARTESIAN_POINT('Ctrl Pts',(-15.5,-13.6752954743876,10.8620201234482));
#33599=CARTESIAN_POINT('Ctrl Pts',(-16.2901202367904,-14.1314716057907,
10.8203534567815));
#33600=CARTESIAN_POINT('Ctrl Pts',(-17.0802404735808,-14.5876477371938,
10.7786867901149));
#33601=CARTESIAN_POINT('Ctrl Pts',(-17.0802404735808,-15.5000000000001,
10.7370201234482));
#33602=CARTESIAN_POINT('Ctrl Pts',(-17.0802404735808,-16.4123522628063,
10.6953534567815));
#33603=CARTESIAN_POINT('Ctrl Pts',(-16.2901202367904,-16.8685283942094,
10.6536867901149));
#33604=CARTESIAN_POINT('Ctrl Pts',(-15.4999999999999,-17.3247045256125,
10.6120201234482));
#33605=CARTESIAN_POINT('Ctrl Pts',(-14.7098797632095,-16.8685283942094,
10.5703534567815));
#33606=CARTESIAN_POINT('Ctrl Pts',(-13.9197595264191,-16.4123522628063,
10.5286867901149));
#33607=CARTESIAN_POINT('Ctrl Pts',(-13.9197595264191,-15.5,10.4870201234482));
#33608=CARTESIAN_POINT('Ctrl Pts',(-13.9197595264191,-14.5876477371938,
10.4453534567815));
#33609=CARTESIAN_POINT('Ctrl Pts',(-14.7098797632095,-14.1314716057907,
10.4036867901149));
#33610=CARTESIAN_POINT('Ctrl Pts',(-15.5,-13.6752954743876,10.3620201234482));
#33611=CARTESIAN_POINT('Ctrl Pts',(-16.2901202367904,-14.1314716057907,
10.3203534567815));
#33612=CARTESIAN_POINT('Ctrl Pts',(-17.0802404735808,-14.5876477371938,
10.2786867901149));
#33613=CARTESIAN_POINT('Ctrl Pts',(-17.0802404735808,-15.5000000000001,
10.2370201234482));
#33614=CARTESIAN_POINT('Ctrl Pts',(-17.0802404735808,-16.4123522628063,
10.1953534567815));
#33615=CARTESIAN_POINT('Ctrl Pts',(-16.2901202367904,-16.8685283942094,
10.1536867901149));
#33616=CARTESIAN_POINT('Ctrl Pts',(-15.4999999999999,-17.3247045256125,
10.1120201234482));
#33617=CARTESIAN_POINT('Ctrl Pts',(-14.7098797632095,-16.8685283942094,
10.0703534567815));
#33618=CARTESIAN_POINT('Ctrl Pts',(-13.9197595264191,-16.4123522628063,
10.0286867901149));
#33619=CARTESIAN_POINT('Ctrl Pts',(-13.9197595264191,-15.5,9.98702012344819));
#33620=CARTESIAN_POINT('Ctrl Pts',(-13.9197595264191,-14.5876477371938,
9.94535345678152));
#33621=CARTESIAN_POINT('Ctrl Pts',(-14.7098797632095,-14.1314716057907,
9.90368679011485));
#33622=CARTESIAN_POINT('Ctrl Pts',(-15.5,-13.6752954743876,9.86202012344818));
#33623=CARTESIAN_POINT('Ctrl Pts',(-16.2901202367904,-14.1314716057907,
9.82035345678151));
#33624=CARTESIAN_POINT('Ctrl Pts',(-17.0802404735808,-14.5876477371938,
9.77868679011485));
#33625=CARTESIAN_POINT('Ctrl Pts',(-17.0802404735808,-15.5000000000001,
9.73702012344818));
#33626=CARTESIAN_POINT('Ctrl Pts',(-17.0802404735808,-16.4123522628063,
9.69535345678152));
#33627=CARTESIAN_POINT('Ctrl Pts',(-16.2901202367904,-16.8685283942094,
9.65368679011485));
#33628=CARTESIAN_POINT('Ctrl Pts',(-15.4999999999999,-17.3247045256125,
9.61202012344818));
#33629=CARTESIAN_POINT('Ctrl Pts',(-14.7098797632095,-16.8685283942094,
9.57035345678151));
#33630=CARTESIAN_POINT('Ctrl Pts',(-13.9197595264191,-16.4123522628063,
9.52868679011484));
#33631=CARTESIAN_POINT('Ctrl Pts',(-13.9197595264191,-15.5,9.48702012344818));
#33632=CARTESIAN_POINT('Ctrl Pts',(-13.9197595264191,-14.5876477371938,
9.44535345678151));
#33633=CARTESIAN_POINT('Ctrl Pts',(-14.7098797632095,-14.1314716057907,
9.40368679011484));
#33634=CARTESIAN_POINT('Ctrl Pts',(-15.5,-13.6752954743876,9.36202012344818));
#33635=CARTESIAN_POINT('Ctrl Pts',(-16.2901202367904,-14.1314716057907,
9.32035345678151));
#33636=CARTESIAN_POINT('Ctrl Pts',(-17.0802404735808,-14.5876477371938,
9.27868679011484));
#33637=CARTESIAN_POINT('Ctrl Pts',(-17.0802404735808,-15.5000000000001,
9.23702012344818));
#33638=CARTESIAN_POINT('Ctrl Pts',(-17.0802404735808,-16.4123522628063,
9.19535345678151));
#33639=CARTESIAN_POINT('Ctrl Pts',(-16.2901202367904,-16.8685283942094,
9.15368679011484));
#33640=CARTESIAN_POINT('Ctrl Pts',(-15.4999999999999,-17.3247045256125,
9.11202012344818));
#33641=CARTESIAN_POINT('Ctrl Pts',(-14.7098797632095,-16.8685283942094,
9.07035345678151));
#33642=CARTESIAN_POINT('Ctrl Pts',(-13.9197595264191,-16.4123522628063,
9.02868679011484));
#33643=CARTESIAN_POINT('Ctrl Pts',(-13.9197595264191,-15.5,8.98702012344817));
#33644=CARTESIAN_POINT('Ctrl Pts',(-13.9197595264191,-14.5876477371938,
8.9453534567815));
#33645=CARTESIAN_POINT('Ctrl Pts',(-14.7098797632095,-14.1314716057907,
8.90368679011484));
#33646=CARTESIAN_POINT('Ctrl Pts',(-15.5,-13.6752954743876,8.86202012344817));
#33647=CARTESIAN_POINT('Ctrl Pts',(-16.2901202367904,-14.1314716057907,
8.8203534567815));
#33648=CARTESIAN_POINT('Ctrl Pts',(-17.0802404735808,-14.5876477371938,
8.77868679011484));
#33649=CARTESIAN_POINT('Ctrl Pts',(-17.0802404735808,-15.5000000000001,
8.73702012344817));
#33650=CARTESIAN_POINT('Ctrl Pts',(-17.0802404735808,-16.4123522628063,
8.6953534567815));
#33651=CARTESIAN_POINT('Ctrl Pts',(-16.2901202367904,-16.8685283942094,
8.65368679011483));
#33652=CARTESIAN_POINT('Ctrl Pts',(-15.4999999999999,-17.3247045256125,
8.61202012344817));
#33653=CARTESIAN_POINT('Ctrl Pts',(-14.7098797632095,-16.8685283942094,
8.5703534567815));
#33654=CARTESIAN_POINT('Ctrl Pts',(-13.9197595264191,-16.4123522628063,
8.52868679011483));
#33655=CARTESIAN_POINT('Ctrl Pts',(-13.9197595264191,-15.5,8.48702012344816));
#33656=CARTESIAN_POINT('Ctrl Pts',(-13.9197595264191,-14.5876477371938,
8.4453534567815));
#33657=CARTESIAN_POINT('Ctrl Pts',(-14.7098797632095,-14.1314716057907,
8.40368679011483));
#33658=CARTESIAN_POINT('Ctrl Pts',(-15.5,-13.6752954743876,8.36202012344816));
#33659=CARTESIAN_POINT('Ctrl Pts',(-16.2901202367904,-14.1314716057907,
8.3203534567815));
#33660=CARTESIAN_POINT('Ctrl Pts',(-17.0802404735808,-14.5876477371938,
8.27868679011483));
#33661=CARTESIAN_POINT('Ctrl Pts',(-17.0802404735808,-15.5000000000001,
8.23702012344816));
#33662=CARTESIAN_POINT('Ctrl Pts',(-17.0802404735808,-16.4123522628063,
8.19535345678149));
#33663=CARTESIAN_POINT('Ctrl Pts',(-16.2901202367904,-16.8685283942094,
8.15368679011483));
#33664=CARTESIAN_POINT('Ctrl Pts',(-15.4999999999999,-17.3247045256125,
8.11202012344816));
#33665=CARTESIAN_POINT('Ctrl Pts',(-14.7098797632095,-16.8685283942094,
8.07035345678149));
#33666=CARTESIAN_POINT('Ctrl Pts',(-13.9197595264191,-16.4123522628063,
8.02868679011483));
#33667=CARTESIAN_POINT('Ctrl Pts',(-13.9197595264191,-15.5,7.98702012344816));
#33668=CARTESIAN_POINT('Ctrl Pts',(-13.9197595264191,-14.5876477371938,
7.94535345678149));
#33669=CARTESIAN_POINT('Ctrl Pts',(-14.7098797632095,-14.1314716057907,
7.90368679011482));
#33670=CARTESIAN_POINT('Ctrl Pts',(-15.5,-13.6752954743876,7.86202012344816));
#33671=CARTESIAN_POINT('Ctrl Pts',(-16.2901202367904,-14.1314716057907,
7.82035345678149));
#33672=CARTESIAN_POINT('Ctrl Pts',(-17.0802404735808,-14.5876477371938,
7.77868679011482));
#33673=CARTESIAN_POINT('Ctrl Pts',(-17.0802404735808,-15.5000000000001,
7.73702012344816));
#33674=CARTESIAN_POINT('Ctrl Pts',(-17.0802404735808,-16.4123522628063,
7.69535345678149));
#33675=CARTESIAN_POINT('Ctrl Pts',(-16.2901202367904,-16.8685283942094,
7.65368679011482));
#33676=CARTESIAN_POINT('Ctrl Pts',(-15.4999999999999,-17.3247045256125,
7.61202012344815));
#33677=CARTESIAN_POINT('Ctrl Pts',(-14.7098797632095,-16.8685283942094,
7.57035345678149));
#33678=CARTESIAN_POINT('Ctrl Pts',(-13.9197595264191,-16.4123522628063,
7.52868679011482));
#33679=CARTESIAN_POINT('Ctrl Pts',(-13.9197595264191,-15.5,7.48702012344815));
#33680=CARTESIAN_POINT('Ctrl Pts',(-13.9197595264191,-14.5876477371938,
7.44535345678149));
#33681=CARTESIAN_POINT('Ctrl Pts',(-14.7098797632095,-14.1314716057907,
7.40368679011482));
#33682=CARTESIAN_POINT('Ctrl Pts',(-15.5,-13.6752954743876,7.36202012344815));
#33683=CARTESIAN_POINT('Ctrl Pts',(-16.2901202367904,-14.1314716057907,
7.32035345678148));
#33684=CARTESIAN_POINT('Ctrl Pts',(-17.0802404735808,-14.5876477371938,
7.27868679011482));
#33685=CARTESIAN_POINT('Ctrl Pts',(-17.0802404735808,-15.5000000000001,
7.23702012344815));
#33686=CARTESIAN_POINT('Ctrl Pts',(-17.0802404735808,-16.4123522628063,
7.19535345678148));
#33687=CARTESIAN_POINT('Ctrl Pts',(-16.2901202367904,-16.8685283942094,
7.15368679011481));
#33688=CARTESIAN_POINT('Ctrl Pts',(-15.4999999999999,-17.3247045256125,
7.11202012344815));
#33689=CARTESIAN_POINT('Ctrl Pts',(-14.7098797632095,-16.8685283942094,
7.07035345678148));
#33690=CARTESIAN_POINT('Ctrl Pts',(-13.9197595264191,-16.4123522628063,
7.02868679011481));
#33691=CARTESIAN_POINT('Ctrl Pts',(-13.9197595264191,-15.5,6.98702012344815));
#33692=CARTESIAN_POINT('Ctrl Pts',(-13.9197595264191,-14.5876477371938,
6.94535345678148));
#33693=CARTESIAN_POINT('Ctrl Pts',(-14.7098797632095,-14.1314716057907,
6.90368679011481));
#33694=CARTESIAN_POINT('Ctrl Pts',(-15.5,-13.6752954743876,6.86202012344814));
#33695=CARTESIAN_POINT('Ctrl Pts',(-16.2901202367904,-14.1314716057907,
6.82035345678148));
#33696=CARTESIAN_POINT('Ctrl Pts',(-17.0802404735808,-14.5876477371938,
6.77868679011481));
#33697=CARTESIAN_POINT('Ctrl Pts',(-17.0802404735808,-15.5000000000001,
6.73702012344814));
#33698=CARTESIAN_POINT('Ctrl Pts',(-17.0802404735808,-16.4123522628063,
6.69535345678147));
#33699=CARTESIAN_POINT('Ctrl Pts',(-16.2901202367904,-16.8685283942094,
6.65368679011481));
#33700=CARTESIAN_POINT('Ctrl Pts',(-15.4999999999999,-17.3247045256125,
6.61202012344814));
#33701=CARTESIAN_POINT('Ctrl Pts',(-14.7098797632095,-16.8685283942094,
6.57035345678147));
#33702=CARTESIAN_POINT('Ctrl Pts',(-13.9197595264191,-16.4123522628063,
6.52868679011481));
#33703=CARTESIAN_POINT('Ctrl Pts',(-13.9197595264191,-15.5,6.48702012344814));
#33704=CARTESIAN_POINT('Ctrl Pts',(-13.9197595264191,-14.5876477371938,
6.44535345678147));
#33705=CARTESIAN_POINT('Ctrl Pts',(-14.7098797632095,-14.1314716057907,
6.4036867901148));
#33706=CARTESIAN_POINT('Ctrl Pts',(-15.5,-13.6752954743876,6.36202012344814));
#33707=CARTESIAN_POINT('Ctrl Pts',(-16.2901202367904,-14.1314716057907,
6.32035345678147));
#33708=CARTESIAN_POINT('Ctrl Pts',(-17.0802404735808,-14.5876477371938,
6.2786867901148));
#33709=CARTESIAN_POINT('Ctrl Pts',(-17.0802404735808,-15.5000000000001,
6.23702012344813));
#33710=CARTESIAN_POINT('Ctrl Pts',(-17.0802404735808,-16.4123522628063,
6.19535345678147));
#33711=CARTESIAN_POINT('Ctrl Pts',(-16.2901202367904,-16.8685283942094,
6.1536867901148));
#33712=CARTESIAN_POINT('Ctrl Pts',(-15.4999999999999,-17.3247045256125,
6.11202012344813));
#33713=CARTESIAN_POINT('Ctrl Pts',(-14.7098797632095,-16.8685283942094,
6.07035345678146));
#33714=CARTESIAN_POINT('Ctrl Pts',(-13.9197595264191,-16.4123522628063,
6.0286867901148));
#33715=CARTESIAN_POINT('Ctrl Pts',(-13.9197595264191,-15.5,5.98702012344813));
#33716=CARTESIAN_POINT('Ctrl Pts',(-13.9197595264191,-14.5876477371938,
5.94535345678146));
#33717=CARTESIAN_POINT('Ctrl Pts',(-14.7098797632095,-14.1314716057907,
5.9036867901148));
#33718=CARTESIAN_POINT('Ctrl Pts',(-15.5,-13.6752954743876,5.86202012344813));
#33719=CARTESIAN_POINT('Ctrl Pts',(-16.2901202367904,-14.1314716057907,
5.82035345678146));
#33720=CARTESIAN_POINT('Ctrl Pts',(-17.0802404735808,-14.5876477371938,
5.77868679011479));
#33721=CARTESIAN_POINT('Ctrl Pts',(-17.0802404735808,-15.5000000000001,
5.73702012344813));
#33722=CARTESIAN_POINT('Ctrl Pts',(-17.0802404735808,-16.4123522628063,
5.69535345678146));
#33723=CARTESIAN_POINT('Ctrl Pts',(-16.2901202367904,-16.8685283942094,
5.65368679011479));
#33724=CARTESIAN_POINT('Ctrl Pts',(-15.4999999999999,-17.3247045256125,
5.61202012344813));
#33725=CARTESIAN_POINT('Ctrl Pts',(-14.7098797632095,-16.8685283942094,
5.57035345678146));
#33726=CARTESIAN_POINT('Ctrl Pts',(-13.9197595264191,-16.4123522628063,
5.52868679011479));
#33727=CARTESIAN_POINT('Ctrl Pts',(-13.9197595264191,-15.5,5.48702012344813));
#33728=CARTESIAN_POINT('Ctrl Pts',(-13.9197595264191,-14.5876477371938,
5.44535345678146));
#33729=CARTESIAN_POINT('Ctrl Pts',(-14.7098797632095,-14.1314716057907,
5.40368679011479));
#33730=CARTESIAN_POINT('Ctrl Pts',(-15.5,-13.6752954743876,5.36202012344812));
#33731=CARTESIAN_POINT('Ctrl Pts',(-16.2901202367904,-14.1314716057907,
5.32035345678146));
#33732=CARTESIAN_POINT('Ctrl Pts',(-17.0802404735808,-14.5876477371938,
5.27868679011479));
#33733=CARTESIAN_POINT('Ctrl Pts',(-17.0802404735808,-15.5000000000001,
5.23702012344812));
#33734=CARTESIAN_POINT('Ctrl Pts',(-17.0802404735808,-16.4123522628063,
5.19535345678145));
#33735=CARTESIAN_POINT('Ctrl Pts',(-16.2901202367904,-16.8685283942094,
5.15368679011479));
#33736=CARTESIAN_POINT('Ctrl Pts',(-15.4999999999999,-17.3247045256125,
5.11202012344812));
#33737=CARTESIAN_POINT('Ctrl Pts',(-14.7098797632095,-16.8685283942094,
5.07035345678145));
#33738=CARTESIAN_POINT('Ctrl Pts',(-13.9197595264191,-16.4123522628063,
5.02868679011479));
#33739=CARTESIAN_POINT('Ctrl Pts',(-13.9197595264191,-15.5,4.98702012344812));
#33740=CARTESIAN_POINT('Ctrl Pts',(-13.9197595264191,-14.5876477371938,
4.94535345678145));
#33741=CARTESIAN_POINT('Ctrl Pts',(-14.7098797632095,-14.1314716057907,
4.90368679011478));
#33742=CARTESIAN_POINT('Ctrl Pts',(-15.5,-13.6752954743876,4.86202012344812));
#33743=CARTESIAN_POINT('Ctrl Pts',(-16.2901202367904,-14.1314716057907,
4.82035345678145));
#33744=CARTESIAN_POINT('Ctrl Pts',(-17.0802404735808,-14.5876477371938,
4.77868679011478));
#33745=CARTESIAN_POINT('Ctrl Pts',(-17.0802404735808,-15.5000000000001,
4.73702012344812));
#33746=CARTESIAN_POINT('Ctrl Pts',(-17.0802404735808,-16.4123522628063,
4.69535345678145));
#33747=CARTESIAN_POINT('Ctrl Pts',(-16.2901202367904,-16.8685283942094,
4.65368679011478));
#33748=CARTESIAN_POINT('Ctrl Pts',(-15.4999999999999,-17.3247045256125,
4.61202012344811));
#33749=CARTESIAN_POINT('Ctrl Pts',(-14.7098797632095,-16.8685283942094,
4.57035345678145));
#33750=CARTESIAN_POINT('Ctrl Pts',(-13.9197595264191,-16.4123522628063,
4.52868679011478));
#33751=CARTESIAN_POINT('Ctrl Pts',(-13.9197595264191,-15.5,4.48702012344811));
#33752=CARTESIAN_POINT('Ctrl Pts',(-13.9197595264191,-14.5876477371938,
4.44535345678144));
#33753=CARTESIAN_POINT('Ctrl Pts',(-14.7098797632095,-14.1314716057907,
4.40368679011478));
#33754=CARTESIAN_POINT('Ctrl Pts',(-15.5,-13.6752954743876,4.36202012344811));
#33755=CARTESIAN_POINT('Ctrl Pts',(-16.2901202367904,-14.1314716057907,
4.32035345678144));
#33756=CARTESIAN_POINT('Ctrl Pts',(-17.0802404735808,-14.5876477371938,
4.27868679011477));
#33757=CARTESIAN_POINT('Ctrl Pts',(-17.0802404735808,-15.5000000000001,
4.23702012344811));
#33758=CARTESIAN_POINT('Ctrl Pts',(-17.0802404735808,-16.4123522628063,
4.19535345678144));
#33759=CARTESIAN_POINT('Ctrl Pts',(-16.2901202367904,-16.8685283942094,
4.15368679011477));
#33760=CARTESIAN_POINT('Ctrl Pts',(-15.4999999999999,-17.3247045256125,
4.11202012344811));
#33761=CARTESIAN_POINT('Ctrl Pts',(-14.7098797632095,-16.8685283942094,
4.07035345678144));
#33762=CARTESIAN_POINT('Ctrl Pts',(-13.9197595264191,-16.4123522628063,
4.02868679011477));
#33763=CARTESIAN_POINT('Ctrl Pts',(-13.9197595264191,-15.5,3.9870201234481));
#33764=CARTESIAN_POINT('Ctrl Pts',(-13.9197595264191,-14.5876477371938,
3.94535345678144));
#33765=CARTESIAN_POINT('Ctrl Pts',(-14.7098797632095,-14.1314716057907,
3.90368679011477));
#33766=CARTESIAN_POINT('Ctrl Pts',(-15.5,-13.6752954743876,3.8620201234481));
#33767=CARTESIAN_POINT('Ctrl Pts',(-16.2901202367904,-14.1314716057907,
3.82035345678144));
#33768=CARTESIAN_POINT('Ctrl Pts',(-17.0802404735808,-14.5876477371938,
3.77868679011477));
#33769=CARTESIAN_POINT('Ctrl Pts',(-17.0802404735808,-15.5000000000001,
3.7370201234481));
#33770=CARTESIAN_POINT('Ctrl Pts',(-17.0802404735808,-16.4123522628063,
3.69535345678143));
#33771=CARTESIAN_POINT('Ctrl Pts',(-16.2901202367904,-16.8685283942094,
3.65368679011477));
#33772=CARTESIAN_POINT('Ctrl Pts',(-15.4999999999999,-17.3247045256125,
3.6120201234481));
#33773=CARTESIAN_POINT('Ctrl Pts',(-14.7098797632095,-16.8685283942094,
3.57035345678143));
#33774=CARTESIAN_POINT('Ctrl Pts',(-13.9197595264191,-16.4123522628063,
3.52868679011477));
#33775=CARTESIAN_POINT('Ctrl Pts',(-13.9197595264191,-15.5,3.4870201234481));
#33776=CARTESIAN_POINT('Ctrl Pts',(-13.9197595264191,-14.5876477371938,
3.44535345678143));
#33777=CARTESIAN_POINT('Ctrl Pts',(-14.7098797632095,-14.1314716057907,
3.40368679011476));
#33778=CARTESIAN_POINT('Ctrl Pts',(-15.5,-13.6752954743876,3.3620201234481));
#33779=CARTESIAN_POINT('Ctrl Pts',(-16.2901202367904,-14.1314716057907,
3.32035345678143));
#33780=CARTESIAN_POINT('Ctrl Pts',(-17.0802404735808,-14.5876477371938,
3.27868679011476));
#33781=CARTESIAN_POINT('Ctrl Pts',(-17.0802404735808,-15.5000000000001,
3.2370201234481));
#33782=CARTESIAN_POINT('Ctrl Pts',(-17.0802404735808,-16.4123522628063,
3.19535345678143));
#33783=CARTESIAN_POINT('Ctrl Pts',(-16.2901202367904,-16.8685283942094,
3.15368679011476));
#33784=CARTESIAN_POINT('Ctrl Pts',(-15.4999999999999,-17.3247045256125,
3.11202012344809));
#33785=CARTESIAN_POINT('Ctrl Pts',(-14.7098797632095,-16.8685283942094,
3.07035345678143));
#33786=CARTESIAN_POINT('Ctrl Pts',(-13.9197595264191,-16.4123522628063,
3.02868679011476));
#33787=CARTESIAN_POINT('Ctrl Pts',(-13.9197595264191,-15.5,2.98702012344809));
#33788=CARTESIAN_POINT('Ctrl Pts',(-13.9197595264191,-14.5876477371938,
2.94535345678143));
#33789=CARTESIAN_POINT('Ctrl Pts',(-14.7098797632095,-14.1314716057907,
2.90368679011476));
#33790=CARTESIAN_POINT('Ctrl Pts',(-15.5,-13.6752954743876,2.86202012344809));
#33791=CARTESIAN_POINT('Ctrl Pts',(-16.2901202367904,-14.1314716057907,
2.82035345678142));
#33792=CARTESIAN_POINT('Ctrl Pts',(-17.0802404735808,-14.5876477371938,
2.77868679011475));
#33793=CARTESIAN_POINT('Ctrl Pts',(-17.0802404735808,-15.5000000000001,
2.73702012344809));
#33794=CARTESIAN_POINT('Ctrl Pts',(-17.0802404735808,-16.4123522628063,
2.69535345678142));
#33795=CARTESIAN_POINT('Ctrl Pts',(-16.2901202367904,-16.8685283942094,
2.65368679011475));
#33796=CARTESIAN_POINT('Ctrl Pts',(-15.4999999999999,-17.3247045256125,
2.61202012344809));
#33797=CARTESIAN_POINT('Ctrl Pts',(-14.7098797632095,-16.8685283942094,
2.57035345678142));
#33798=CARTESIAN_POINT('Ctrl Pts',(-13.9197595264191,-16.4123522628063,
2.52868679011475));
#33799=CARTESIAN_POINT('Ctrl Pts',(-13.9197595264191,-15.5,2.48702012344808));
#33800=CARTESIAN_POINT('Ctrl Pts',(-13.9197595264191,-14.5876477371938,
2.44535345678142));
#33801=CARTESIAN_POINT('Ctrl Pts',(-14.7098797632095,-14.1314716057907,
2.40368679011475));
#33802=CARTESIAN_POINT('Ctrl Pts',(-15.5,-13.6752954743876,2.36202012344808));
#33803=CARTESIAN_POINT('Ctrl Pts',(-16.2901202367904,-14.1314716057907,
2.32035345678142));
#33804=CARTESIAN_POINT('Ctrl Pts',(-17.0802404735808,-14.5876477371938,
2.27868679011475));
#33805=CARTESIAN_POINT('Ctrl Pts',(-17.0802404735808,-15.5000000000001,
2.23702012344808));
#33806=CARTESIAN_POINT('Ctrl Pts',(-17.0802404735808,-16.4123522628063,
2.19535345678142));
#33807=CARTESIAN_POINT('Ctrl Pts',(-16.2901202367904,-16.8685283942094,
2.15368679011475));
#33808=CARTESIAN_POINT('Ctrl Pts',(-15.4999999999999,-17.3247045256125,
2.11202012344808));
#33809=CARTESIAN_POINT('Ctrl Pts',(-14.7098797632095,-16.8685283942094,
2.07035345678141));
#33810=CARTESIAN_POINT('Ctrl Pts',(-13.9197595264191,-16.4123522628063,
2.02868679011475));
#33811=CARTESIAN_POINT('Ctrl Pts',(-13.9197595264191,-15.5,1.98702012344808));
#33812=CARTESIAN_POINT('Ctrl Pts',(-13.9197595264191,-14.5876477371938,
1.94535345678141));
#33813=CARTESIAN_POINT('Ctrl Pts',(-14.7098797632095,-14.1314716057907,
1.90368679011474));
#33814=CARTESIAN_POINT('Ctrl Pts',(-15.5,-13.6752954743876,1.86202012344808));
#33815=CARTESIAN_POINT('Ctrl Pts',(-16.2901202367904,-14.1314716057907,
1.82035345678141));
#33816=CARTESIAN_POINT('Ctrl Pts',(-17.0802404735808,-14.5876477371938,
1.77868679011474));
#33817=CARTESIAN_POINT('Ctrl Pts',(-17.0802404735808,-15.5000000000001,
1.73702012344808));
#33818=CARTESIAN_POINT('Ctrl Pts',(-17.0802404735808,-16.4123522628063,
1.69535345678141));
#33819=CARTESIAN_POINT('Ctrl Pts',(-16.2901202367904,-16.8685283942094,
1.65368679011474));
#33820=CARTESIAN_POINT('Ctrl Pts',(-15.4999999999999,-17.3247045256125,
1.61202012344807));
#33821=CARTESIAN_POINT('Ctrl Pts',(-14.7098797632095,-16.8685283942094,
1.57035345678141));
#33822=CARTESIAN_POINT('Ctrl Pts',(-13.9197595264191,-16.4123522628063,
1.52868679011474));
#33823=CARTESIAN_POINT('Ctrl Pts',(-13.9197595264191,-15.5,1.48702012344807));
#33824=CARTESIAN_POINT('Ctrl Pts',(-13.9197595264191,-14.5876477371938,
1.4453534567814));
#33825=CARTESIAN_POINT('Ctrl Pts',(-14.7098797632095,-14.1314716057907,
1.40368679011474));
#33826=CARTESIAN_POINT('Ctrl Pts',(-15.5,-13.6752954743876,1.36202012344807));
#33827=CARTESIAN_POINT('Ctrl Pts',(-16.2901202367904,-14.1314716057907,
1.3203534567814));
#33828=CARTESIAN_POINT('Ctrl Pts',(-17.0802404735808,-14.5876477371938,
1.27868679011473));
#33829=CARTESIAN_POINT('Ctrl Pts',(-17.0802404735808,-15.5000000000001,
1.23702012344807));
#33830=CARTESIAN_POINT('Ctrl Pts',(-17.0802404735808,-16.4123522628063,
1.1953534567814));
#33831=CARTESIAN_POINT('Ctrl Pts',(-16.2901202367904,-16.8685283942094,
1.15368679011473));
#33832=CARTESIAN_POINT('Ctrl Pts',(-15.4999999999999,-17.3247045256125,
1.11202012344807));
#33833=CARTESIAN_POINT('Ctrl Pts',(-14.7098797632095,-16.8685283942094,
1.0703534567814));
#33834=CARTESIAN_POINT('Ctrl Pts',(-13.9197595264191,-16.4123522628063,
1.02868679011473));
#33835=CARTESIAN_POINT('Ctrl Pts',(-13.9197595264191,-15.5,0.987020123448066));
#33836=CARTESIAN_POINT('Ctrl Pts',(-13.9197595264191,-14.5876477371938,
0.945353456781398));
#33837=CARTESIAN_POINT('Ctrl Pts',(-14.7098797632095,-14.1314716057907,
0.903686790114731));
#33838=CARTESIAN_POINT('Ctrl Pts',(-15.5,-13.6752954743876,0.862020123448064));
#33839=CARTESIAN_POINT('Ctrl Pts',(-16.2901202367904,-14.1314716057907,
0.820353456781396));
#33840=CARTESIAN_POINT('Ctrl Pts',(-17.0802404735808,-14.5876477371938,
0.778686790114729));
#33841=CARTESIAN_POINT('Ctrl Pts',(-17.0802404735808,-15.5000000000001,
0.737020123448062));
#33842=CARTESIAN_POINT('Ctrl Pts',(-17.0802404735808,-16.4123522628063,
0.695353456781395));
#33843=CARTESIAN_POINT('Ctrl Pts',(-16.2901202367904,-16.8685283942094,
0.653686790114727));
#33844=CARTESIAN_POINT('Ctrl Pts',(-15.4999999999999,-17.3247045256125,
0.61202012344806));
#33845=CARTESIAN_POINT('Ctrl Pts',(-14.7098797632095,-16.8685283942094,
0.570353456781393));
#33846=CARTESIAN_POINT('Ctrl Pts',(-13.9197595264191,-16.4123522628063,
0.528686790114725));
#33847=CARTESIAN_POINT('Ctrl Pts',(-13.9197595264191,-15.5,0.487020123448058));
#33848=CARTESIAN_POINT('Ctrl Pts',(-13.9197595264191,-14.5876477371938,
0.445353456781391));
#33849=CARTESIAN_POINT('Ctrl Pts',(-14.7098797632095,-14.1314716057907,
0.403686790114724));
#33850=CARTESIAN_POINT('Ctrl Pts',(-15.5,-13.6752954743876,0.362020123448056));
#33851=CARTESIAN_POINT('Ctrl Pts',(-16.2901202367904,-14.1314716057907,
0.320353456781389));
#33852=CARTESIAN_POINT('Ctrl Pts',(-17.0802404735808,-14.5876477371938,
0.278686790114722));
#33853=CARTESIAN_POINT('Ctrl Pts',(-17.0802404735808,-15.5000000000001,
0.237020123448054));
#33854=CARTESIAN_POINT('Ctrl Pts',(-17.0802404735808,-16.4123522628063,
0.195353456781387));
#33855=CARTESIAN_POINT('Ctrl Pts',(-16.2901202367904,-16.8685283942094,
0.15368679011472));
#33856=CARTESIAN_POINT('Ctrl Pts',(-15.4999999999999,-17.3247045256125,
0.112020123448053));
#33857=CARTESIAN_POINT('Ctrl Pts',(-14.7098797632095,-16.8685283942094,
0.0703534567813853));
#33858=CARTESIAN_POINT('Ctrl Pts',(-13.9197595264191,-16.4123522628063,
0.028686790114718));
#33859=CARTESIAN_POINT('Ctrl Pts',(-13.9197595264191,-15.5,-0.0129798765519493));
#33860=CARTESIAN_POINT('Ctrl Pts',(-13.9197595264191,-14.5876477371938,
-0.0546465432186148));
#33861=CARTESIAN_POINT('Ctrl Pts',(-14.7098797632095,-14.1314716057907,
-0.0963132098852821));
#33862=CARTESIAN_POINT('Ctrl Pts',(-15.5,-13.6752954743876,-0.137979876551949));
#33863=CARTESIAN_POINT('Ctrl Pts',(-16.2901202367904,-14.1314716057907,
-0.179646543218617));
#33864=CARTESIAN_POINT('Ctrl Pts',(-17.0802404735808,-14.5876477371938,
-0.221313209885284));
#33865=CARTESIAN_POINT('Ctrl Pts',(-17.0802404735808,-15.5000000000001,
-0.262979876551951));
#33866=CARTESIAN_POINT('Ctrl Pts',(-17.0802404735808,-16.4123522628063,
-0.304646543218619));
#33867=CARTESIAN_POINT('Ctrl Pts',(-16.2901202367904,-16.8685283942094,
-0.346313209885286));
#33868=CARTESIAN_POINT('Ctrl Pts',(-15.4999999999999,-17.3247045256125,
-0.387979876551953));
#33869=CARTESIAN_POINT('Ctrl Pts',(-14.7098797632095,-16.8685283942094,
-0.42964654321862));
#33870=CARTESIAN_POINT('Ctrl Pts',(-13.9197595264191,-16.4123522628063,
-0.471313209885288));
#33871=CARTESIAN_POINT('Ctrl Pts',(-13.9197595264191,-15.5,-0.512979876551955));
#33872=CARTESIAN_POINT('Ctrl Pts',(-13.9197595264191,-14.5876477371938,
-0.554646543218622));
#33873=CARTESIAN_POINT('Ctrl Pts',(-14.7098797632095,-14.1314716057907,
-0.596313209885289));
#33874=CARTESIAN_POINT('Ctrl Pts',(-15.5,-13.6752954743876,-0.637979876551957));
#33875=CARTESIAN_POINT('Ctrl Pts',(-16.2901202367904,-14.1314716057907,
-0.679646543218624));
#33876=CARTESIAN_POINT('Ctrl Pts',(-17.0802404735808,-14.5876477371938,
-0.721313209885291));
#33877=CARTESIAN_POINT('Ctrl Pts',(-17.0802404735808,-15.5000000000001,
-0.762979876551959));
#33878=CARTESIAN_POINT('Ctrl Pts',(-17.0802404735808,-16.4123522628063,
-0.804646543218626));
#33879=CARTESIAN_POINT('Ctrl Pts',(-16.2901202367904,-16.8685283942094,
-0.846313209885293));
#33880=CARTESIAN_POINT('Ctrl Pts',(-15.4999999999999,-17.3247045256125,
-0.88797987655196));
#33881=CARTESIAN_POINT('Ctrl Pts',(-14.7098797632095,-16.8685283942094,
-0.929646543218628));
#33882=CARTESIAN_POINT('Ctrl Pts',(-13.9197595264191,-16.4123522628063,
-0.971313209885295));
#33883=CARTESIAN_POINT('Ctrl Pts',(-13.9197595264191,-15.5,-1.01297987655196));
#33884=CARTESIAN_POINT('Ctrl Pts',(-13.9197595264191,-14.5876477371938,
-1.05464654321863));
#33885=CARTESIAN_POINT('Ctrl Pts',(-14.7098797632095,-14.1314716057907,
-1.0963132098853));
#33886=CARTESIAN_POINT('Ctrl Pts',(-15.5,-13.6752954743876,-1.13797987655196));
#33887=CARTESIAN_POINT('Ctrl Pts',(-16.2901202367904,-14.1314716057907,
-1.17964654321863));
#33888=CARTESIAN_POINT('Ctrl Pts',(-17.0802404735808,-14.5876477371938,
-1.2213132098853));
#33889=CARTESIAN_POINT('Ctrl Pts',(-17.0802404735808,-15.5000000000001,
-1.26297987655196));
#33890=CARTESIAN_POINT('Ctrl Pts',(-17.0802404735808,-16.4123522628063,
-1.30464654321863));
#33891=CARTESIAN_POINT('Ctrl Pts',(-16.2901202367904,-16.8685283942094,
-1.3463132098853));
#33892=CARTESIAN_POINT('Ctrl Pts',(-15.4999999999999,-17.3247045256125,
-1.38797987655197));
#33893=CARTESIAN_POINT('Ctrl Pts',(-14.7098797632095,-16.8685283942094,
-1.42964654321863));
#33894=CARTESIAN_POINT('Ctrl Pts',(-13.9197595264191,-16.4123522628063,
-1.4713132098853));
#33895=CARTESIAN_POINT('Ctrl Pts',(-13.9197595264191,-15.5,-1.51297987655197));
#33896=CARTESIAN_POINT('Ctrl Pts',(-13.9197595264191,-14.5876477371938,
-1.55464654321864));
#33897=CARTESIAN_POINT('Ctrl Pts',(-14.7098797632095,-14.1314716057907,
-1.5963132098853));
#33898=CARTESIAN_POINT('Ctrl Pts',(-15.5,-13.6752954743876,-1.63797987655197));
#33899=CARTESIAN_POINT('Ctrl Pts',(-16.2901202367904,-14.1314716057907,
-1.67964654321864));
#33900=CARTESIAN_POINT('Ctrl Pts',(-17.0802404735808,-14.5876477371938,
-1.7213132098853));
#33901=CARTESIAN_POINT('Ctrl Pts',(-17.0802404735808,-15.5000000000001,
-1.76297987655197));
#33902=CARTESIAN_POINT('Ctrl Pts',(-17.0802404735808,-16.4123522628063,
-1.80464654321864));
#33903=CARTESIAN_POINT('Ctrl Pts',(-16.2901202367904,-16.8685283942094,
-1.84631320988531));
#33904=CARTESIAN_POINT('Ctrl Pts',(-15.4999999999999,-17.3247045256125,
-1.88797987655197));
#33905=CARTESIAN_POINT('Ctrl Pts',(-14.7098797632095,-16.8685283942094,
-1.92964654321864));
#33906=CARTESIAN_POINT('Ctrl Pts',(-14.4189900731898,-16.7005831533721,
-1.94498649173085));
#33907=CARTESIAN_POINT('Ctrl Pts',(-14.2215586016756,-16.4288420454488,
-1.96260250461286));
#33908=CARTESIAN_POINT('Ctrl Pts',(-13.4352476007234,-15.3465777998746,
-2.03276185973389));
#33909=CARTESIAN_POINT('Ctrl Pts',(-12.6489365997712,-14.2643135543004,
-2.10292121485492));
#33910=CARTESIAN_POINT('Ctrl Pts',(-17.0802404735808,-15.5000000000001,
11.1745));
#33911=CARTESIAN_POINT('Ctrl Pts',(-17.0802404735808,-16.4123522628063,
11.1328333333333));
#33912=CARTESIAN_POINT('Ctrl Pts',(-16.2901202367904,-16.8685283942094,
11.0911666666667));
#33913=CARTESIAN_POINT('Ctrl Pts',(-15.4999999999999,-17.3247045256125,
11.0495));
#33914=CARTESIAN_POINT('Ctrl Pts',(-14.7098797632095,-16.8685283942094,
11.0078333333333));
#33915=CARTESIAN_POINT('Ctrl Pts',(-13.9197595264191,-16.4123522628063,
10.9661666666667));
#33916=CARTESIAN_POINT('Ctrl Pts',(-13.9197595264191,-15.5,10.9245));
#33917=CARTESIAN_POINT('Ctrl Pts',(-13.9197595264191,-14.5876477371938,
10.8828333333333));
#33918=CARTESIAN_POINT('Ctrl Pts',(-14.7098797632095,-14.1314716057907,
10.8411666666667));
#33919=CARTESIAN_POINT('Ctrl Pts',(-15.5,-13.6752954743876,10.7995));
#33920=CARTESIAN_POINT('Ctrl Pts',(-16.2901202367904,-14.1314716057907,
10.7578333333333));
#33921=CARTESIAN_POINT('Ctrl Pts',(-17.0802404735808,-14.5876477371938,
10.7161666666667));
#33922=CARTESIAN_POINT('Ctrl Pts',(-17.0802404735808,-15.5000000000001,
10.6745));
#33923=CARTESIAN_POINT('Ctrl Pts',(-17.0802404735808,-16.4123522628063,
10.6328333333333));
#33924=CARTESIAN_POINT('Ctrl Pts',(-16.2901202367904,-16.8685283942094,
10.5911666666667));
#33925=CARTESIAN_POINT('Ctrl Pts',(-15.4999999999999,-17.3247045256125,
10.5495));
#33926=CARTESIAN_POINT('Ctrl Pts',(-14.7098797632095,-16.8685283942094,
10.5078333333333));
#33927=CARTESIAN_POINT('Ctrl Pts',(-13.9197595264191,-16.4123522628063,
10.4661666666667));
#33928=CARTESIAN_POINT('Ctrl Pts',(-13.9197595264191,-15.5,10.4245));
#33929=CARTESIAN_POINT('Ctrl Pts',(-13.9197595264191,-14.5876477371938,
10.3828333333333));
#33930=CARTESIAN_POINT('Ctrl Pts',(-14.7098797632095,-14.1314716057907,
10.3411666666667));
#33931=CARTESIAN_POINT('Ctrl Pts',(-15.5,-13.6752954743876,10.2995));
#33932=CARTESIAN_POINT('Ctrl Pts',(-16.2901202367904,-14.1314716057907,
10.2578333333333));
#33933=CARTESIAN_POINT('Ctrl Pts',(-17.0802404735808,-14.5876477371938,
10.2161666666667));
#33934=CARTESIAN_POINT('Ctrl Pts',(-17.0802404735808,-15.5000000000001,
10.1745));
#33935=CARTESIAN_POINT('Ctrl Pts',(-17.0802404735808,-16.4123522628063,
10.1328333333333));
#33936=CARTESIAN_POINT('Ctrl Pts',(-16.2901202367904,-16.8685283942094,
10.0911666666667));
#33937=CARTESIAN_POINT('Ctrl Pts',(-15.4999999999999,-17.3247045256125,
10.0495));
#33938=CARTESIAN_POINT('Ctrl Pts',(-14.7098797632095,-16.8685283942094,
10.0078333333333));
#33939=CARTESIAN_POINT('Ctrl Pts',(-13.9197595264191,-16.4123522628063,
9.96616666666665));
#33940=CARTESIAN_POINT('Ctrl Pts',(-13.9197595264191,-15.5,9.92449999999998));
#33941=CARTESIAN_POINT('Ctrl Pts',(-13.9197595264191,-14.5876477371938,
9.88283333333331));
#33942=CARTESIAN_POINT('Ctrl Pts',(-14.7098797632095,-14.1314716057907,
9.84116666666665));
#33943=CARTESIAN_POINT('Ctrl Pts',(-15.5,-13.6752954743876,9.79949999999998));
#33944=CARTESIAN_POINT('Ctrl Pts',(-16.2901202367904,-14.1314716057907,
9.75783333333331));
#33945=CARTESIAN_POINT('Ctrl Pts',(-17.0802404735808,-14.5876477371938,
9.71616666666665));
#33946=CARTESIAN_POINT('Ctrl Pts',(-17.0802404735808,-15.5000000000001,
9.67449999999998));
#33947=CARTESIAN_POINT('Ctrl Pts',(-17.0802404735808,-16.4123522628063,
9.63283333333331));
#33948=CARTESIAN_POINT('Ctrl Pts',(-16.2901202367904,-16.8685283942094,
9.59116666666664));
#33949=CARTESIAN_POINT('Ctrl Pts',(-15.4999999999999,-17.3247045256125,
9.54949999999998));
#33950=CARTESIAN_POINT('Ctrl Pts',(-14.7098797632095,-16.8685283942094,
9.50783333333331));
#33951=CARTESIAN_POINT('Ctrl Pts',(-13.9197595264191,-16.4123522628063,
9.46616666666664));
#33952=CARTESIAN_POINT('Ctrl Pts',(-13.9197595264191,-15.5,9.42449999999998));
#33953=CARTESIAN_POINT('Ctrl Pts',(-13.9197595264191,-14.5876477371938,
9.38283333333331));
#33954=CARTESIAN_POINT('Ctrl Pts',(-14.7098797632095,-14.1314716057907,
9.34116666666664));
#33955=CARTESIAN_POINT('Ctrl Pts',(-15.5,-13.6752954743876,9.29949999999998));
#33956=CARTESIAN_POINT('Ctrl Pts',(-16.2901202367904,-14.1314716057907,
9.25783333333331));
#33957=CARTESIAN_POINT('Ctrl Pts',(-17.0802404735808,-14.5876477371938,
9.21616666666664));
#33958=CARTESIAN_POINT('Ctrl Pts',(-17.0802404735808,-15.5000000000001,
9.17449999999997));
#33959=CARTESIAN_POINT('Ctrl Pts',(-17.0802404735808,-16.4123522628063,
9.13283333333331));
#33960=CARTESIAN_POINT('Ctrl Pts',(-16.2901202367904,-16.8685283942094,
9.09116666666664));
#33961=CARTESIAN_POINT('Ctrl Pts',(-15.4999999999999,-17.3247045256125,
9.04949999999997));
#33962=CARTESIAN_POINT('Ctrl Pts',(-14.7098797632095,-16.8685283942094,
9.0078333333333));
#33963=CARTESIAN_POINT('Ctrl Pts',(-13.9197595264191,-16.4123522628063,
8.96616666666664));
#33964=CARTESIAN_POINT('Ctrl Pts',(-13.9197595264191,-15.5,8.92449999999997));
#33965=CARTESIAN_POINT('Ctrl Pts',(-13.9197595264191,-14.5876477371938,
8.8828333333333));
#33966=CARTESIAN_POINT('Ctrl Pts',(-14.7098797632095,-14.1314716057907,
8.84116666666664));
#33967=CARTESIAN_POINT('Ctrl Pts',(-15.5,-13.6752954743876,8.79949999999997));
#33968=CARTESIAN_POINT('Ctrl Pts',(-16.2901202367904,-14.1314716057907,
8.7578333333333));
#33969=CARTESIAN_POINT('Ctrl Pts',(-17.0802404735808,-14.5876477371938,
8.71616666666663));
#33970=CARTESIAN_POINT('Ctrl Pts',(-17.0802404735808,-15.5000000000001,
8.67449999999997));
#33971=CARTESIAN_POINT('Ctrl Pts',(-17.0802404735808,-16.4123522628063,
8.6328333333333));
#33972=CARTESIAN_POINT('Ctrl Pts',(-16.2901202367904,-16.8685283942094,
8.59116666666663));
#33973=CARTESIAN_POINT('Ctrl Pts',(-15.4999999999999,-17.3247045256125,
8.54949999999996));
#33974=CARTESIAN_POINT('Ctrl Pts',(-14.7098797632095,-16.8685283942094,
8.50783333333329));
#33975=CARTESIAN_POINT('Ctrl Pts',(-13.9197595264191,-16.4123522628063,
8.46616666666663));
#33976=CARTESIAN_POINT('Ctrl Pts',(-13.9197595264191,-15.5,8.42449999999996));
#33977=CARTESIAN_POINT('Ctrl Pts',(-13.9197595264191,-14.5876477371938,
8.3828333333333));
#33978=CARTESIAN_POINT('Ctrl Pts',(-14.7098797632095,-14.1314716057907,
8.34116666666663));
#33979=CARTESIAN_POINT('Ctrl Pts',(-15.5,-13.6752954743876,8.29949999999996));
#33980=CARTESIAN_POINT('Ctrl Pts',(-16.2901202367904,-14.1314716057907,
8.25783333333329));
#33981=CARTESIAN_POINT('Ctrl Pts',(-17.0802404735808,-14.5876477371938,
8.21616666666663));
#33982=CARTESIAN_POINT('Ctrl Pts',(-17.0802404735808,-15.5000000000001,
8.17449999999996));
#33983=CARTESIAN_POINT('Ctrl Pts',(-17.0802404735808,-16.4123522628063,
8.13283333333329));
#33984=CARTESIAN_POINT('Ctrl Pts',(-16.2901202367904,-16.8685283942094,
8.09116666666663));
#33985=CARTESIAN_POINT('Ctrl Pts',(-15.4999999999999,-17.3247045256125,
8.04949999999996));
#33986=CARTESIAN_POINT('Ctrl Pts',(-14.7098797632095,-16.8685283942094,
8.00783333333329));
#33987=CARTESIAN_POINT('Ctrl Pts',(-13.9197595264191,-16.4123522628063,
7.96616666666662));
#33988=CARTESIAN_POINT('Ctrl Pts',(-13.9197595264191,-15.5,7.92449999999996));
#33989=CARTESIAN_POINT('Ctrl Pts',(-13.9197595264191,-14.5876477371938,
7.88283333333329));
#33990=CARTESIAN_POINT('Ctrl Pts',(-14.7098797632095,-14.1314716057907,
7.84116666666662));
#33991=CARTESIAN_POINT('Ctrl Pts',(-15.5,-13.6752954743876,7.79949999999995));
#33992=CARTESIAN_POINT('Ctrl Pts',(-16.2901202367904,-14.1314716057907,
7.75783333333329));
#33993=CARTESIAN_POINT('Ctrl Pts',(-17.0802404735808,-14.5876477371938,
7.71616666666662));
#33994=CARTESIAN_POINT('Ctrl Pts',(-17.0802404735808,-15.5000000000001,
7.67449999999995));
#33995=CARTESIAN_POINT('Ctrl Pts',(-17.0802404735808,-16.4123522628063,
7.63283333333328));
#33996=CARTESIAN_POINT('Ctrl Pts',(-16.2901202367904,-16.8685283942094,
7.59116666666662));
#33997=CARTESIAN_POINT('Ctrl Pts',(-15.4999999999999,-17.3247045256125,
7.54949999999995));
#33998=CARTESIAN_POINT('Ctrl Pts',(-14.7098797632095,-16.8685283942094,
7.50783333333328));
#33999=CARTESIAN_POINT('Ctrl Pts',(-13.9197595264191,-16.4123522628063,
7.46616666666662));
#34000=CARTESIAN_POINT('Ctrl Pts',(-13.9197595264191,-15.5,7.42449999999995));
#34001=CARTESIAN_POINT('Ctrl Pts',(-13.9197595264191,-14.5876477371938,
7.38283333333328));
#34002=CARTESIAN_POINT('Ctrl Pts',(-14.7098797632095,-14.1314716057907,
7.34116666666661));
#34003=CARTESIAN_POINT('Ctrl Pts',(-15.5,-13.6752954743876,7.29949999999995));
#34004=CARTESIAN_POINT('Ctrl Pts',(-16.2901202367904,-14.1314716057907,
7.25783333333328));
#34005=CARTESIAN_POINT('Ctrl Pts',(-17.0802404735808,-14.5876477371938,
7.21616666666661));
#34006=CARTESIAN_POINT('Ctrl Pts',(-17.0802404735808,-15.5000000000001,
7.17449999999995));
#34007=CARTESIAN_POINT('Ctrl Pts',(-17.0802404735808,-16.4123522628063,
7.13283333333328));
#34008=CARTESIAN_POINT('Ctrl Pts',(-16.2901202367904,-16.8685283942094,
7.09116666666661));
#34009=CARTESIAN_POINT('Ctrl Pts',(-15.4999999999999,-17.3247045256125,
7.04949999999994));
#34010=CARTESIAN_POINT('Ctrl Pts',(-14.7098797632095,-16.8685283942094,
7.00783333333328));
#34011=CARTESIAN_POINT('Ctrl Pts',(-13.9197595264191,-16.4123522628063,
6.96616666666661));
#34012=CARTESIAN_POINT('Ctrl Pts',(-13.9197595264191,-15.5,6.92449999999994));
#34013=CARTESIAN_POINT('Ctrl Pts',(-13.9197595264191,-14.5876477371938,
6.88283333333327));
#34014=CARTESIAN_POINT('Ctrl Pts',(-14.7098797632095,-14.1314716057907,
6.84116666666661));
#34015=CARTESIAN_POINT('Ctrl Pts',(-15.5,-13.6752954743876,6.79949999999994));
#34016=CARTESIAN_POINT('Ctrl Pts',(-16.2901202367904,-14.1314716057907,
6.75783333333327));
#34017=CARTESIAN_POINT('Ctrl Pts',(-17.0802404735808,-14.5876477371938,
6.71616666666661));
#34018=CARTESIAN_POINT('Ctrl Pts',(-17.0802404735808,-15.5000000000001,
6.67449999999994));
#34019=CARTESIAN_POINT('Ctrl Pts',(-17.0802404735808,-16.4123522628063,
6.63283333333327));
#34020=CARTESIAN_POINT('Ctrl Pts',(-16.2901202367904,-16.8685283942094,
6.59116666666661));
#34021=CARTESIAN_POINT('Ctrl Pts',(-15.4999999999999,-17.3247045256125,
6.54949999999994));
#34022=CARTESIAN_POINT('Ctrl Pts',(-14.7098797632095,-16.8685283942094,
6.50783333333327));
#34023=CARTESIAN_POINT('Ctrl Pts',(-13.9197595264191,-16.4123522628063,
6.4661666666666));
#34024=CARTESIAN_POINT('Ctrl Pts',(-13.9197595264191,-15.5,6.42449999999994));
#34025=CARTESIAN_POINT('Ctrl Pts',(-13.9197595264191,-14.5876477371938,
6.38283333333327));
#34026=CARTESIAN_POINT('Ctrl Pts',(-14.7098797632095,-14.1314716057907,
6.3411666666666));
#34027=CARTESIAN_POINT('Ctrl Pts',(-15.5,-13.6752954743876,6.29949999999993));
#34028=CARTESIAN_POINT('Ctrl Pts',(-16.2901202367904,-14.1314716057907,
6.25783333333327));
#34029=CARTESIAN_POINT('Ctrl Pts',(-17.0802404735808,-14.5876477371938,
6.2161666666666));
#34030=CARTESIAN_POINT('Ctrl Pts',(-17.0802404735808,-15.5000000000001,
6.17449999999993));
#34031=CARTESIAN_POINT('Ctrl Pts',(-17.0802404735808,-16.4123522628063,
6.13283333333326));
#34032=CARTESIAN_POINT('Ctrl Pts',(-16.2901202367904,-16.8685283942094,
6.0911666666666));
#34033=CARTESIAN_POINT('Ctrl Pts',(-15.4999999999999,-17.3247045256125,
6.04949999999993));
#34034=CARTESIAN_POINT('Ctrl Pts',(-14.7098797632095,-16.8685283942094,
6.00783333333326));
#34035=CARTESIAN_POINT('Ctrl Pts',(-13.9197595264191,-16.4123522628063,
5.9661666666666));
#34036=CARTESIAN_POINT('Ctrl Pts',(-13.9197595264191,-15.5,5.92449999999993));
#34037=CARTESIAN_POINT('Ctrl Pts',(-13.9197595264191,-14.5876477371938,
5.88283333333326));
#34038=CARTESIAN_POINT('Ctrl Pts',(-14.7098797632095,-14.1314716057907,
5.8411666666666));
#34039=CARTESIAN_POINT('Ctrl Pts',(-15.5,-13.6752954743876,5.79949999999993));
#34040=CARTESIAN_POINT('Ctrl Pts',(-16.2901202367904,-14.1314716057907,
5.75783333333326));
#34041=CARTESIAN_POINT('Ctrl Pts',(-17.0802404735808,-14.5876477371938,
5.71616666666659));
#34042=CARTESIAN_POINT('Ctrl Pts',(-17.0802404735808,-15.5000000000001,
5.67449999999993));
#34043=CARTESIAN_POINT('Ctrl Pts',(-17.0802404735808,-16.4123522628063,
5.63283333333326));
#34044=CARTESIAN_POINT('Ctrl Pts',(-16.2901202367904,-16.8685283942094,
5.59116666666659));
#34045=CARTESIAN_POINT('Ctrl Pts',(-15.4999999999999,-17.3247045256125,
5.54949999999992));
#34046=CARTESIAN_POINT('Ctrl Pts',(-14.7098797632095,-16.8685283942094,
5.50783333333326));
#34047=CARTESIAN_POINT('Ctrl Pts',(-13.9197595264191,-16.4123522628063,
5.46616666666659));
#34048=CARTESIAN_POINT('Ctrl Pts',(-13.9197595264191,-15.5,5.42449999999992));
#34049=CARTESIAN_POINT('Ctrl Pts',(-13.9197595264191,-14.5876477371938,
5.38283333333326));
#34050=CARTESIAN_POINT('Ctrl Pts',(-14.7098797632095,-14.1314716057907,
5.34116666666659));
#34051=CARTESIAN_POINT('Ctrl Pts',(-15.5,-13.6752954743876,5.29949999999992));
#34052=CARTESIAN_POINT('Ctrl Pts',(-16.2901202367904,-14.1314716057907,
5.25783333333325));
#34053=CARTESIAN_POINT('Ctrl Pts',(-17.0802404735808,-14.5876477371938,
5.21616666666659));
#34054=CARTESIAN_POINT('Ctrl Pts',(-17.0802404735808,-15.5000000000001,
5.17449999999992));
#34055=CARTESIAN_POINT('Ctrl Pts',(-17.0802404735808,-16.4123522628063,
5.13283333333325));
#34056=CARTESIAN_POINT('Ctrl Pts',(-16.2901202367904,-16.8685283942094,
5.09116666666658));
#34057=CARTESIAN_POINT('Ctrl Pts',(-15.4999999999999,-17.3247045256125,
5.04949999999992));
#34058=CARTESIAN_POINT('Ctrl Pts',(-14.7098797632095,-16.8685283942094,
5.00783333333325));
#34059=CARTESIAN_POINT('Ctrl Pts',(-13.9197595264191,-16.4123522628063,
4.96616666666658));
#34060=CARTESIAN_POINT('Ctrl Pts',(-13.9197595264191,-15.5,4.92449999999992));
#34061=CARTESIAN_POINT('Ctrl Pts',(-13.9197595264191,-14.5876477371938,
4.88283333333325));
#34062=CARTESIAN_POINT('Ctrl Pts',(-14.7098797632095,-14.1314716057907,
4.84116666666658));
#34063=CARTESIAN_POINT('Ctrl Pts',(-15.5,-13.6752954743876,4.79949999999991));
#34064=CARTESIAN_POINT('Ctrl Pts',(-16.2901202367904,-14.1314716057907,
4.75783333333325));
#34065=CARTESIAN_POINT('Ctrl Pts',(-17.0802404735808,-14.5876477371938,
4.71616666666658));
#34066=CARTESIAN_POINT('Ctrl Pts',(-17.0802404735808,-15.5000000000001,
4.67449999999991));
#34067=CARTESIAN_POINT('Ctrl Pts',(-17.0802404735808,-16.4123522628063,
4.63283333333324));
#34068=CARTESIAN_POINT('Ctrl Pts',(-16.2901202367904,-16.8685283942094,
4.59116666666658));
#34069=CARTESIAN_POINT('Ctrl Pts',(-15.4999999999999,-17.3247045256125,
4.54949999999991));
#34070=CARTESIAN_POINT('Ctrl Pts',(-14.7098797632095,-16.8685283942094,
4.50783333333324));
#34071=CARTESIAN_POINT('Ctrl Pts',(-13.9197595264191,-16.4123522628063,
4.46616666666658));
#34072=CARTESIAN_POINT('Ctrl Pts',(-13.9197595264191,-15.5,4.42449999999991));
#34073=CARTESIAN_POINT('Ctrl Pts',(-13.9197595264191,-14.5876477371938,
4.38283333333324));
#34074=CARTESIAN_POINT('Ctrl Pts',(-14.7098797632095,-14.1314716057907,
4.34116666666657));
#34075=CARTESIAN_POINT('Ctrl Pts',(-15.5,-13.6752954743876,4.29949999999991));
#34076=CARTESIAN_POINT('Ctrl Pts',(-16.2901202367904,-14.1314716057907,
4.25783333333324));
#34077=CARTESIAN_POINT('Ctrl Pts',(-17.0802404735808,-14.5876477371938,
4.21616666666657));
#34078=CARTESIAN_POINT('Ctrl Pts',(-17.0802404735808,-15.5000000000001,
4.17449999999991));
#34079=CARTESIAN_POINT('Ctrl Pts',(-17.0802404735808,-16.4123522628063,
4.13283333333324));
#34080=CARTESIAN_POINT('Ctrl Pts',(-16.2901202367904,-16.8685283942094,
4.09116666666657));
#34081=CARTESIAN_POINT('Ctrl Pts',(-15.4999999999999,-17.3247045256125,
4.0494999999999));
#34082=CARTESIAN_POINT('Ctrl Pts',(-14.7098797632095,-16.8685283942094,
4.00783333333324));
#34083=CARTESIAN_POINT('Ctrl Pts',(-13.9197595264191,-16.4123522628063,
3.96616666666657));
#34084=CARTESIAN_POINT('Ctrl Pts',(-13.9197595264191,-15.5,3.9244999999999));
#34085=CARTESIAN_POINT('Ctrl Pts',(-13.9197595264191,-14.5876477371938,
3.88283333333323));
#34086=CARTESIAN_POINT('Ctrl Pts',(-14.7098797632095,-14.1314716057907,
3.84116666666657));
#34087=CARTESIAN_POINT('Ctrl Pts',(-15.5,-13.6752954743876,3.7994999999999));
#34088=CARTESIAN_POINT('Ctrl Pts',(-16.2901202367904,-14.1314716057907,
3.75783333333323));
#34089=CARTESIAN_POINT('Ctrl Pts',(-17.0802404735808,-14.5876477371938,
3.71616666666657));
#34090=CARTESIAN_POINT('Ctrl Pts',(-17.0802404735808,-15.5000000000001,
3.6744999999999));
#34091=CARTESIAN_POINT('Ctrl Pts',(-17.0802404735808,-16.4123522628063,
3.63283333333323));
#34092=CARTESIAN_POINT('Ctrl Pts',(-16.2901202367904,-16.8685283942094,
3.59116666666656));
#34093=CARTESIAN_POINT('Ctrl Pts',(-15.4999999999999,-17.3247045256125,
3.5494999999999));
#34094=CARTESIAN_POINT('Ctrl Pts',(-14.7098797632095,-16.8685283942094,
3.50783333333323));
#34095=CARTESIAN_POINT('Ctrl Pts',(-13.9197595264191,-16.4123522628063,
3.46616666666656));
#34096=CARTESIAN_POINT('Ctrl Pts',(-13.9197595264191,-15.5,3.4244999999999));
#34097=CARTESIAN_POINT('Ctrl Pts',(-13.9197595264191,-14.5876477371938,
3.38283333333323));
#34098=CARTESIAN_POINT('Ctrl Pts',(-14.7098797632095,-14.1314716057907,
3.34116666666656));
#34099=CARTESIAN_POINT('Ctrl Pts',(-15.5,-13.6752954743876,3.29949999999989));
#34100=CARTESIAN_POINT('Ctrl Pts',(-16.2901202367904,-14.1314716057907,
3.25783333333323));
#34101=CARTESIAN_POINT('Ctrl Pts',(-17.0802404735808,-14.5876477371938,
3.21616666666656));
#34102=CARTESIAN_POINT('Ctrl Pts',(-17.0802404735808,-15.5000000000001,
3.17449999999989));
#34103=CARTESIAN_POINT('Ctrl Pts',(-17.0802404735808,-16.4123522628063,
3.13283333333323));
#34104=CARTESIAN_POINT('Ctrl Pts',(-16.2901202367904,-16.8685283942094,
3.09116666666656));
#34105=CARTESIAN_POINT('Ctrl Pts',(-15.4999999999999,-17.3247045256125,
3.04949999999989));
#34106=CARTESIAN_POINT('Ctrl Pts',(-14.7098797632095,-16.8685283942094,
3.00783333333322));
#34107=CARTESIAN_POINT('Ctrl Pts',(-13.9197595264191,-16.4123522628063,
2.96616666666656));
#34108=CARTESIAN_POINT('Ctrl Pts',(-13.9197595264191,-15.5,2.92449999999989));
#34109=CARTESIAN_POINT('Ctrl Pts',(-13.9197595264191,-14.5876477371938,
2.88283333333322));
#34110=CARTESIAN_POINT('Ctrl Pts',(-14.7098797632095,-14.1314716057907,
2.84116666666655));
#34111=CARTESIAN_POINT('Ctrl Pts',(-15.5,-13.6752954743876,2.79949999999989));
#34112=CARTESIAN_POINT('Ctrl Pts',(-16.2901202367904,-14.1314716057907,
2.75783333333322));
#34113=CARTESIAN_POINT('Ctrl Pts',(-17.0802404735808,-14.5876477371938,
2.71616666666655));
#34114=CARTESIAN_POINT('Ctrl Pts',(-17.0802404735808,-15.5000000000001,
2.67449999999989));
#34115=CARTESIAN_POINT('Ctrl Pts',(-17.0802404735808,-16.4123522628063,
2.63283333333322));
#34116=CARTESIAN_POINT('Ctrl Pts',(-16.2901202367904,-16.8685283942094,
2.59116666666655));
#34117=CARTESIAN_POINT('Ctrl Pts',(-15.4999999999999,-17.3247045256125,
2.54949999999988));
#34118=CARTESIAN_POINT('Ctrl Pts',(-14.7098797632095,-16.8685283942094,
2.50783333333322));
#34119=CARTESIAN_POINT('Ctrl Pts',(-13.9197595264191,-16.4123522628063,
2.46616666666655));
#34120=CARTESIAN_POINT('Ctrl Pts',(-13.9197595264191,-15.5,2.42449999999988));
#34121=CARTESIAN_POINT('Ctrl Pts',(-13.9197595264191,-14.5876477371938,
2.38283333333321));
#34122=CARTESIAN_POINT('Ctrl Pts',(-14.7098797632095,-14.1314716057907,
2.34116666666655));
#34123=CARTESIAN_POINT('Ctrl Pts',(-15.5,-13.6752954743876,2.29949999999988));
#34124=CARTESIAN_POINT('Ctrl Pts',(-16.2901202367904,-14.1314716057907,
2.25783333333321));
#34125=CARTESIAN_POINT('Ctrl Pts',(-17.0802404735808,-14.5876477371938,
2.21616666666655));
#34126=CARTESIAN_POINT('Ctrl Pts',(-17.0802404735808,-15.5000000000001,
2.17449999999988));
#34127=CARTESIAN_POINT('Ctrl Pts',(-17.0802404735808,-16.4123522628063,
2.13283333333321));
#34128=CARTESIAN_POINT('Ctrl Pts',(-16.2901202367904,-16.8685283942094,
2.09116666666655));
#34129=CARTESIAN_POINT('Ctrl Pts',(-15.4999999999999,-17.3247045256125,
2.04949999999988));
#34130=CARTESIAN_POINT('Ctrl Pts',(-14.7098797632095,-16.8685283942094,
2.00783333333321));
#34131=CARTESIAN_POINT('Ctrl Pts',(-13.9197595264191,-16.4123522628063,
1.96616666666654));
#34132=CARTESIAN_POINT('Ctrl Pts',(-13.9197595264191,-15.5,1.92449999999988));
#34133=CARTESIAN_POINT('Ctrl Pts',(-13.9197595264191,-14.5876477371938,
1.88283333333321));
#34134=CARTESIAN_POINT('Ctrl Pts',(-14.7098797632095,-14.1314716057907,
1.84116666666654));
#34135=CARTESIAN_POINT('Ctrl Pts',(-15.5,-13.6752954743876,1.79949999999987));
#34136=CARTESIAN_POINT('Ctrl Pts',(-16.2901202367904,-14.1314716057907,
1.75783333333321));
#34137=CARTESIAN_POINT('Ctrl Pts',(-17.0802404735808,-14.5876477371938,
1.71616666666654));
#34138=CARTESIAN_POINT('Ctrl Pts',(-17.0802404735808,-15.5000000000001,
1.67449999999987));
#34139=CARTESIAN_POINT('Ctrl Pts',(-17.0802404735808,-16.4123522628063,
1.63283333333321));
#34140=CARTESIAN_POINT('Ctrl Pts',(-16.2901202367904,-16.8685283942094,
1.59116666666654));
#34141=CARTESIAN_POINT('Ctrl Pts',(-15.4999999999999,-17.3247045256125,
1.54949999999987));
#34142=CARTESIAN_POINT('Ctrl Pts',(-14.7098797632095,-16.8685283942094,
1.5078333333332));
#34143=CARTESIAN_POINT('Ctrl Pts',(-13.9197595264191,-16.4123522628063,
1.46616666666654));
#34144=CARTESIAN_POINT('Ctrl Pts',(-13.9197595264191,-15.5,1.42449999999987));
#34145=CARTESIAN_POINT('Ctrl Pts',(-13.9197595264191,-14.5876477371938,
1.3828333333332));
#34146=CARTESIAN_POINT('Ctrl Pts',(-14.7098797632095,-14.1314716057907,
1.34116666666653));
#34147=CARTESIAN_POINT('Ctrl Pts',(-15.5,-13.6752954743876,1.29949999999987));
#34148=CARTESIAN_POINT('Ctrl Pts',(-16.2901202367904,-14.1314716057907,
1.2578333333332));
#34149=CARTESIAN_POINT('Ctrl Pts',(-17.0802404735808,-14.5876477371938,
1.21616666666653));
#34150=CARTESIAN_POINT('Ctrl Pts',(-17.0802404735808,-15.5000000000001,
1.17449999999986));
#34151=CARTESIAN_POINT('Ctrl Pts',(-17.0802404735808,-16.4123522628063,
1.1328333333332));
#34152=CARTESIAN_POINT('Ctrl Pts',(-16.2901202367904,-16.8685283942094,
1.09116666666653));
#34153=CARTESIAN_POINT('Ctrl Pts',(-15.4999999999999,-17.3247045256125,
1.04949999999986));
#34154=CARTESIAN_POINT('Ctrl Pts',(-14.7098797632095,-16.8685283942094,
1.0078333333332));
#34155=CARTESIAN_POINT('Ctrl Pts',(-13.9197595264191,-16.4123522628063,
0.96616666666653));
#34156=CARTESIAN_POINT('Ctrl Pts',(-13.9197595264191,-15.5,0.924499999999863));
#34157=CARTESIAN_POINT('Ctrl Pts',(-13.9197595264191,-14.5876477371938,
0.882833333333196));
#34158=CARTESIAN_POINT('Ctrl Pts',(-14.7098797632095,-14.1314716057907,
0.841166666666529));
#34159=CARTESIAN_POINT('Ctrl Pts',(-15.5,-13.6752954743876,0.799499999999861));
#34160=CARTESIAN_POINT('Ctrl Pts',(-16.2901202367904,-14.1314716057907,
0.757833333333194));
#34161=CARTESIAN_POINT('Ctrl Pts',(-17.0802404735808,-14.5876477371938,
0.716166666666527));
#34162=CARTESIAN_POINT('Ctrl Pts',(-17.0802404735808,-15.5000000000001,
0.674499999999859));
#34163=CARTESIAN_POINT('Ctrl Pts',(-17.0802404735808,-16.4123522628063,
0.632833333333192));
#34164=CARTESIAN_POINT('Ctrl Pts',(-16.2901202367904,-16.8685283942094,
0.591166666666525));
#34165=CARTESIAN_POINT('Ctrl Pts',(-15.4999999999999,-17.3247045256125,
0.549499999999857));
#34166=CARTESIAN_POINT('Ctrl Pts',(-14.7098797632095,-16.8685283942094,
0.50783333333319));
#34167=CARTESIAN_POINT('Ctrl Pts',(-13.9197595264191,-16.4123522628063,
0.466166666666523));
#34168=CARTESIAN_POINT('Ctrl Pts',(-13.9197595264191,-15.5,0.424499999999856));
#34169=CARTESIAN_POINT('Ctrl Pts',(-13.9197595264191,-14.5876477371938,
0.382833333333188));
#34170=CARTESIAN_POINT('Ctrl Pts',(-14.7098797632095,-14.1314716057907,
0.341166666666521));
#34171=CARTESIAN_POINT('Ctrl Pts',(-15.5,-13.6752954743876,0.299499999999854));
#34172=CARTESIAN_POINT('Ctrl Pts',(-16.2901202367904,-14.1314716057907,
0.257833333333186));
#34173=CARTESIAN_POINT('Ctrl Pts',(-17.0802404735808,-14.5876477371938,
0.216166666666519));
#34174=CARTESIAN_POINT('Ctrl Pts',(-17.0802404735808,-15.5000000000001,
0.174499999999852));
#34175=CARTESIAN_POINT('Ctrl Pts',(-17.0802404735808,-16.4123522628063,
0.132833333333185));
#34176=CARTESIAN_POINT('Ctrl Pts',(-16.2901202367904,-16.8685283942094,
0.0911666666665173));
#34177=CARTESIAN_POINT('Ctrl Pts',(-15.4999999999999,-17.3247045256125,
0.04949999999985));
#34178=CARTESIAN_POINT('Ctrl Pts',(-14.7098797632095,-16.8685283942094,
0.00783333333318273));
#34179=CARTESIAN_POINT('Ctrl Pts',(-13.9197595264191,-16.4123522628063,
-0.0338333333334846));
#34180=CARTESIAN_POINT('Ctrl Pts',(-13.9197595264191,-15.5,-0.0755000000001518));
#34181=CARTESIAN_POINT('Ctrl Pts',(-13.9197595264191,-14.5876477371938,
-0.117166666666817));
#34182=CARTESIAN_POINT('Ctrl Pts',(-14.7098797632095,-14.1314716057907,
-0.158833333333485));
#34183=CARTESIAN_POINT('Ctrl Pts',(-15.5,-13.6752954743876,-0.200500000000152));
#34184=CARTESIAN_POINT('Ctrl Pts',(-16.2901202367904,-14.1314716057907,
-0.242166666666819));
#34185=CARTESIAN_POINT('Ctrl Pts',(-17.0802404735808,-14.5876477371938,
-0.283833333333486));
#34186=CARTESIAN_POINT('Ctrl Pts',(-17.0802404735808,-15.5000000000001,
-0.325500000000154));
#34187=CARTESIAN_POINT('Ctrl Pts',(-17.0802404735808,-16.4123522628063,
-0.367166666666821));
#34188=CARTESIAN_POINT('Ctrl Pts',(-16.2901202367904,-16.8685283942094,
-0.408833333333488));
#34189=CARTESIAN_POINT('Ctrl Pts',(-15.4999999999999,-17.3247045256125,
-0.450500000000156));
#34190=CARTESIAN_POINT('Ctrl Pts',(-14.7098797632095,-16.8685283942094,
-0.492166666666823));
#34191=CARTESIAN_POINT('Ctrl Pts',(-13.9197595264191,-16.4123522628063,
-0.53383333333349));
#34192=CARTESIAN_POINT('Ctrl Pts',(-13.9197595264191,-15.5,-0.575500000000157));
#34193=CARTESIAN_POINT('Ctrl Pts',(-13.9197595264191,-14.5876477371938,
-0.617166666666825));
#34194=CARTESIAN_POINT('Ctrl Pts',(-14.7098797632095,-14.1314716057907,
-0.658833333333492));
#34195=CARTESIAN_POINT('Ctrl Pts',(-15.5,-13.6752954743876,-0.700500000000159));
#34196=CARTESIAN_POINT('Ctrl Pts',(-16.2901202367904,-14.1314716057907,
-0.742166666666827));
#34197=CARTESIAN_POINT('Ctrl Pts',(-17.0802404735808,-14.5876477371938,
-0.783833333333494));
#34198=CARTESIAN_POINT('Ctrl Pts',(-17.0802404735808,-15.5000000000001,
-0.825500000000161));
#34199=CARTESIAN_POINT('Ctrl Pts',(-17.0802404735808,-16.4123522628063,
-0.867166666666829));
#34200=CARTESIAN_POINT('Ctrl Pts',(-16.2901202367904,-16.8685283942094,
-0.908833333333496));
#34201=CARTESIAN_POINT('Ctrl Pts',(-15.4999999999999,-17.3247045256125,
-0.950500000000163));
#34202=CARTESIAN_POINT('Ctrl Pts',(-14.7098797632095,-16.8685283942094,
-0.99216666666683));
#34203=CARTESIAN_POINT('Ctrl Pts',(-13.9197595264191,-16.4123522628063,
-1.0338333333335));
#34204=CARTESIAN_POINT('Ctrl Pts',(-13.9197595264191,-15.5,-1.07550000000016));
#34205=CARTESIAN_POINT('Ctrl Pts',(-13.9197595264191,-14.5876477371938,
-1.11716666666683));
#34206=CARTESIAN_POINT('Ctrl Pts',(-14.7098797632095,-14.1314716057907,
-1.1588333333335));
#34207=CARTESIAN_POINT('Ctrl Pts',(-15.5,-13.6752954743876,-1.20050000000017));
#34208=CARTESIAN_POINT('Ctrl Pts',(-16.2901202367904,-14.1314716057907,
-1.24216666666683));
#34209=CARTESIAN_POINT('Ctrl Pts',(-17.0802404735808,-14.5876477371938,
-1.2838333333335));
#34210=CARTESIAN_POINT('Ctrl Pts',(-17.0802404735808,-15.5000000000001,
-1.32550000000017));
#34211=CARTESIAN_POINT('Ctrl Pts',(-17.0802404735808,-16.4123522628063,
-1.36716666666683));
#34212=CARTESIAN_POINT('Ctrl Pts',(-16.2901202367904,-16.8685283942094,
-1.4088333333335));
#34213=CARTESIAN_POINT('Ctrl Pts',(-15.4999999999999,-17.3247045256125,
-1.45050000000017));
#34214=CARTESIAN_POINT('Ctrl Pts',(-14.7098797632095,-16.8685283942094,
-1.49216666666684));
#34215=CARTESIAN_POINT('Ctrl Pts',(-13.9197595264191,-16.4123522628063,
-1.5338333333335));
#34216=CARTESIAN_POINT('Ctrl Pts',(-13.9197595264191,-15.5,-1.57550000000017));
#34217=CARTESIAN_POINT('Ctrl Pts',(-13.9197595264191,-14.5876477371938,
-1.61716666666684));
#34218=CARTESIAN_POINT('Ctrl Pts',(-14.7098797632095,-14.1314716057907,
-1.65883333333351));
#34219=CARTESIAN_POINT('Ctrl Pts',(-15.5,-13.6752954743876,-1.70050000000017));
#34220=CARTESIAN_POINT('Ctrl Pts',(-16.2901202367904,-14.1314716057907,
-1.74216666666684));
#34221=CARTESIAN_POINT('Ctrl Pts',(-17.0802404735808,-14.5876477371938,
-1.78383333333351));
#34222=CARTESIAN_POINT('Ctrl Pts',(-17.0802404735808,-15.5000000000001,
-1.82550000000017));
#34223=CARTESIAN_POINT('Ctrl Pts',(-17.0802404735808,-16.4123522628063,
-1.86716666666684));
#34224=CARTESIAN_POINT('Ctrl Pts',(-16.2901202367904,-16.8685283942094,
-1.90883333333351));
#34225=CARTESIAN_POINT('Ctrl Pts',(-15.4999999999999,-17.3247045256125,
-1.95050000000018));
#34226=CARTESIAN_POINT('Ctrl Pts',(-14.7098797632095,-16.8685283942094,
-1.99216666666684));
#34227=CARTESIAN_POINT('Ctrl Pts',(-14.4189900731898,-16.7005831533721,
-2.00750661517905));
#34228=CARTESIAN_POINT('Ctrl Pts',(-14.2215586016756,-16.4288420454488,
-2.02512262806106));
#34229=CARTESIAN_POINT('Ctrl Pts',(-13.4352476007234,-15.3465777998746,
-2.09528198318209));
#34230=CARTESIAN_POINT('Ctrl Pts',(-12.6489365997712,-14.2643135543004,
-2.16544133830312));
#34231=CARTESIAN_POINT('Origin',(0.,0.,6.669));
#34232=CARTESIAN_POINT('Origin',(0.,0.,13.019));
#34233=CARTESIAN_POINT('Origin',(-16.96,21.2,10.987));
#34234=CARTESIAN_POINT('',(-21.2,16.96,10.225));
#34235=CARTESIAN_POINT('',(-21.2,16.96,10.987));
#34236=CARTESIAN_POINT('',(-16.96,21.2,10.225));
#34237=CARTESIAN_POINT('',(-16.96,21.2,10.225));
#34238=CARTESIAN_POINT('',(-16.96,21.2,10.987));
#34239=CARTESIAN_POINT('Origin',(-21.2,-16.96,10.987));
#34240=CARTESIAN_POINT('',(-21.2,-16.96,10.225));
#34241=CARTESIAN_POINT('',(-21.2,-16.96,10.987));
#34242=CARTESIAN_POINT('',(-21.2,-16.96,10.225));
#34243=CARTESIAN_POINT('Origin',(-18.5411846327358,18.541184632736,10.225));
#34244=CARTESIAN_POINT('',(-20.438,16.6443692654717,10.987));
#34245=CARTESIAN_POINT('Origin',(-20.4379999999999,16.6443692654717,10.2249999999998));
#34246=CARTESIAN_POINT('',(-16.6443692654717,20.438,10.987));
#34247=CARTESIAN_POINT('',(-18.5411846327358,18.541184632736,10.987));
#34248=CARTESIAN_POINT('Origin',(-16.6443692654718,20.4380000000003,10.2250000000004));
#34249=CARTESIAN_POINT('Origin',(-16.96,21.2,10.987));
#34250=CARTESIAN_POINT('',(16.96,21.2,10.225));
#34251=CARTESIAN_POINT('',(-16.96,21.2,10.225));
#34252=CARTESIAN_POINT('',(16.96,21.2,10.987));
#34253=CARTESIAN_POINT('Origin',(-16.96,-21.2,10.987));
#34254=CARTESIAN_POINT('',(-16.96,-21.2,10.225));
#34255=CARTESIAN_POINT('',(-16.96,-21.2,10.987));
#34256=CARTESIAN_POINT('',(-16.96,-21.2,10.225));
#34257=CARTESIAN_POINT('Origin',(-20.438,-2.09046452842063E-15,10.225));
#34258=CARTESIAN_POINT('',(-20.438,-16.6443692654717,10.987));
#34259=CARTESIAN_POINT('Origin',(-20.4380000000003,-16.6443692654719,10.2250000000003));
#34260=CARTESIAN_POINT('',(-20.438,-2.09046452842063E-15,10.987));
#34261=CARTESIAN_POINT('Origin',(16.96,-21.2,10.987));
#34262=CARTESIAN_POINT('',(16.96,-21.2,10.225));
#34263=CARTESIAN_POINT('',(16.96,-21.2,10.987));
#34264=CARTESIAN_POINT('',(16.96,-21.2,10.225));
#34265=CARTESIAN_POINT('Origin',(-18.5411846327358,-18.541184632736,10.225));
#34266=CARTESIAN_POINT('',(-16.6443692654717,-20.438,10.987));
#34267=CARTESIAN_POINT('Origin',(-16.6443692654716,-20.4379999999998,10.2249999999998));
#34268=CARTESIAN_POINT('',(-18.5411846327358,-18.541184632736,10.987));
#34269=CARTESIAN_POINT('Origin',(16.96,-21.2,10.987));
#34270=CARTESIAN_POINT('',(21.2,-16.96,10.225));
#34271=CARTESIAN_POINT('',(21.2,-16.96,10.987));
#34272=CARTESIAN_POINT('',(16.96,-21.2,10.225));
#34273=CARTESIAN_POINT('Origin',(4.18092905684127E-15,-20.438,10.225));
#34274=CARTESIAN_POINT('',(16.6443692654717,-20.438,10.987));
#34275=CARTESIAN_POINT('Origin',(16.6443692654717,-20.4380000000001,10.2250000000001));
#34276=CARTESIAN_POINT('',(4.18092905684127E-15,-20.438,10.987));
#34277=CARTESIAN_POINT('Origin',(21.2,16.96,10.987));
#34278=CARTESIAN_POINT('',(21.2,16.96,10.225));
#34279=CARTESIAN_POINT('',(21.2,16.96,10.987));
#34280=CARTESIAN_POINT('',(21.2,16.96,10.225));
#34281=CARTESIAN_POINT('Origin',(18.5411846327358,-18.541184632736,10.225));
#34282=CARTESIAN_POINT('',(20.438,-16.6443692654717,10.987));
#34283=CARTESIAN_POINT('Origin',(20.4380000000001,-16.6443692654718,10.2250000000002));
#34284=CARTESIAN_POINT('',(18.5411846327358,-18.541184632736,10.987));
#34285=CARTESIAN_POINT('Origin',(16.96,21.2,10.987));
#34286=CARTESIAN_POINT('',(16.96,21.2,10.225));
#34287=CARTESIAN_POINT('Origin',(20.438,0.,10.225));
#34288=CARTESIAN_POINT('',(20.438,16.6443692654717,10.987));
#34289=CARTESIAN_POINT('Origin',(20.4380000000004,16.6443692654719,10.2250000000004));
#34290=CARTESIAN_POINT('',(20.438,0.,10.987));
#34291=CARTESIAN_POINT('Origin',(18.5411846327358,18.541184632736,10.225));
#34292=CARTESIAN_POINT('',(16.6443692654717,20.438,10.987));
#34293=CARTESIAN_POINT('Origin',(16.6443692654718,20.4380000000003,10.2250000000003));
#34294=CARTESIAN_POINT('',(18.5411846327358,18.541184632736,10.987));
#34295=CARTESIAN_POINT('Origin',(0.,20.438,10.225));
#34296=CARTESIAN_POINT('',(0.,20.438,10.987));
#34297=CARTESIAN_POINT('Origin',(0.,0.,10.987));
#34298=CARTESIAN_POINT('Origin',(0.,0.,37.019));
#34299=CARTESIAN_POINT('',(2.50000000000186,-3.06161699787066E-16,36.5109999999982));
#34300=CARTESIAN_POINT('',(1.99199999999996,-2.43949642390148E-16,37.0190000000001));
#34301=CARTESIAN_POINT('',(1.99200000000004,-2.43949642390158E-16,37.019));
#34302=CARTESIAN_POINT('',(1.51060782468515,1.99199999999999,36.511));
#34303=CARTESIAN_POINT('Origin',(0.,0.,36.511));
#34304=CARTESIAN_POINT('',(0.,1.99200000000004,37.019));
#34305=CARTESIAN_POINT('Ctrl Pts',(2.79900555615041E-16,1.99199999999998,
37.0190000000001));
#34306=CARTESIAN_POINT('Ctrl Pts',(0.669886639976148,1.99199999999998,37.0190000000001));
#34307=CARTESIAN_POINT('Ctrl Pts',(1.51060782468516,1.99199999999998,36.5110000000001));
#34308=CARTESIAN_POINT('Origin',(0.,0.,37.019));
#34309=CARTESIAN_POINT('Origin',(0.,0.,37.019));
#34310=CARTESIAN_POINT('Origin',(0.,0.,37.019));
#34311=CARTESIAN_POINT('',(-1.51060782468517,1.99199999999999,36.511));
#34312=CARTESIAN_POINT('Ctrl Pts',(-1.51060782468828,1.99199999999998,36.5109999999982));
#34313=CARTESIAN_POINT('Ctrl Pts',(-0.669886639977248,1.99199999999998,
37.0190000000001));
#34314=CARTESIAN_POINT('Ctrl Pts',(2.79900555615041E-16,1.99199999999998,
37.0190000000001));
#34315=CARTESIAN_POINT('Origin',(0.,0.,36.511));
#34316=CARTESIAN_POINT('Origin',(0.,0.,37.019));
#34317=CARTESIAN_POINT('',(0.,0.,36.043));
#34318=CARTESIAN_POINT('',(-0.975999999999995,1.19525527596781E-16,37.019));
#34319=CARTESIAN_POINT('',(-0.975999999999995,-1.19525527596781E-16,37.019));
#34320=CARTESIAN_POINT('Origin',(0.,0.,37.019));
#34321=CARTESIAN_POINT('Origin',(0.,0.,37.019));
#34322=CARTESIAN_POINT('',(2.5,-3.06161699786838E-16,-31.939));
#34323=CARTESIAN_POINT('Origin',(0.,0.,-31.939));
#34324=CARTESIAN_POINT('',(2.5,-3.06161699786838E-16,37.019));
#34325=CARTESIAN_POINT('',(-1.51060782468515,1.99199999999999,16.719));
#34326=CARTESIAN_POINT('',(-1.51060782468515,1.99199999999999,37.019));
#34327=CARTESIAN_POINT('',(1.51060782468515,1.99199999999999,16.719));
#34328=CARTESIAN_POINT('Origin',(0.,0.,16.719));
#34329=CARTESIAN_POINT('',(1.51060782468515,1.99199999999999,37.019));
#34330=CARTESIAN_POINT('Origin',(0.,0.,37.019));
#34331=CARTESIAN_POINT('Origin',(0.,0.,-31.939));
#34332=CARTESIAN_POINT('Origin',(-21.2,3.008,16.719));
#34333=CARTESIAN_POINT('',(-21.2,1.99199999999999,16.719));
#34334=CARTESIAN_POINT('Origin',(-21.2,1.99199999999999,37.019));
#34335=CARTESIAN_POINT('Origin',(0.,0.,-32.574));
#34336=CARTESIAN_POINT('',(5.16699999999999,-6.32775001119437E-16,-32.574));
#34337=CARTESIAN_POINT('Origin',(0.,0.,-32.574));
#34338=CARTESIAN_POINT('',(5.16699999999999,-6.32775001119437E-16,-37.019));
#34339=CARTESIAN_POINT('',(5.16699999999999,-6.32775001119436E-16,-32.574));
#34340=CARTESIAN_POINT('Origin',(0.,0.,-37.019));
#34341=CARTESIAN_POINT('Origin',(-15.5,-15.5,-36.765));
#34342=CARTESIAN_POINT('',(-12.325,-15.5,-36.765));
#34343=CARTESIAN_POINT('Origin',(-15.5,-15.5,-36.765));
#34344=CARTESIAN_POINT('',(-12.071,-15.5,-37.019));
#34345=CARTESIAN_POINT('',(-12.325,-15.5,-36.765));
#34346=CARTESIAN_POINT('Origin',(-15.5,-15.5,-37.019));
#34347=CARTESIAN_POINT('Origin',(15.5,-15.5,-36.765));
#34348=CARTESIAN_POINT('',(18.675,-15.5,-36.765));
#34349=CARTESIAN_POINT('Origin',(15.5,-15.5,-36.765));
#34350=CARTESIAN_POINT('',(18.929,-15.5,-37.019));
#34351=CARTESIAN_POINT('',(18.675,-15.5,-36.765));
#34352=CARTESIAN_POINT('Origin',(15.5,-15.5,-37.019));
#34353=CARTESIAN_POINT('Origin',(15.5,15.5,-36.765));
#34354=CARTESIAN_POINT('',(18.675,15.5,-36.765));
#34355=CARTESIAN_POINT('Origin',(15.5,15.5,-36.765));
#34356=CARTESIAN_POINT('',(18.929,15.5,-37.019));
#34357=CARTESIAN_POINT('',(18.675,15.5,-36.765));
#34358=CARTESIAN_POINT('Origin',(15.5,15.5,-37.019));
#34359=CARTESIAN_POINT('Origin',(-15.5,15.5,-36.765));
#34360=CARTESIAN_POINT('',(-12.325,15.5,-36.765));
#34361=CARTESIAN_POINT('Origin',(-15.5,15.5,-36.765));
#34362=CARTESIAN_POINT('',(-12.071,15.5,-37.019));
#34363=CARTESIAN_POINT('',(-12.325,15.5,-36.765));
#34364=CARTESIAN_POINT('Origin',(-15.5,15.5,-37.019));
#34365=CARTESIAN_POINT('Origin',(-15.5,-15.5,-33.844));
#34366=CARTESIAN_POINT('',(-12.325,-15.5,-33.844));
#34367=CARTESIAN_POINT('Origin',(-15.5,-15.5,-33.844));
#34368=CARTESIAN_POINT('',(-12.325,-15.5,-33.844));
#34369=CARTESIAN_POINT('Origin',(15.5,-15.5,-33.844));
#34370=CARTESIAN_POINT('',(18.675,-15.5,-33.844));
#34371=CARTESIAN_POINT('Origin',(15.5,-15.5,-33.844));
#34372=CARTESIAN_POINT('',(18.675,-15.5,-33.844));
#34373=CARTESIAN_POINT('Origin',(15.5,15.5,-33.844));
#34374=CARTESIAN_POINT('',(18.675,15.5,-33.844));
#34375=CARTESIAN_POINT('Origin',(15.5,15.5,-33.844));
#34376=CARTESIAN_POINT('',(18.675,15.5,-33.844));
#34377=CARTESIAN_POINT('Origin',(-15.5,15.5,-33.844));
#34378=CARTESIAN_POINT('',(-12.325,15.5,-33.844));
#34379=CARTESIAN_POINT('Origin',(-15.5,15.5,-33.844));
#34380=CARTESIAN_POINT('',(-12.325,15.5,-33.844));
#34381=CARTESIAN_POINT('Origin',(0.,0.,-37.019));
#34382=CARTESIAN_POINT('',(-2.62699999999999,-3.21714714136009E-16,-32.574));
#34383=CARTESIAN_POINT('Origin',(0.,0.,-32.574));
#34384=CARTESIAN_POINT('',(-2.62699999999999,-3.21714714136009E-16,-27.4178));
#34385=CARTESIAN_POINT('',(-2.62699999999999,-3.21714714136008E-16,-37.019));
#34386=CARTESIAN_POINT('Origin',(0.,0.,-27.4178));
#34387=CARTESIAN_POINT('Origin',(-15.5,15.5,-33.844));
#34388=CARTESIAN_POINT('Origin',(15.5,15.5,-33.844));
#34389=CARTESIAN_POINT('Origin',(15.5,-15.5,-33.844));
#34390=CARTESIAN_POINT('Origin',(-15.5,-15.5,-33.844));
#34391=CARTESIAN_POINT('Origin',(0.,14.342,0.));
#34392=CARTESIAN_POINT('',(-4.445,14.342,-28.9418));
#34393=CARTESIAN_POINT('',(4.445,14.342,-28.9418));
#34394=CARTESIAN_POINT('',(-4.445,14.342,-28.9418));
#34395=CARTESIAN_POINT('',(4.445,14.342,-35.495));
#34396=CARTESIAN_POINT('',(4.445,14.342,-28.9418));
#34397=CARTESIAN_POINT('',(-4.445,14.342,-35.495));
#34398=CARTESIAN_POINT('',(4.445,14.342,-35.495));
#34399=CARTESIAN_POINT('',(-4.445,14.342,-35.495));
#34400=CARTESIAN_POINT('Origin',(4.445,14.342,-35.495));
#34401=CARTESIAN_POINT('',(4.445,21.962,-35.495));
#34402=CARTESIAN_POINT('',(-4.445,21.962,-35.495));
#34403=CARTESIAN_POINT('',(4.445,21.962,-35.495));
#34404=CARTESIAN_POINT('',(-4.445,14.342,-35.495));
#34405=CARTESIAN_POINT('',(4.445,14.342,-35.495));
#34406=CARTESIAN_POINT('Origin',(-4.445,14.342,-35.495));
#34407=CARTESIAN_POINT('',(-4.445,21.962,-28.9418));
#34408=CARTESIAN_POINT('',(-4.445,21.962,-35.495));
#34409=CARTESIAN_POINT('',(-4.445,14.342,-28.9418));
#34410=CARTESIAN_POINT('Origin',(-4.445,14.342,-28.9418));
#34411=CARTESIAN_POINT('',(4.445,21.962,-28.9418));
#34412=CARTESIAN_POINT('',(-4.445,21.962,-28.9418));
#34413=CARTESIAN_POINT('',(4.445,14.342,-28.9418));
#34414=CARTESIAN_POINT('Origin',(4.445,14.342,-28.9418));
#34415=CARTESIAN_POINT('',(4.445,21.962,-28.9418));
#34416=CARTESIAN_POINT('Origin',(0.,21.962,0.));
#34417=CARTESIAN_POINT('',(5.715,21.962,-27.6718));
#34418=CARTESIAN_POINT('',(5.715,21.962,-36.765));
#34419=CARTESIAN_POINT('',(5.715,21.962,-27.6718));
#34420=CARTESIAN_POINT('',(-5.715,21.962,-36.765));
#34421=CARTESIAN_POINT('',(-5.715,21.962,-36.765));
#34422=CARTESIAN_POINT('',(-5.715,21.962,-27.6718));
#34423=CARTESIAN_POINT('',(-5.715,21.962,-27.6718));
#34424=CARTESIAN_POINT('',(-5.715,21.962,-27.6718));
#34425=CARTESIAN_POINT('Origin',(-5.715,21.962,-36.765));
#34426=CARTESIAN_POINT('',(5.715,21.0059612662849,-36.765));
#34427=CARTESIAN_POINT('',(5.715,21.962,-36.765));
#34428=CARTESIAN_POINT('',(-5.715,21.0059612662849,-36.765));
#34429=CARTESIAN_POINT('',(5.715,21.0059612662849,-36.765));
#34430=CARTESIAN_POINT('',(-5.715,21.962,-36.765));
#34431=CARTESIAN_POINT('Origin',(0.,0.,-37.019));
#34432=CARTESIAN_POINT('',(16.6443692654717,-20.438,-37.019));
#34433=CARTESIAN_POINT('',(-16.6443692654717,-20.438,-37.019));
#34434=CARTESIAN_POINT('',(-16.96,-20.438,-37.019));
#34435=CARTESIAN_POINT('',(-20.438,-16.6443692654717,-37.019));
#34436=CARTESIAN_POINT('',(-20.6611846327359,-16.4211846327359,-37.019));
#34437=CARTESIAN_POINT('',(-20.438,16.6443692654717,-37.019));
#34438=CARTESIAN_POINT('',(-20.438,16.96,-37.019));
#34439=CARTESIAN_POINT('',(-16.6443692654717,20.438,-37.019));
#34440=CARTESIAN_POINT('',(-16.4211846327359,20.6611846327359,-37.019));
#34441=CARTESIAN_POINT('',(16.6443692654717,20.438,-37.019));
#34442=CARTESIAN_POINT('',(16.96,20.438,-37.019));
#34443=CARTESIAN_POINT('',(20.438,16.6443692654717,-37.019));
#34444=CARTESIAN_POINT('',(20.6611846327359,16.4211846327359,-37.019));
#34445=CARTESIAN_POINT('',(20.438,-16.6443692654717,-37.019));
#34446=CARTESIAN_POINT('',(20.438,-16.96,-37.019));
#34447=CARTESIAN_POINT('',(16.4211846327359,-20.6611846327358,-37.019));
#34448=CARTESIAN_POINT('Origin',(-16.4211846327359,20.6611846327359,-36.257));
#34449=CARTESIAN_POINT('',(-16.96,21.2,-36.257));
#34450=CARTESIAN_POINT('Origin',(-16.6443692654719,20.4380000000006,-36.2570000000005));
#34451=CARTESIAN_POINT('',(-21.2,16.96,-36.257));
#34452=CARTESIAN_POINT('Origin',(-20.4380000000008,16.6443692654721,-36.2570000000008));
#34453=CARTESIAN_POINT('',(-21.2,16.96,-36.257));
#34454=CARTESIAN_POINT('Origin',(-20.438,-16.96,-36.257));
#34455=CARTESIAN_POINT('',(-21.2,-16.96,-36.257));
#34456=CARTESIAN_POINT('Origin',(-20.4380000000006,-16.644369265472,-36.2570000000005));
#34457=CARTESIAN_POINT('',(-21.2,-16.96,-36.257));
#34458=CARTESIAN_POINT('Origin',(-16.4211846327358,-20.6611846327359,-36.257));
#34459=CARTESIAN_POINT('',(-16.96,-21.2,-36.257));
#34460=CARTESIAN_POINT('Origin',(-16.6443692654721,-20.4380000000011,-36.257000000001));
#34461=CARTESIAN_POINT('',(-16.96,-21.2,-36.257));
#34462=CARTESIAN_POINT('Origin',(-21.2,-16.96,10.987));
#34463=CARTESIAN_POINT('',(-21.2,16.96,-27.4178));
#34464=CARTESIAN_POINT('',(-21.2,16.96,10.987));
#34465=CARTESIAN_POINT('',(-21.2,-16.96,-27.4178));
#34466=CARTESIAN_POINT('',(-21.2,-16.96,10.987));
#34467=CARTESIAN_POINT('',(-21.2,21.2,-27.4178));
#34468=CARTESIAN_POINT('Origin',(16.96,-20.438,-36.257));
#34469=CARTESIAN_POINT('',(16.96,-21.2,-36.257));
#34470=CARTESIAN_POINT('Origin',(16.6443692654718,-20.4380000000002,-36.2570000000002));
#34471=CARTESIAN_POINT('',(16.96,-21.2,-36.257));
#34472=CARTESIAN_POINT('Origin',(-16.96,-21.2,10.987));
#34473=CARTESIAN_POINT('',(-16.96,-21.2,-27.4178));
#34474=CARTESIAN_POINT('',(-16.96,-21.2,10.987));
#34475=CARTESIAN_POINT('',(-16.96,-21.2,-27.4178));
#34476=CARTESIAN_POINT('Origin',(16.4211846327359,-20.6611846327358,-36.257));
#34477=CARTESIAN_POINT('',(21.2,-16.96,-36.257));
#34478=CARTESIAN_POINT('Origin',(20.4380000000003,-16.6443692654718,-36.2570000000003));
#34479=CARTESIAN_POINT('',(21.2,-16.96,-36.257));
#34480=CARTESIAN_POINT('Origin',(16.96,-21.2,10.987));
#34481=CARTESIAN_POINT('',(16.96,-21.2,-27.4178));
#34482=CARTESIAN_POINT('',(16.96,-21.2,10.987));
#34483=CARTESIAN_POINT('',(-21.2,-21.2,-27.4178));
#34484=CARTESIAN_POINT('Origin',(20.438,16.96,-36.257));
#34485=CARTESIAN_POINT('',(21.2,16.96,-36.257));
#34486=CARTESIAN_POINT('Origin',(20.4379999999998,16.6443692654717,-36.2569999999998));
#34487=CARTESIAN_POINT('',(21.2,16.96,-36.257));
#34488=CARTESIAN_POINT('Origin',(16.96,-21.2,10.987));
#34489=CARTESIAN_POINT('',(21.2,-16.96,-27.4178));
#34490=CARTESIAN_POINT('',(21.2,-16.96,10.987));
#34491=CARTESIAN_POINT('',(16.96,-21.2,-27.4178));
#34492=CARTESIAN_POINT('Origin',(16.4211846327359,20.6611846327359,-36.257));
#34493=CARTESIAN_POINT('',(16.96,21.2,-36.257));
#34494=CARTESIAN_POINT('Origin',(16.6443692654716,20.4379999999997,-36.2569999999998));
#34495=CARTESIAN_POINT('',(16.96,21.2,-36.257));
#34496=CARTESIAN_POINT('Origin',(21.2,16.96,10.987));
#34497=CARTESIAN_POINT('',(21.2,16.96,-27.4178));
#34498=CARTESIAN_POINT('',(21.2,16.96,10.987));
#34499=CARTESIAN_POINT('',(21.2,21.2,-27.4178));
#34500=CARTESIAN_POINT('Origin',(-16.96,21.2,10.987));
#34501=CARTESIAN_POINT('',(-16.96,21.2,-27.4178));
#34502=CARTESIAN_POINT('',(-16.96,21.2,10.987));
#34503=CARTESIAN_POINT('',(-16.96,21.2,-27.4178));
#34504=CARTESIAN_POINT('Origin',(-5.715,21.962,-27.6718));
#34505=CARTESIAN_POINT('',(-5.715,21.2,-36.257));
#34506=CARTESIAN_POINT('Origin',(-5.715,20.438,-36.257));
#34507=CARTESIAN_POINT('',(-5.715,21.2,-27.6718));
#34508=CARTESIAN_POINT('',(-5.715,21.2,-27.6718));
#34509=CARTESIAN_POINT('',(-5.715,21.962,-27.6718));
#34510=CARTESIAN_POINT('Origin',(-5.715,21.962,-27.6718));
#34511=CARTESIAN_POINT('',(5.715,21.2,-27.6718));
#34512=CARTESIAN_POINT('',(-5.715,21.2,-27.6718));
#34513=CARTESIAN_POINT('',(5.715,21.962,-27.6718));
#34514=CARTESIAN_POINT('Origin',(5.715,21.962,-27.6718));
#34515=CARTESIAN_POINT('',(5.715,21.2,-36.257));
#34516=CARTESIAN_POINT('',(5.715,21.2,-27.6718));
#34517=CARTESIAN_POINT('Origin',(5.715,20.438,-36.257));
#34518=CARTESIAN_POINT('Origin',(-16.96,20.438,-36.257));
#34519=CARTESIAN_POINT('',(-16.96,21.2,-36.257));
#34520=CARTESIAN_POINT('',(-16.96,21.2,-36.257));
#34521=CARTESIAN_POINT('Origin',(16.96,21.2,10.987));
#34522=CARTESIAN_POINT('',(16.96,21.2,-27.4178));
#34523=CARTESIAN_POINT('',(16.96,21.2,10.987));
#34524=CARTESIAN_POINT('',(16.96,21.2,-27.4178));
#34525=CARTESIAN_POINT('Origin',(-16.96,21.2,10.987));
#34526=CARTESIAN_POINT('',(-21.2,21.2,-27.4178));
#34527=CARTESIAN_POINT('Origin',(-21.2,16.96,-27.4178));
#34528=CARTESIAN_POINT('Origin',(0.,0.,-32.574));
#34529=CARTESIAN_POINT('Origin',(0.,0.,-37.019));
#34530=CARTESIAN_POINT('',(-2.62699999999999,-3.21714714136009E-16,-27.4178));
#34531=CARTESIAN_POINT('Origin',(0.,0.,-27.4178));
#34532=CARTESIAN_POINT('',(-2.62699999999999,-3.21714714136009E-16,1.3858));
#34533=CARTESIAN_POINT('',(-2.62699999999999,-3.21714714136008E-16,-37.019));
#34534=CARTESIAN_POINT('Origin',(0.,0.,1.3858));
#34535=CARTESIAN_POINT('Origin',(15.5,-15.5,-1.713));
#34536=CARTESIAN_POINT('',(13.595,-15.5,-1.713));
#34537=CARTESIAN_POINT('Origin',(15.5,-15.5,-1.713));
#34538=CARTESIAN_POINT('',(13.595,-15.5,1.3858));
#34539=CARTESIAN_POINT('',(13.595,-15.5,-1.713));
#34540=CARTESIAN_POINT('Origin',(15.5,-15.5,1.3858));
#34541=CARTESIAN_POINT('Origin',(-15.5,15.5,-1.713));
#34542=CARTESIAN_POINT('',(-17.405,15.5,-1.713));
#34543=CARTESIAN_POINT('Origin',(-15.5,15.5,-1.713));
#34544=CARTESIAN_POINT('',(-17.405,15.5,1.3858));
#34545=CARTESIAN_POINT('',(-17.405,15.5,-1.713));
#34546=CARTESIAN_POINT('Origin',(-15.5,15.5,1.3858));
#34547=CARTESIAN_POINT('Origin',(15.5,15.5,-1.713));
#34548=CARTESIAN_POINT('',(13.595,15.5,-1.713));
#34549=CARTESIAN_POINT('Origin',(15.5,15.5,-1.713));
#34550=CARTESIAN_POINT('',(13.595,15.5,1.3858));
#34551=CARTESIAN_POINT('',(13.595,15.5,-1.713));
#34552=CARTESIAN_POINT('Origin',(15.5,15.5,1.3858));
#34553=CARTESIAN_POINT('Origin',(-15.5,-15.5,-1.713));
#34554=CARTESIAN_POINT('',(-17.405,-15.5,-1.713));
#34555=CARTESIAN_POINT('Origin',(-15.5,-15.5,-1.713));
#34556=CARTESIAN_POINT('',(-17.405,-15.5,1.3858));
#34557=CARTESIAN_POINT('',(-17.405,-15.5,-1.713));
#34558=CARTESIAN_POINT('Origin',(-15.5,-15.5,1.3858));
#34559=CARTESIAN_POINT('Origin',(-21.2,16.96,-27.4178));
#34560=CARTESIAN_POINT('',(14.5199231636792,20.946,-27.4178));
#34561=CARTESIAN_POINT('',(20.946,14.5199231636793,-27.4178));
#34562=CARTESIAN_POINT('',(15.6129615818396,19.8529615818396,-27.4178));
#34563=CARTESIAN_POINT('',(20.946,-14.5199231636793,-27.4178));
#34564=CARTESIAN_POINT('',(20.946,14.5199231636793,-27.4178));
#34565=CARTESIAN_POINT('',(14.5199231636792,-20.946,-27.4178));
#34566=CARTESIAN_POINT('',(20.946,-14.5199231636793,-27.4178));
#34567=CARTESIAN_POINT('',(-14.5199231636792,-20.946,-27.4178));
#34568=CARTESIAN_POINT('',(-14.5199231636792,-20.946,-27.4178));
#34569=CARTESIAN_POINT('',(-20.946,-14.5199231636793,-27.4178));
#34570=CARTESIAN_POINT('',(-15.6129615818396,-19.8529615818396,-27.4178));
#34571=CARTESIAN_POINT('',(-20.946,14.5199231636793,-27.4178));
#34572=CARTESIAN_POINT('',(-20.946,14.5199231636793,-27.4178));
#34573=CARTESIAN_POINT('',(-14.5199231636792,20.946,-27.4178));
#34574=CARTESIAN_POINT('',(-15.6129615818396,19.8529615818396,-27.4178));
#34575=CARTESIAN_POINT('',(-14.5199231636792,20.946,-27.4178));
#34576=CARTESIAN_POINT('Origin',(16.96,21.2,1.3858));
#34577=CARTESIAN_POINT('',(14.5199231636792,20.946,1.3858));
#34578=CARTESIAN_POINT('',(20.946,14.5199231636793,1.3858));
#34579=CARTESIAN_POINT('',(20.946,14.5199231636793,1.3858));
#34580=CARTESIAN_POINT('',(-14.5199231636792,20.946,1.3858));
#34581=CARTESIAN_POINT('',(-14.5199231636792,20.946,1.3858));
#34582=CARTESIAN_POINT('',(-20.946,14.5199231636793,1.3858));
#34583=CARTESIAN_POINT('',(-15.6129615818396,19.8529615818396,1.3858));
#34584=CARTESIAN_POINT('',(-20.946,-14.5199231636793,1.3858));
#34585=CARTESIAN_POINT('',(-20.946,14.5199231636793,1.3858));
#34586=CARTESIAN_POINT('',(-14.5199231636792,-20.946,1.3858));
#34587=CARTESIAN_POINT('',(-20.946,-14.5199231636793,1.3858));
#34588=CARTESIAN_POINT('',(14.5199231636792,-20.946,1.3858));
#34589=CARTESIAN_POINT('',(-14.5199231636792,-20.946,1.3858));
#34590=CARTESIAN_POINT('',(20.946,-14.5199231636793,1.3858));
#34591=CARTESIAN_POINT('',(15.6129615818396,-19.8529615818396,1.3858));
#34592=CARTESIAN_POINT('',(20.946,14.5199231636793,1.3858));
#34593=CARTESIAN_POINT('Origin',(-14.5199231636792,20.946,-27.4178));
#34594=CARTESIAN_POINT('',(14.5199231636792,20.946,-27.4178));
#34595=CARTESIAN_POINT('',(-14.5199231636792,20.946,-27.4178));
#34596=CARTESIAN_POINT('Origin',(20.946,14.5199231636793,-27.4178));
#34597=CARTESIAN_POINT('',(20.946,14.5199231636793,-27.4178));
#34598=CARTESIAN_POINT('Origin',(-15.6129615818396,19.8529615818396,-27.4178));
#34599=CARTESIAN_POINT('',(-20.946,14.5199231636793,-27.4178));
#34600=CARTESIAN_POINT('Origin',(15.6129615818396,-19.8529615818396,-27.4178));
#34601=CARTESIAN_POINT('',(14.5199231636792,-20.946,-27.4178));
#34602=CARTESIAN_POINT('',(20.946,-14.5199231636793,-27.4178));
#34603=CARTESIAN_POINT('Origin',(-20.946,-14.5199231636793,-27.4178));
#34604=CARTESIAN_POINT('',(-20.946,-14.5199231636793,-27.4178));
#34605=CARTESIAN_POINT('',(-14.5199231636792,-20.946,-27.4178));
#34606=CARTESIAN_POINT('Origin',(-20.946,14.5199231636793,-27.4178));
#34607=CARTESIAN_POINT('Origin',(-14.5199231636792,-20.946,-27.4178));
#34608=CARTESIAN_POINT('Origin',(20.946,14.5199231636793,-27.4178));
#34609=CARTESIAN_POINT('Origin',(15.5,-15.5,-1.713));
#34610=CARTESIAN_POINT('Origin',(-15.5,15.5,-1.713));
#34611=CARTESIAN_POINT('Origin',(15.5,15.5,-1.713));
#34612=CARTESIAN_POINT('Origin',(-15.5,-15.5,-1.713));
#34613=CARTESIAN_POINT('',(0.,0.,0.));
#34614=CARTESIAN_POINT('',(0.,0.,0.));
#34615=CARTESIAN_POINT('Origin',(-6.,190.828431883169,20.8299327490105));
#34616=CARTESIAN_POINT('',(-7.,202.778931883169,20.8299327490105));
#34617=CARTESIAN_POINT('Origin',(-7.,190.828431883169,20.8299327490105));
#34618=CARTESIAN_POINT('',(-5.,200.778931883169,20.8299327490105));
#34619=CARTESIAN_POINT('',(-6.,201.778931883169,20.8299327490105));
#34620=CARTESIAN_POINT('Origin',(-5.,190.828431883169,20.8299327490105));
#34621=CARTESIAN_POINT('Origin',(-10.,190.828431883169,20.8299327490105));
#34622=CARTESIAN_POINT('',(-13.,202.778931883169,20.8299327490105));
#34623=CARTESIAN_POINT('Origin',(-13.,190.828431883169,20.8299327490105));
#34624=CARTESIAN_POINT('',(-10.,202.778931883169,20.8299327490105));
#34625=CARTESIAN_POINT('Origin',(-5.,190.828431883169,20.8299327490105));
#34626=CARTESIAN_POINT('',(-5.,198.828431883169,20.8299327490105));
#34627=CARTESIAN_POINT('Origin',(-5.,190.828431883169,20.8299327490105));
#34628=CARTESIAN_POINT('Origin',(-14.,190.828431883169,20.8299327490105));
#34629=CARTESIAN_POINT('',(-15.,200.778931883169,20.8299327490105));
#34630=CARTESIAN_POINT('',(-14.,201.778931883169,20.8299327490105));
#34631=CARTESIAN_POINT('Origin',(-15.,190.828431883169,20.8299327490105));
#34632=CARTESIAN_POINT('Origin',(-15.,190.828431883169,20.8299327490105));
#34633=CARTESIAN_POINT('',(-15.,198.828431883169,20.8299327490105));
#34634=CARTESIAN_POINT('Origin',(-15.,190.828431883169,20.8299327490105));
#34635=CARTESIAN_POINT('Origin',(-10.,190.828431883169,20.8299327490105));
#34636=CARTESIAN_POINT('',(-10.,198.828431883169,20.8299327490105));
#34637=CARTESIAN_POINT('',(0.,0.,0.));
#34638=CARTESIAN_POINT('Origin',(-22.5,190.828431883169,20.8299327490105));
#34639=CARTESIAN_POINT('',(-22.5,188.328431883169,20.8299327490105));
#34640=CARTESIAN_POINT('Origin',(-22.5,190.828431883169,20.8299327490105));
#34641=CARTESIAN_POINT('',(-14.95,188.328431883169,20.8299327490105));
#34642=CARTESIAN_POINT('',(-22.5,188.328431883169,20.8299327490105));
#34643=CARTESIAN_POINT('Origin',(-14.95,190.828431883169,20.8299327490105));
#34644=CARTESIAN_POINT('Origin',(-22.5,190.828431883169,20.8299327490105));
#34645=CARTESIAN_POINT('',(-14.95,186.328431883169,20.8299327490105));
#34646=CARTESIAN_POINT('Origin',(-14.95,190.828431883169,20.8299327490105));
#34647=CARTESIAN_POINT('',(-22.5,186.328431883169,20.8299327490105));
#34648=CARTESIAN_POINT('',(-22.5,186.328431883169,20.8299327490105));
#34649=CARTESIAN_POINT('Origin',(-22.5,190.828431883169,20.8299327490105));
#34650=CARTESIAN_POINT('Origin',(-14.95,190.828431883169,20.8299327490105));
#34651=CARTESIAN_POINT('Origin',(-22.5,190.828431883169,20.8299327490105));
#34652=CARTESIAN_POINT('',(0.,0.,0.));
#34653=CARTESIAN_POINT('Origin',(0.,0.,0.675));
#34654=CARTESIAN_POINT('',(2.117,-2.59257727379495E-16,0.663375459298879));
#34655=CARTESIAN_POINT('Origin',(0.,0.,0.663375459298879));
#34656=CARTESIAN_POINT('',(2.5,-3.06161699786838E-16,-2.77555756156289E-16));
#34657=CARTESIAN_POINT('',(2.110288568297,-2.58435814044217E-16,0.675));
#34658=CARTESIAN_POINT('Origin',(0.,0.,0.));
#34659=CARTESIAN_POINT('Origin',(0.,0.,2.025));
#34660=CARTESIAN_POINT('',(2.117,2.59257727379495E-16,2.03662454070112));
#34661=CARTESIAN_POINT('Origin',(0.,0.,2.03662454070112));
#34662=CARTESIAN_POINT('',(2.5,-3.06161699786838E-16,2.7));
#34663=CARTESIAN_POINT('',(2.110288568297,2.58435814044217E-16,2.025));
#34664=CARTESIAN_POINT('Origin',(0.,0.,2.7));
#34665=CARTESIAN_POINT('Origin',(0.00207392470908813,4.61999953450607,2.7));
#34666=CARTESIAN_POINT('',(6.47240898139264E-15,4.618802153517,0.403453611443332));
#34667=CARTESIAN_POINT('',(6.40757044047557E-15,4.618802153517,2.29654638855667));
#34668=CARTESIAN_POINT('',(6.38378239159465E-15,4.618802153517,2.7));
#34669=CARTESIAN_POINT('',(-4.,2.30940107675851,0.403453611443333));
#34670=CARTESIAN_POINT('Ctrl Pts',(-4.,2.30940107675851,0.403453611443333));
#34671=CARTESIAN_POINT('Ctrl Pts',(-2.,3.46410161513776,-0.263213055223336));
#34672=CARTESIAN_POINT('Ctrl Pts',(6.47240898139264E-15,4.618802153517,
0.403453611443332));
#34673=CARTESIAN_POINT('',(-4.,2.30940107675851,2.29654638855667));
#34674=CARTESIAN_POINT('',(-4.,2.30940107675851,2.7));
#34675=CARTESIAN_POINT('Ctrl Pts',(6.40757044047557E-15,4.618802153517,
2.29654638855667));
#34676=CARTESIAN_POINT('Ctrl Pts',(-1.99999999999999,3.46410161513776,2.96321305522333));
#34677=CARTESIAN_POINT('Ctrl Pts',(-4.,2.30940107675851,2.29654638855667));
#34678=CARTESIAN_POINT('Origin',(-4.,2.31179583873664,2.7));
#34679=CARTESIAN_POINT('',(-4.,-2.3094010767585,0.403453611443332));
#34680=CARTESIAN_POINT('Ctrl Pts',(-4.,-2.3094010767585,0.403453611443332));
#34681=CARTESIAN_POINT('Ctrl Pts',(-4.,3.05311331771918E-15,-0.263213055223334));
#34682=CARTESIAN_POINT('Ctrl Pts',(-4.,2.30940107675851,0.403453611443333));
#34683=CARTESIAN_POINT('',(-4.,-2.3094010767585,2.29654638855667));
#34684=CARTESIAN_POINT('',(-4.,-2.3094010767585,2.7));
#34685=CARTESIAN_POINT('Ctrl Pts',(-4.,2.30940107675851,2.29654638855667));
#34686=CARTESIAN_POINT('Ctrl Pts',(-4.,2.77555756156289E-15,2.96321305522333));
#34687=CARTESIAN_POINT('Ctrl Pts',(-4.,-2.3094010767585,2.29654638855667));
#34688=CARTESIAN_POINT('Origin',(0.,0.,0.202072594216369));
#34689=CARTESIAN_POINT('',(4.,2.3094010767585,0.403453611443332));
#34690=CARTESIAN_POINT('',(4.,2.44929359829471E-16,0.0461880215351717));
#34691=CARTESIAN_POINT('Ctrl Pts',(4.,0.,0.0461880215351717));
#34692=CARTESIAN_POINT('Ctrl Pts',(4.,1.07179676972558,0.0461880215351722));
#34693=CARTESIAN_POINT('Ctrl Pts',(4.,2.30940107676122,0.403453611444119));
#34694=CARTESIAN_POINT('',(3.92,-4.80061545265762E-16,-2.08166817117217E-16));
#34695=CARTESIAN_POINT('',(4.27,5.2292418323592E-16,0.202072594216369));
#34696=CARTESIAN_POINT('Origin',(0.,0.,0.));
#34697=CARTESIAN_POINT('',(4.,-2.30940107675851,0.403453611443332));
#34698=CARTESIAN_POINT('Ctrl Pts',(4.,-2.30940107676123,0.40345361144412));
#34699=CARTESIAN_POINT('Ctrl Pts',(4.,-1.07179676972559,0.0461880215351713));
#34700=CARTESIAN_POINT('Ctrl Pts',(4.,0.,0.0461880215351717));
#34701=CARTESIAN_POINT('',(-4.62343916228259E-15,-4.618802153517,0.403453611443332));
#34702=CARTESIAN_POINT('Ctrl Pts',(4.,-2.30940107675851,0.403453611443332));
#34703=CARTESIAN_POINT('Ctrl Pts',(2.,-3.46410161513775,-0.263213055223336));
#34704=CARTESIAN_POINT('Ctrl Pts',(-4.62343916228259E-15,-4.618802153517,
0.403453611443332));
#34705=CARTESIAN_POINT('Ctrl Pts',(-4.6713134644614E-15,-4.618802153517,
0.403453611443332));
#34706=CARTESIAN_POINT('Ctrl Pts',(-2.,-3.46410161513775,-0.263213055223335));
#34707=CARTESIAN_POINT('Ctrl Pts',(-4.,-2.3094010767585,0.403453611443332));
#34708=CARTESIAN_POINT('Ctrl Pts',(6.38831555038924E-15,4.618802153517,
0.403453611443332));
#34709=CARTESIAN_POINT('Ctrl Pts',(2.,3.46410161513775,-0.263213055223334));
#34710=CARTESIAN_POINT('Ctrl Pts',(4.,2.3094010767585,0.403453611443332));
#34711=CARTESIAN_POINT('Origin',(4.00207392470908,2.30820369576943,2.7));
#34712=CARTESIAN_POINT('',(4.,2.3094010767585,2.29654638855667));
#34713=CARTESIAN_POINT('Ctrl Pts',(4.,2.3094010767585,2.29654638855667));
#34714=CARTESIAN_POINT('Ctrl Pts',(2.,3.46410161513775,2.96321305522333));
#34715=CARTESIAN_POINT('Ctrl Pts',(6.31419352837025E-15,4.618802153517,
2.29654638855667));
#34716=CARTESIAN_POINT('',(4.,2.3094010767585,2.7));
#34717=CARTESIAN_POINT('Origin',(4.,-2.31179583873664,2.7));
#34718=CARTESIAN_POINT('',(4.,-9.47417920472595E-17,2.65381197846483));
#34719=CARTESIAN_POINT('Ctrl Pts',(4.,2.30940107676399,2.29654638855508));
#34720=CARTESIAN_POINT('Ctrl Pts',(4.,1.0717967697267,2.65381197846483));
#34721=CARTESIAN_POINT('Ctrl Pts',(4.,3.00375135564423E-16,2.65381197846483));
#34722=CARTESIAN_POINT('',(4.,-2.30940107675851,2.29654638855667));
#34723=CARTESIAN_POINT('Ctrl Pts',(4.,3.00375135564423E-16,2.65381197846483));
#34724=CARTESIAN_POINT('Ctrl Pts',(4.,-1.0717967697267,2.65381197846483));
#34725=CARTESIAN_POINT('Ctrl Pts',(4.,-2.309401076764,2.29654638855508));
#34726=CARTESIAN_POINT('',(4.,-2.30940107675851,2.7));
#34727=CARTESIAN_POINT('Origin',(-0.00207392470908535,-4.61999953450607,
2.7));
#34728=CARTESIAN_POINT('',(-5.55275774471924E-15,-4.618802153517,2.29654638855667));
#34729=CARTESIAN_POINT('Ctrl Pts',(-5.55275774471924E-15,-4.618802153517,
2.29654638855667));
#34730=CARTESIAN_POINT('Ctrl Pts',(2.,-3.46410161513776,2.96321305522334));
#34731=CARTESIAN_POINT('Ctrl Pts',(4.,-2.30940107675851,2.29654638855667));
#34732=CARTESIAN_POINT('',(-4.44089209850063E-15,-4.618802153517,2.7));
#34733=CARTESIAN_POINT('Origin',(-4.00207392470908,-2.30820369576943,2.7));
#34734=CARTESIAN_POINT('Ctrl Pts',(-4.,-2.3094010767585,2.29654638855667));
#34735=CARTESIAN_POINT('Ctrl Pts',(-2.,-3.46410161513775,2.96321305522333));
#34736=CARTESIAN_POINT('Ctrl Pts',(-5.73341293170963E-15,-4.618802153517,
2.29654638855667));
#34737=CARTESIAN_POINT('Origin',(-3.92,0.,2.7));
#34738=CARTESIAN_POINT('',(3.92,-4.80061545265762E-16,2.7));
#34739=CARTESIAN_POINT('Origin',(0.,0.,2.7));
#34740=CARTESIAN_POINT('Origin',(0.,0.,2.49792740578363));
#34741=CARTESIAN_POINT('',(4.27,-5.2292418323592E-16,2.49792740578363));
#34742=CARTESIAN_POINT('Origin',(-2.5,0.,0.));
#34743=CARTESIAN_POINT('Origin',(0.,0.,1.35));
#34744=CARTESIAN_POINT('',(2.117,-2.59257727379495E-16,1.35));
#34745=CARTESIAN_POINT('',(0.,0.,0.));
#34746=CARTESIAN_POINT('Origin',(0.,0.,2.5));
#34747=CARTESIAN_POINT('',(-5.73351648351648,-7.02153260939705E-16,1.11111111111111));
#34748=CARTESIAN_POINT('Origin',(0.,0.,1.11111111111111));
#34749=CARTESIAN_POINT('',(-5.73351648351648,-7.02153260939705E-16,2.5));
#34750=CARTESIAN_POINT('',(-5.73351648351648,-7.02153260939705E-16,2.5));
#34751=CARTESIAN_POINT('Origin',(0.,0.,2.5));
#34752=CARTESIAN_POINT('Origin',(0.,0.,-7.04171909509728E-16));
#34753=CARTESIAN_POINT('',(-5.73351648351648,-7.02153260939705E-16,-1.11111111111111));
#34754=CARTESIAN_POINT('Origin',(0.,0.,-1.11111111111111));
#34755=CARTESIAN_POINT('Origin',(-5.25,-6.42939569552361E-16,-7.04171909509728E-16));
#34756=CARTESIAN_POINT('Origin',(0.,0.,2.5));
#34757=CARTESIAN_POINT('',(-5.73351648351648,-7.02153260939705E-16,-2.5));
#34758=CARTESIAN_POINT('Origin',(0.,0.,-2.5));
#34759=CARTESIAN_POINT('',(-5.73351648351648,-7.02153260939705E-16,2.5));
#34760=CARTESIAN_POINT('Origin',(0.,0.,-2.5));
#34761=CARTESIAN_POINT('',(-8.,-9.79717439317883E-16,-2.25));
#34762=CARTESIAN_POINT('Origin',(0.,0.,-2.25));
#34763=CARTESIAN_POINT('',(-7.75,-9.49101269339199E-16,-2.5));
#34764=CARTESIAN_POINT('',(-7.75,-9.49101269339199E-16,-2.5));
#34765=CARTESIAN_POINT('Origin',(0.,0.,-2.5));
#34766=CARTESIAN_POINT('Origin',(0.,0.,2.5));
#34767=CARTESIAN_POINT('',(8.,9.79717439317883E-16,2.25));
#34768=CARTESIAN_POINT('',(-8.,-9.79717439317883E-16,2.25));
#34769=CARTESIAN_POINT('Origin',(0.,0.,2.25));
#34770=CARTESIAN_POINT('Origin',(0.,0.,2.25));
#34771=CARTESIAN_POINT('',(-8.,-9.79717439317883E-16,2.5));
#34772=CARTESIAN_POINT('Origin',(0.,0.,2.25));
#34773=CARTESIAN_POINT('',(7.75,-9.49101269339199E-16,2.5));
#34774=CARTESIAN_POINT('',(8.,-9.79717439317883E-16,2.25));
#34775=CARTESIAN_POINT('Origin',(0.,0.,2.5));
#34776=CARTESIAN_POINT('Origin',(0.,7.75,-2.5));
#34777=CARTESIAN_POINT('Origin',(0.,7.75,2.5));
#34778=CARTESIAN_POINT('Origin',(0.,0.,2.5));
#34779=CARTESIAN_POINT('',(-4.76648351648352,-5.83725878165016E-16,2.5));
#34780=CARTESIAN_POINT('Origin',(0.,0.,2.5));
#34781=CARTESIAN_POINT('',(-4.76648351648352,-5.83725878165016E-16,1.11111111111111));
#34782=CARTESIAN_POINT('',(-4.76648351648352,-5.83725878165016E-16,2.5));
#34783=CARTESIAN_POINT('Origin',(0.,0.,1.11111111111111));
#34784=CARTESIAN_POINT('Origin',(0.,0.,-7.04171909509728E-16));
#34785=CARTESIAN_POINT('',(-4.03824256096085,-4.94542082646132E-16,-4.33680868994202E-16));
#34786=CARTESIAN_POINT('Origin',(-5.25,-6.42939569552361E-16,-7.04171909509728E-16));
#34787=CARTESIAN_POINT('Origin',(0.,0.,-4.33680868994202E-16));
#34788=CARTESIAN_POINT('Origin',(0.,0.,2.5));
#34789=CARTESIAN_POINT('',(-3.26912128048043,-4.00351891216485E-16,-2.22044604925031E-15));
#34790=CARTESIAN_POINT('Origin',(0.,0.,-2.16840434497101E-15));
#34791=CARTESIAN_POINT('',(-3.26912128048043,-4.00351891216485E-16,1.75131888199846));
#34792=CARTESIAN_POINT('',(-3.26912128048043,-4.00351891216486E-16,2.5));
#34793=CARTESIAN_POINT('Origin',(0.,0.,1.75131888199846));
#34794=CARTESIAN_POINT('Origin',(0.,0.,2.5));
#34795=CARTESIAN_POINT('',(-4.01780239848197,-4.92038884690751E-16,2.5));
#34796=CARTESIAN_POINT('',(-4.01780239848197,-4.9203888469075E-16,2.5));
#34797=CARTESIAN_POINT('Origin',(0.,0.,2.5));
#34798=CARTESIAN_POINT('Origin',(0.,4.76648351648352,2.5));
#34799=CARTESIAN_POINT('Origin',(0.,3.26912128048043,-1.32068860796267E-15));
#34800=CARTESIAN_POINT('Origin',(0.,0.,2.5));
#34801=CARTESIAN_POINT('',(-2.5,-3.06161699786838E-16,1.73087871951958));
#34802=CARTESIAN_POINT('Origin',(0.,0.,1.73087871951958));
#34803=CARTESIAN_POINT('',(-3.26912128048043,-4.00351891216485E-16,2.5));
#34804=CARTESIAN_POINT('',(-3.26912128048043,-4.00351891216486E-16,2.5));
#34805=CARTESIAN_POINT('Origin',(0.,0.,2.5));
#34806=CARTESIAN_POINT('Origin',(0.,0.,2.5));
#34807=CARTESIAN_POINT('',(2.5,3.2146978477618E-16,-2.25));
#34808=CARTESIAN_POINT('',(-2.5,-3.06161699786838E-16,-2.25));
#34809=CARTESIAN_POINT('Origin',(0.,0.,-2.25));
#34810=CARTESIAN_POINT('Origin',(0.,0.,-2.25));
#34811=CARTESIAN_POINT('',(-2.5,-3.06161699786838E-16,2.5));
#34812=CARTESIAN_POINT('Origin',(0.,0.,-2.25));
#34813=CARTESIAN_POINT('',(2.75,-3.36777869765522E-16,-2.5));
#34814=CARTESIAN_POINT('',(2.5,-3.06161699786838E-16,-2.25));
#34815=CARTESIAN_POINT('Origin',(0.,0.,-2.5));
#34816=CARTESIAN_POINT('Origin',(0.,0.,2.5));
#34817=CARTESIAN_POINT('',(-4.76648351648352,-5.83725878165016E-16,-1.11111111111111));
#34818=CARTESIAN_POINT('Origin',(0.,0.,-1.11111111111111));
#34819=CARTESIAN_POINT('',(-4.76648351648352,-5.83725878165016E-16,-2.5));
#34820=CARTESIAN_POINT('',(-4.76648351648352,-5.83725878165016E-16,2.5));
#34821=CARTESIAN_POINT('Origin',(0.,0.,-2.5));
#34822=CARTESIAN_POINT('Origin',(0.,0.,-7.04171909509728E-16));
#34823=CARTESIAN_POINT('',(-4.03824256096085,-4.94542082646132E-16,-8.67361737988404E-16));
#34824=CARTESIAN_POINT('Origin',(0.,0.,-8.67361737988404E-16));
#34825=CARTESIAN_POINT('Origin',(-5.25,-6.42939569552361E-16,-7.04171909509728E-16));
#34826=CARTESIAN_POINT('Origin',(0.,0.,2.5));
#34827=CARTESIAN_POINT('',(-3.26912128048043,-4.00351891216485E-16,1.75131888199846));
#34828=CARTESIAN_POINT('Origin',(0.,0.,1.75131888199846));
#34829=CARTESIAN_POINT('',(-3.26912128048043,-4.00351891216485E-16,-2.22044604925031E-15));
#34830=CARTESIAN_POINT('',(-3.26912128048043,-4.00351891216486E-16,2.5));
#34831=CARTESIAN_POINT('Origin',(0.,0.,-2.16840434497101E-15));
#34832=CARTESIAN_POINT('Origin',(0.,0.,1.75131888199846));
#34833=CARTESIAN_POINT('',(-4.01780239848197,-4.92038884690751E-16,2.5));
#34834=CARTESIAN_POINT('Origin',(0.,0.,2.5));
#34835=CARTESIAN_POINT('',(-3.26912128048043,-4.00351891216486E-16,1.75131888199846));
#34836=CARTESIAN_POINT('Origin',(0.,4.01780239848197,2.5));
#34837=CARTESIAN_POINT('Origin',(0.,3.26912128048043,-1.51358163738168E-15));
#34838=CARTESIAN_POINT('Origin',(0.,2.75,-2.5));
#34839=CARTESIAN_POINT('Origin',(0.,5.25,-7.04171909509728E-16));
#34840=CARTESIAN_POINT('',(-1.21175743903915,5.25,-7.04171909509728E-16));
#34841=CARTESIAN_POINT('',(1.21175743903915,5.25,-7.04171909509728E-16));
#34842=CARTESIAN_POINT('Origin',(0.,5.25,-7.04171909509728E-16));
#34843=CARTESIAN_POINT('Origin',(3.08587257453549,4.24733922046847,-7.04171909509728E-16));
#34844=CARTESIAN_POINT('',(2.10554021329255,4.95959237249138,-7.04171909509728E-16));
#34845=CARTESIAN_POINT('',(4.06620493577843,3.53508606844556,-7.04171909509728E-16));
#34846=CARTESIAN_POINT('Origin',(3.08587257453549,4.24733922046847,-7.04171909509728E-16));
#34847=CARTESIAN_POINT('Origin',(4.99304671054956,1.62233922046846,-7.04171909509728E-16));
#34848=CARTESIAN_POINT('',(4.6185930688262,2.77478902903577,-7.04171909509728E-16));
#34849=CARTESIAN_POINT('',(5.36750035227292,0.469889411901148,-7.04171909509728E-16));
#34850=CARTESIAN_POINT('Origin',(4.99304671054956,1.62233922046846,-7.04171909509728E-16));
#34851=CARTESIAN_POINT('Origin',(4.99304671054955,-1.6223392204685,-7.04171909509728E-16));
#34852=CARTESIAN_POINT('',(5.36750035227292,-0.469889411901191,-7.04171909509728E-16));
#34853=CARTESIAN_POINT('',(4.61859306882618,-2.77478902903581,-7.04171909509728E-16));
#34854=CARTESIAN_POINT('Origin',(4.99304671054955,-1.6223392204685,-7.04171909509728E-16));
#34855=CARTESIAN_POINT('Origin',(3.08587257453546,-4.24733922046849,-7.04171909509728E-16));
#34856=CARTESIAN_POINT('',(4.0662049357784,-3.53508606844559,-7.04171909509728E-16));
#34857=CARTESIAN_POINT('',(2.10554021329252,-4.95959237249139,-7.04171909509728E-16));
#34858=CARTESIAN_POINT('Origin',(3.08587257453546,-4.24733922046849,-7.04171909509728E-16));
#34859=CARTESIAN_POINT('Origin',(-3.66605540578529E-14,-5.25,-7.04171909509728E-16));
#34860=CARTESIAN_POINT('',(1.21175743903911,-5.25000000000001,-7.04171909509728E-16));
#34861=CARTESIAN_POINT('',(-1.21175743903919,-5.24999999999999,-7.04171909509728E-16));
#34862=CARTESIAN_POINT('Origin',(-3.66605540578529E-14,-5.25,-7.04171909509728E-16));
#34863=CARTESIAN_POINT('Origin',(-3.08587257453552,-4.24733922046845,-7.04171909509728E-16));
#34864=CARTESIAN_POINT('',(-2.10554021329259,-4.95959237249137,-7.04171909509728E-16));
#34865=CARTESIAN_POINT('',(-4.06620493577845,-3.53508606844553,-7.04171909509728E-16));
#34866=CARTESIAN_POINT('Origin',(-3.08587257453552,-4.24733922046845,-7.04171909509728E-16));
#34867=CARTESIAN_POINT('Origin',(-4.99304671054957,-1.62233922046843,-7.04171909509728E-16));
#34868=CARTESIAN_POINT('',(-4.61859306882622,-2.77478902903574,-7.04171909509728E-16));
#34869=CARTESIAN_POINT('',(-5.36750035227292,-0.469889411901115,-7.04171909509728E-16));
#34870=CARTESIAN_POINT('Origin',(-4.99304671054957,-1.62233922046843,-7.04171909509728E-16));
#34871=CARTESIAN_POINT('Origin',(-4.99304671054954,1.62233922046853,-7.04171909509728E-16));
#34872=CARTESIAN_POINT('',(-5.36750035227291,0.469889411901223,-7.04171909509728E-16));
#34873=CARTESIAN_POINT('',(-4.61859306882617,2.77478902903584,-7.04171909509728E-16));
#34874=CARTESIAN_POINT('Origin',(-4.99304671054954,1.62233922046853,-7.04171909509728E-16));
#34875=CARTESIAN_POINT('Origin',(-3.08587257453543,4.24733922046851,-7.04171909509728E-16));
#34876=CARTESIAN_POINT('',(-4.06620493577838,3.53508606844562,-7.04171909509728E-16));
#34877=CARTESIAN_POINT('',(-2.10554021329248,4.95959237249141,-7.04171909509728E-16));
#34878=CARTESIAN_POINT('Origin',(-3.08587257453543,4.24733922046851,-7.04171909509728E-16));
#34879=CARTESIAN_POINT('',(0.,0.,0.));
#34880=CARTESIAN_POINT('',(0.,0.,0.));
#34881=CARTESIAN_POINT('',(-2.25046001479401,190.828431883169,20.8299327490105));
#34882=CARTESIAN_POINT('',(-7.45046001479403,190.828431883169,20.8299327490106));
#34883=CARTESIAN_POINT('',(-12.450460014794,190.828431883169,20.8299327490105));
#34884=CARTESIAN_POINT('',(0.,0.,0.));
#34885=CARTESIAN_POINT('Origin',(2.69069170170099,0.,-6.2440918089009));
#34886=CARTESIAN_POINT('',(2.69069170170099,0.,-8.19999999999999));
#34887=CARTESIAN_POINT('',(2.69069170170099,0.,-6.2440918089009));
#34888=CARTESIAN_POINT('',(2.69069170170099,0.,-6.33074178210092));
#34889=CARTESIAN_POINT('',(2.69069170170099,500.,-6.2440918089009));
#34890=CARTESIAN_POINT('',(2.69069170170099,0.,-6.2440918089009));
#34891=CARTESIAN_POINT('',(2.69069170170099,500.,-8.19999999999999));
#34892=CARTESIAN_POINT('',(2.69069170170099,500.,-6.33074178210092));
#34893=CARTESIAN_POINT('',(2.69069170170099,0.,-8.19999999999999));
#34894=CARTESIAN_POINT('Origin',(2.69069170170097,0.,6.24409180890091));
#34895=CARTESIAN_POINT('',(2.69069170170097,0.,6.24409180890091));
#34896=CARTESIAN_POINT('',(2.69069170170097,0.,8.2));
#34897=CARTESIAN_POINT('',(2.69069170170098,0.,-0.0866499732000153));
#34898=CARTESIAN_POINT('',(2.69069170170097,500.,8.2));
#34899=CARTESIAN_POINT('',(2.69069170170097,0.,8.2));
#34900=CARTESIAN_POINT('',(2.69069170170097,500.,6.24409180890091));
#34901=CARTESIAN_POINT('',(2.69069170170098,500.,-0.0866499732000138));
#34902=CARTESIAN_POINT('',(2.69069170170097,0.,6.24409180890091));
#34903=CARTESIAN_POINT('Origin',(6.09999999999999,0.,3.90000000000001));
#34904=CARTESIAN_POINT('',(6.1,0.,-2.83478351060188));
#34905=CARTESIAN_POINT('',(6.1,500.,-2.83478351060188));
#34906=CARTESIAN_POINT('',(6.1,0.,-2.83478351060188));
#34907=CARTESIAN_POINT('',(6.09999999999999,0.,2.8347835106019));
#34908=CARTESIAN_POINT('',(6.09999999999999,0.,3.90000000000001));
#34909=CARTESIAN_POINT('',(6.09999999999999,500.,2.8347835106019));
#34910=CARTESIAN_POINT('',(6.09999999999999,0.,2.8347835106019));
#34911=CARTESIAN_POINT('',(6.1,500.,-1.25869587765046));
#34912=CARTESIAN_POINT('Origin',(13.9,0.,3.90000000000001));
#34913=CARTESIAN_POINT('',(12.8347835106019,0.,3.90000000000001));
#34914=CARTESIAN_POINT('',(12.8347835106019,500.,3.90000000000001));
#34915=CARTESIAN_POINT('',(12.8347835106019,0.,3.90000000000001));
#34916=CARTESIAN_POINT('',(7.1652164893981,500.,3.90000000000001));
#34917=CARTESIAN_POINT('',(5.15869587765046,500.,3.90000000000001));
#34918=CARTESIAN_POINT('',(7.1652164893981,0.,3.90000000000001));
#34919=CARTESIAN_POINT('',(7.1652164893981,0.,3.90000000000001));
#34920=CARTESIAN_POINT('',(13.9,0.,3.90000000000001));
#34921=CARTESIAN_POINT('Origin',(13.9,0.,-3.89999999999999));
#34922=CARTESIAN_POINT('',(13.9,0.,2.8347835106019));
#34923=CARTESIAN_POINT('',(13.9,500.,2.8347835106019));
#34924=CARTESIAN_POINT('',(13.9,0.,2.8347835106019));
#34925=CARTESIAN_POINT('',(13.9,0.,-2.83478351060188));
#34926=CARTESIAN_POINT('',(13.9,0.,-3.89999999999999));
#34927=CARTESIAN_POINT('',(13.9,500.,-2.83478351060188));
#34928=CARTESIAN_POINT('',(13.9,0.,-2.83478351060188));
#34929=CARTESIAN_POINT('',(13.9,500.,-5.15869587765045));
#34930=CARTESIAN_POINT('Origin',(10.,0.,1.02489030670754E-14));
#34931=CARTESIAN_POINT('',(12.1,500.,1.26583485389822E-14));
#34932=CARTESIAN_POINT('Origin',(10.,500.,1.02489030670754E-14));
#34933=CARTESIAN_POINT('',(12.1,0.,1.26583485389822E-14));
#34934=CARTESIAN_POINT('',(12.1,0.,1.26583485389822E-14));
#34935=CARTESIAN_POINT('Origin',(10.,0.,1.02489030670754E-14));
#34936=CARTESIAN_POINT('Origin',(6.1,0.,-3.89999999999999));
#34937=CARTESIAN_POINT('',(7.16521648939811,0.,-3.89999999999999));
#34938=CARTESIAN_POINT('',(7.16521648939811,500.,-3.89999999999999));
#34939=CARTESIAN_POINT('',(7.16521648939811,0.,-3.89999999999999));
#34940=CARTESIAN_POINT('',(12.8347835106019,500.,-3.89999999999999));
#34941=CARTESIAN_POINT('',(1.25869587765047,500.,-3.9));
#34942=CARTESIAN_POINT('',(12.8347835106019,0.,-3.89999999999999));
#34943=CARTESIAN_POINT('',(12.8347835106019,0.,-3.89999999999999));
#34944=CARTESIAN_POINT('',(6.1,0.,-3.89999999999999));
#34945=CARTESIAN_POINT('Origin',(15.509308298299,0.,-6.57452478769711));
#34946=CARTESIAN_POINT('',(15.509308298299,0.,-8.19999999999998));
#34947=CARTESIAN_POINT('',(15.509308298299,0.,-6.57452478769711));
#34948=CARTESIAN_POINT('',(15.509308298299,0.,-8.19999999999998));
#34949=CARTESIAN_POINT('',(15.509308298299,500.,-6.57452478769711));
#34950=CARTESIAN_POINT('',(15.509308298299,0.,-6.57452478769711));
#34951=CARTESIAN_POINT('',(15.509308298299,500.,-8.19999999999998));
#34952=CARTESIAN_POINT('',(15.509308298299,500.,-6.49595827149902));
#34953=CARTESIAN_POINT('',(15.509308298299,0.,-8.19999999999998));
#34954=CARTESIAN_POINT('Origin',(12.8347835106019,0.,-3.89999999999999));
#34955=CARTESIAN_POINT('',(15.509308298299,0.,-6.57452478769711));
#34956=CARTESIAN_POINT('',(9.35978351060189,500.,-0.424999999999988));
#34957=CARTESIAN_POINT('Origin',(16.5745247876971,0.,-5.509308298299));
#34958=CARTESIAN_POINT('',(16.5745247876971,0.,-5.509308298299));
#34959=CARTESIAN_POINT('',(16.5745247876971,0.,-5.509308298299));
#34960=CARTESIAN_POINT('',(16.5745247876971,500.,-5.509308298299));
#34961=CARTESIAN_POINT('',(16.5745247876971,0.,-5.509308298299));
#34962=CARTESIAN_POINT('',(11.7622623938486,500.,-0.697045904450441));
#34963=CARTESIAN_POINT('Origin',(18.2,0.,-5.509308298299));
#34964=CARTESIAN_POINT('',(18.2,0.,-5.509308298299));
#34965=CARTESIAN_POINT('',(18.2,0.,-5.509308298299));
#34966=CARTESIAN_POINT('',(18.2,500.,-5.509308298299));
#34967=CARTESIAN_POINT('',(18.2,0.,-5.509308298299));
#34968=CARTESIAN_POINT('',(7.30869587765047,500.,-5.509308298299));
#34969=CARTESIAN_POINT('Origin',(18.2,0.,-3.09999999999998));
#34970=CARTESIAN_POINT('',(18.2,0.,-3.09999999999998));
#34971=CARTESIAN_POINT('',(18.2,0.,-5.509308298299));
#34972=CARTESIAN_POINT('',(18.2,500.,-3.09999999999998));
#34973=CARTESIAN_POINT('',(18.2,0.,-3.09999999999998));
#34974=CARTESIAN_POINT('',(18.2,500.,-4.75869587765046));
#34975=CARTESIAN_POINT('Origin',(18.5210615995951,0.,-3.09999999999998));
#34976=CARTESIAN_POINT('',(18.5210615995951,0.,-3.09999999999998));
#34977=CARTESIAN_POINT('',(18.2,0.,-3.09999999999998));
#34978=CARTESIAN_POINT('',(18.5210615995951,500.,-3.09999999999998));
#34979=CARTESIAN_POINT('',(18.5210615995951,0.,-3.09999999999998));
#34980=CARTESIAN_POINT('',(7.46922667744803,500.,-3.09999999999999));
#34981=CARTESIAN_POINT('Origin',(20.,0.,-4.57893840040485));
#34982=CARTESIAN_POINT('',(20.,0.,-4.57893840040485));
#34983=CARTESIAN_POINT('',(20.,0.,-4.57893840040485));
#34984=CARTESIAN_POINT('',(20.,500.,-4.57893840040485));
#34985=CARTESIAN_POINT('',(20.,0.,-4.57893840040485));
#34986=CARTESIAN_POINT('',(14.5639612775493,500.,0.857100322045891));
#34987=CARTESIAN_POINT('Origin',(20.,0.,-9.49999999999998));
#34988=CARTESIAN_POINT('',(20.,0.,-9.49999999999998));
#34989=CARTESIAN_POINT('',(20.,0.,-9.49999999999998));
#34990=CARTESIAN_POINT('',(20.,500.,-9.49999999999998));
#34991=CARTESIAN_POINT('',(20.,0.,-9.49999999999998));
#34992=CARTESIAN_POINT('',(20.,500.,-7.95869587765045));
#34993=CARTESIAN_POINT('Origin',(19.5,0.,-9.49999999999998));
#34994=CARTESIAN_POINT('',(19.5,0.,-9.99999999999998));
#34995=CARTESIAN_POINT('Origin',(19.5,0.,-9.49999999999998));
#34996=CARTESIAN_POINT('',(19.5,500.,-9.99999999999998));
#34997=CARTESIAN_POINT('',(19.5,0.,-9.99999999999998));
#34998=CARTESIAN_POINT('Origin',(19.5,500.,-9.49999999999998));
#34999=CARTESIAN_POINT('Origin',(14.5789384004049,0.,-9.99999999999998));
#35000=CARTESIAN_POINT('',(14.5789384004049,0.,-9.99999999999998));
#35001=CARTESIAN_POINT('',(14.5789384004049,0.,-9.99999999999998));
#35002=CARTESIAN_POINT('',(14.5789384004049,500.,-9.99999999999998));
#35003=CARTESIAN_POINT('',(14.5789384004049,0.,-9.99999999999998));
#35004=CARTESIAN_POINT('',(5.49816507785291,500.,-9.99999999999999));
#35005=CARTESIAN_POINT('Origin',(13.1,0.,-8.52106159959512));
#35006=CARTESIAN_POINT('',(13.1,0.,-8.52106159959512));
#35007=CARTESIAN_POINT('',(14.5789384004049,0.,-9.99999999999998));
#35008=CARTESIAN_POINT('',(13.1,500.,-8.52106159959512));
#35009=CARTESIAN_POINT('',(13.1,0.,-8.52106159959512));
#35010=CARTESIAN_POINT('',(8.40343047775168,500.,-3.82449207734681));
#35011=CARTESIAN_POINT('Origin',(13.1,0.,-8.19999999999998));
#35012=CARTESIAN_POINT('',(13.1,0.,-8.19999999999998));
#35013=CARTESIAN_POINT('',(13.1,0.,-8.19999999999998));
#35014=CARTESIAN_POINT('',(13.1,500.,-8.19999999999998));
#35015=CARTESIAN_POINT('',(13.1,0.,-8.19999999999998));
#35016=CARTESIAN_POINT('',(13.1,500.,-7.30869587765046));
#35017=CARTESIAN_POINT('Origin',(15.509308298299,0.,-8.19999999999998));
#35018=CARTESIAN_POINT('',(15.509308298299,0.,-8.19999999999998));
#35019=CARTESIAN_POINT('',(5.96335002679998,500.,-8.19999999999999));
#35020=CARTESIAN_POINT('Origin',(4.49069170170097,0.,6.57452478769713));
#35021=CARTESIAN_POINT('',(4.49069170170097,0.,8.2));
#35022=CARTESIAN_POINT('',(4.49069170170097,0.,6.57452478769713));
#35023=CARTESIAN_POINT('',(4.49069170170097,0.,8.2));
#35024=CARTESIAN_POINT('',(4.49069170170097,500.,6.57452478769713));
#35025=CARTESIAN_POINT('',(4.49069170170097,0.,6.57452478769713));
#35026=CARTESIAN_POINT('',(4.49069170170097,500.,8.2));
#35027=CARTESIAN_POINT('',(4.49069170170098,500.,0.0785665161980986));
#35028=CARTESIAN_POINT('',(4.49069170170097,0.,8.2));
#35029=CARTESIAN_POINT('Origin',(7.1652164893981,0.,3.90000000000001));
#35030=CARTESIAN_POINT('',(4.49069170170097,0.,6.57452478769713));
#35031=CARTESIAN_POINT('',(7.05760824469904,500.,4.00760824469907));
#35032=CARTESIAN_POINT('Origin',(3.42547521230287,0.,5.50930829829902));
#35033=CARTESIAN_POINT('',(3.42547521230287,0.,5.50930829829902));
#35034=CARTESIAN_POINT('',(4.65512936145237,500.,4.27965414914951));
#35035=CARTESIAN_POINT('Origin',(6.89999999999999,0.,8.52106159959514));
#35036=CARTESIAN_POINT('',(5.42106159959512,0.,10.));
#35037=CARTESIAN_POINT('',(6.89999999999999,0.,8.52106159959514));
#35038=CARTESIAN_POINT('',(5.42106159959512,0.,10.));
#35039=CARTESIAN_POINT('',(6.89999999999999,500.,8.52106159959514));
#35040=CARTESIAN_POINT('',(6.89999999999999,0.,8.52106159959514));
#35041=CARTESIAN_POINT('',(5.42106159959512,500.,10.));
#35042=CARTESIAN_POINT('',(8.01396127754924,500.,7.40710032204589));
#35043=CARTESIAN_POINT('',(5.42106159959512,0.,10.));
#35044=CARTESIAN_POINT('Origin',(6.89999999999999,0.,8.2));
#35045=CARTESIAN_POINT('',(6.89999999999999,0.,8.2));
#35046=CARTESIAN_POINT('',(6.89999999999999,0.,8.2));
#35047=CARTESIAN_POINT('',(6.89999999999999,500.,8.2));
#35048=CARTESIAN_POINT('',(6.89999999999999,0.,8.2));
#35049=CARTESIAN_POINT('',(6.9,500.,0.891304122349535));
#35050=CARTESIAN_POINT('Origin',(4.49069170170097,0.,8.2));
#35051=CARTESIAN_POINT('',(4.49069170170097,0.,8.2));
#35052=CARTESIAN_POINT('',(0.454041728500951,500.,8.2));
#35053=CARTESIAN_POINT('Origin',(16.5745247876971,0.,5.50930829829903));
#35054=CARTESIAN_POINT('',(18.2,0.,5.50930829829903));
#35055=CARTESIAN_POINT('',(16.5745247876971,0.,5.50930829829903));
#35056=CARTESIAN_POINT('',(18.2,0.,5.50930829829903));
#35057=CARTESIAN_POINT('',(16.5745247876971,500.,5.50930829829903));
#35058=CARTESIAN_POINT('',(16.5745247876971,0.,5.50930829829903));
#35059=CARTESIAN_POINT('',(18.2,500.,5.50930829829903));
#35060=CARTESIAN_POINT('',(6.49595827149902,500.,5.50930829829902));
#35061=CARTESIAN_POINT('',(18.2,0.,5.50930829829903));
#35062=CARTESIAN_POINT('Origin',(13.9,0.,2.8347835106019));
#35063=CARTESIAN_POINT('',(16.5745247876971,0.,5.50930829829903));
#35064=CARTESIAN_POINT('',(7.21630412234953,500.,-3.84891236704857));
#35065=CARTESIAN_POINT('Origin',(15.509308298299,0.,6.57452478769714));
#35066=CARTESIAN_POINT('',(15.509308298299,0.,6.57452478769714));
#35067=CARTESIAN_POINT('',(15.509308298299,0.,6.57452478769714));
#35068=CARTESIAN_POINT('',(15.509308298299,500.,6.57452478769714));
#35069=CARTESIAN_POINT('',(15.509308298299,0.,6.57452478769714));
#35070=CARTESIAN_POINT('',(7.48835002679998,500.,-1.4464334838019));
#35071=CARTESIAN_POINT('Origin',(15.509308298299,0.,8.20000000000001));
#35072=CARTESIAN_POINT('',(15.509308298299,0.,8.20000000000001));
#35073=CARTESIAN_POINT('',(15.509308298299,0.,8.20000000000001));
#35074=CARTESIAN_POINT('',(15.509308298299,500.,8.20000000000001));
#35075=CARTESIAN_POINT('',(15.509308298299,0.,8.20000000000001));
#35076=CARTESIAN_POINT('',(15.509308298299,500.,0.891304122349531));
#35077=CARTESIAN_POINT('Origin',(13.1,0.,8.20000000000001));
#35078=CARTESIAN_POINT('',(13.1,0.,8.20000000000001));
#35079=CARTESIAN_POINT('',(15.509308298299,0.,8.20000000000001));
#35080=CARTESIAN_POINT('',(13.1,500.,8.20000000000001));
#35081=CARTESIAN_POINT('',(13.1,0.,8.20000000000001));
#35082=CARTESIAN_POINT('',(4.75869587765046,500.,8.20000000000001));
#35083=CARTESIAN_POINT('Origin',(13.1,0.,8.52106159959514));
#35084=CARTESIAN_POINT('',(13.1,0.,8.52106159959514));
#35085=CARTESIAN_POINT('',(13.1,0.,8.20000000000001));
#35086=CARTESIAN_POINT('',(13.1,500.,8.52106159959514));
#35087=CARTESIAN_POINT('',(13.1,0.,8.52106159959514));
#35088=CARTESIAN_POINT('',(13.1,500.,1.05183492214711));
#35089=CARTESIAN_POINT('Origin',(14.5789384004049,0.,10.));
#35090=CARTESIAN_POINT('',(14.5789384004049,0.,10.));
#35091=CARTESIAN_POINT('',(14.5789384004049,0.,10.));
#35092=CARTESIAN_POINT('',(14.5789384004049,500.,10.));
#35093=CARTESIAN_POINT('',(14.5789384004049,0.,10.));
#35094=CARTESIAN_POINT('',(5.93420380030364,500.,1.35526539989879));
#35095=CARTESIAN_POINT('Origin',(19.5,0.,10.));
#35096=CARTESIAN_POINT('',(19.5,0.,10.));
#35097=CARTESIAN_POINT('',(19.5,0.,10.));
#35098=CARTESIAN_POINT('',(19.5,500.,10.));
#35099=CARTESIAN_POINT('',(19.5,0.,10.));
#35100=CARTESIAN_POINT('',(7.95869587765046,500.,10.));
#35101=CARTESIAN_POINT('Origin',(19.5,0.,9.50000000000001));
#35102=CARTESIAN_POINT('',(20.,0.,9.50000000000001));
#35103=CARTESIAN_POINT('Origin',(19.5,0.,9.50000000000001));
#35104=CARTESIAN_POINT('',(20.,500.,9.50000000000001));
#35105=CARTESIAN_POINT('',(20.,0.,9.50000000000001));
#35106=CARTESIAN_POINT('Origin',(19.5,500.,9.50000000000001));
#35107=CARTESIAN_POINT('Origin',(20.,0.,4.57893840040489));
#35108=CARTESIAN_POINT('',(20.,0.,4.57893840040489));
#35109=CARTESIAN_POINT('',(20.,0.,4.57893840040489));
#35110=CARTESIAN_POINT('',(20.,500.,4.57893840040489));
#35111=CARTESIAN_POINT('',(20.,0.,4.57893840040489));
#35112=CARTESIAN_POINT('',(20.,500.,-0.919226677448016));
#35113=CARTESIAN_POINT('Origin',(18.5210615995951,0.,3.10000000000002));
#35114=CARTESIAN_POINT('',(18.5210615995951,0.,3.10000000000002));
#35115=CARTESIAN_POINT('',(20.,0.,4.57893840040489));
#35116=CARTESIAN_POINT('',(18.5210615995951,500.,3.10000000000002));
#35117=CARTESIAN_POINT('',(18.5210615995951,0.,3.10000000000002));
#35118=CARTESIAN_POINT('',(10.6157961996964,500.,-4.80526539989878));
#35119=CARTESIAN_POINT('Origin',(18.2,0.,3.10000000000002));
#35120=CARTESIAN_POINT('',(18.2,0.,3.10000000000002));
#35121=CARTESIAN_POINT('',(18.2,0.,3.10000000000002));
#35122=CARTESIAN_POINT('',(18.2,500.,3.10000000000002));
#35123=CARTESIAN_POINT('',(18.2,0.,3.10000000000002));
#35124=CARTESIAN_POINT('',(7.30869587765046,500.,3.10000000000001));
#35125=CARTESIAN_POINT('Origin',(18.2,0.,5.50930829829903));
#35126=CARTESIAN_POINT('',(18.2,0.,5.50930829829903));
#35127=CARTESIAN_POINT('',(18.2,500.,-0.454041728500943));
#35128=CARTESIAN_POINT('Origin',(6.1,0.,-2.83478351060188));
#35129=CARTESIAN_POINT('',(3.42547521230287,0.,-5.50930829829901));
#35130=CARTESIAN_POINT('',(2.78369587765047,500.,-6.15108763295141));
#35131=CARTESIAN_POINT('Origin',(4.49069170170099,0.,-6.57452478769712));
#35132=CARTESIAN_POINT('',(4.49069170170099,0.,-6.57452478769712));
#35133=CARTESIAN_POINT('',(4.49069170170099,0.,-6.57452478769712));
#35134=CARTESIAN_POINT('',(4.49069170170099,500.,-6.57452478769712));
#35135=CARTESIAN_POINT('',(4.49069170170099,0.,-6.57452478769712));
#35136=CARTESIAN_POINT('',(2.51164997320002,500.,-8.55356651619809));
#35137=CARTESIAN_POINT('Origin',(4.49069170170099,0.,-8.19999999999999));
#35138=CARTESIAN_POINT('',(4.49069170170099,0.,-8.19999999999999));
#35139=CARTESIAN_POINT('',(4.49069170170099,0.,-8.19999999999999));
#35140=CARTESIAN_POINT('',(4.49069170170099,500.,-8.19999999999999));
#35141=CARTESIAN_POINT('',(4.49069170170099,0.,-8.19999999999999));
#35142=CARTESIAN_POINT('',(4.49069170170099,500.,-7.30869587765047));
#35143=CARTESIAN_POINT('Origin',(6.9,0.,-8.19999999999999));
#35144=CARTESIAN_POINT('',(6.9,0.,-8.19999999999999));
#35145=CARTESIAN_POINT('',(4.49069170170099,0.,-8.19999999999999));
#35146=CARTESIAN_POINT('',(6.9,500.,-8.19999999999999));
#35147=CARTESIAN_POINT('',(6.9,0.,-8.19999999999999));
#35148=CARTESIAN_POINT('',(1.65869587765047,500.,-8.19999999999999));
#35149=CARTESIAN_POINT('Origin',(6.9,0.,-8.52106159959512));
#35150=CARTESIAN_POINT('',(6.9,0.,-8.52106159959512));
#35151=CARTESIAN_POINT('',(6.9,0.,-8.19999999999999));
#35152=CARTESIAN_POINT('',(6.9,500.,-8.52106159959512));
#35153=CARTESIAN_POINT('',(6.9,0.,-8.52106159959512));
#35154=CARTESIAN_POINT('',(6.9,500.,-7.46922667744803));
#35155=CARTESIAN_POINT('Origin',(5.42106159959514,0.,-9.99999999999999));
#35156=CARTESIAN_POINT('',(5.42106159959514,0.,-9.99999999999999));
#35157=CARTESIAN_POINT('',(5.42106159959514,0.,-9.99999999999999));
#35158=CARTESIAN_POINT('',(5.42106159959514,500.,-9.99999999999999));
#35159=CARTESIAN_POINT('',(5.42106159959514,0.,-9.99999999999999));
#35160=CARTESIAN_POINT('',(4.06579619969635,500.,-11.3552653998988));
#35161=CARTESIAN_POINT('Origin',(-2.69069170170098,0.,-8.2));
#35162=CARTESIAN_POINT('',(-2.69069170170098,0.,-8.2));
#35163=CARTESIAN_POINT('',(-3.13664997320002,0.,-8.2));
#35164=CARTESIAN_POINT('',(-2.69069170170098,500.,-8.2));
#35165=CARTESIAN_POINT('',(-3.13664997320002,500.,-8.2));
#35166=CARTESIAN_POINT('',(-2.69069170170098,0.,-8.2));
#35167=CARTESIAN_POINT('Origin',(-2.69069170170098,0.,-6.24409180890091));
#35168=CARTESIAN_POINT('',(-2.69069170170098,0.,-6.24409180890091));
#35169=CARTESIAN_POINT('',(-2.69069170170098,0.,-6.33074178210092));
#35170=CARTESIAN_POINT('',(-2.69069170170098,500.,-6.24409180890091));
#35171=CARTESIAN_POINT('',(-2.69069170170098,500.,-6.33074178210092));
#35172=CARTESIAN_POINT('',(-2.69069170170098,0.,-6.24409180890091));
#35173=CARTESIAN_POINT('Origin',(-3.58260824469906,0.,-6.41739175530094));
#35174=CARTESIAN_POINT('',(-5.42106159959513,0.,-9.99999999999999));
#35175=CARTESIAN_POINT('',(0.500000000000009,0.,-9.99999999999999));
#35176=CARTESIAN_POINT('',(-5.42106159959513,0.,10.));
#35177=CARTESIAN_POINT('',(-5.42106159959513,0.,10.));
#35178=CARTESIAN_POINT('',(-6.9,0.,8.52106159959513));
#35179=CARTESIAN_POINT('',(-5.42106159959513,0.,10.));
#35180=CARTESIAN_POINT('',(-6.9,0.,8.2));
#35181=CARTESIAN_POINT('',(-6.9,0.,8.2));
#35182=CARTESIAN_POINT('',(-4.49069170170099,0.,8.2));
#35183=CARTESIAN_POINT('',(-4.49069170170099,0.,8.2));
#35184=CARTESIAN_POINT('',(-4.49069170170099,0.,6.57452478769713));
#35185=CARTESIAN_POINT('',(-4.49069170170099,0.,8.2));
#35186=CARTESIAN_POINT('',(-7.16521648939811,0.,3.9));
#35187=CARTESIAN_POINT('',(-4.49069170170099,0.,6.57452478769713));
#35188=CARTESIAN_POINT('',(-12.8347835106019,0.,3.9));
#35189=CARTESIAN_POINT('',(-13.9,0.,3.9));
#35190=CARTESIAN_POINT('',(-15.509308298299,0.,6.57452478769712));
#35191=CARTESIAN_POINT('',(-15.509308298299,0.,6.57452478769712));
#35192=CARTESIAN_POINT('',(-15.509308298299,0.,8.19999999999999));
#35193=CARTESIAN_POINT('',(-15.509308298299,0.,8.19999999999999));
#35194=CARTESIAN_POINT('',(-13.1,0.,8.2));
#35195=CARTESIAN_POINT('',(-15.509308298299,0.,8.19999999999999));
#35196=CARTESIAN_POINT('',(-13.1,0.,8.52106159959513));
#35197=CARTESIAN_POINT('',(-13.1,0.,8.2));
#35198=CARTESIAN_POINT('',(-14.5789384004049,0.,10.));
#35199=CARTESIAN_POINT('',(-14.5789384004049,0.,10.));
#35200=CARTESIAN_POINT('',(-19.5,0.,9.99999999999999));
#35201=CARTESIAN_POINT('',(-19.5,0.,9.99999999999999));
#35202=CARTESIAN_POINT('',(-20.,0.,9.49999999999999));
#35203=CARTESIAN_POINT('Origin',(-19.5,0.,9.49999999999999));
#35204=CARTESIAN_POINT('',(-20.,0.,4.57893840040487));
#35205=CARTESIAN_POINT('',(-20.,0.,4.57893840040487));
#35206=CARTESIAN_POINT('',(-18.5210615995951,0.,3.1));
#35207=CARTESIAN_POINT('',(-20.,0.,4.57893840040487));
#35208=CARTESIAN_POINT('',(-18.2,0.,3.1));
#35209=CARTESIAN_POINT('',(-18.2,0.,3.1));
#35210=CARTESIAN_POINT('',(-18.2,0.,5.50930829829901));
#35211=CARTESIAN_POINT('',(-18.2,0.,5.50930829829901));
#35212=CARTESIAN_POINT('',(-16.5745247876971,0.,5.50930829829901));
#35213=CARTESIAN_POINT('',(-18.2,0.,5.50930829829901));
#35214=CARTESIAN_POINT('',(-13.9,0.,2.83478351060189));
#35215=CARTESIAN_POINT('',(-16.5745247876971,0.,5.50930829829901));
#35216=CARTESIAN_POINT('',(-13.9,0.,-2.83478351060189));
#35217=CARTESIAN_POINT('',(-13.9,0.,-3.9));
#35218=CARTESIAN_POINT('',(-16.5745247876971,0.,-5.50930829829902));
#35219=CARTESIAN_POINT('',(-16.5745247876971,0.,-5.50930829829902));
#35220=CARTESIAN_POINT('',(-18.2,0.,-5.50930829829902));
#35221=CARTESIAN_POINT('',(-18.2,0.,-5.50930829829902));
#35222=CARTESIAN_POINT('',(-18.2,0.,-3.1));
#35223=CARTESIAN_POINT('',(-18.2,0.,-5.50930829829902));
#35224=CARTESIAN_POINT('',(-18.5210615995951,0.,-3.1));
#35225=CARTESIAN_POINT('',(-18.2,0.,-3.1));
#35226=CARTESIAN_POINT('',(-20.,0.,-4.57893840040487));
#35227=CARTESIAN_POINT('',(-20.,0.,-4.57893840040487));
#35228=CARTESIAN_POINT('',(-20.,0.,-9.5));
#35229=CARTESIAN_POINT('',(-20.,0.,-9.5));
#35230=CARTESIAN_POINT('',(-19.5,0.,-10.));
#35231=CARTESIAN_POINT('Origin',(-19.5,0.,-9.49999999999999));
#35232=CARTESIAN_POINT('',(-14.5789384004049,0.,-10.));
#35233=CARTESIAN_POINT('',(-14.5789384004049,0.,-10.));
#35234=CARTESIAN_POINT('',(-13.1,0.,-8.52106159959513));
#35235=CARTESIAN_POINT('',(-14.5789384004049,0.,-10.));
#35236=CARTESIAN_POINT('',(-13.1,0.,-8.2));
#35237=CARTESIAN_POINT('',(-13.1,0.,-8.2));
#35238=CARTESIAN_POINT('',(-15.509308298299,0.,-8.2));
#35239=CARTESIAN_POINT('',(-15.509308298299,0.,-8.2));
#35240=CARTESIAN_POINT('',(-15.509308298299,0.,-6.57452478769713));
#35241=CARTESIAN_POINT('',(-15.509308298299,0.,-8.2));
#35242=CARTESIAN_POINT('',(-12.8347835106019,0.,-3.9));
#35243=CARTESIAN_POINT('',(-15.509308298299,0.,-6.57452478769713));
#35244=CARTESIAN_POINT('',(-7.16521648939811,0.,-3.9));
#35245=CARTESIAN_POINT('',(-6.1,0.,-3.9));
#35246=CARTESIAN_POINT('',(-4.49069170170098,0.,-6.57452478769712));
#35247=CARTESIAN_POINT('',(-4.49069170170098,0.,-6.57452478769712));
#35248=CARTESIAN_POINT('',(-4.49069170170098,0.,-8.19999999999999));
#35249=CARTESIAN_POINT('',(-4.49069170170098,0.,-8.19999999999999));
#35250=CARTESIAN_POINT('',(-6.9,0.,-8.2));
#35251=CARTESIAN_POINT('',(-4.49069170170098,0.,-8.19999999999999));
#35252=CARTESIAN_POINT('',(-6.9,0.,-8.52106159959513));
#35253=CARTESIAN_POINT('',(-6.9,0.,-8.2));
#35254=CARTESIAN_POINT('',(-5.42106159959513,0.,-9.99999999999999));
#35255=CARTESIAN_POINT('',(-6.1,0.,-2.83478351060189));
#35256=CARTESIAN_POINT('',(-3.42547521230287,0.,-5.50930829829901));
#35257=CARTESIAN_POINT('',(-6.1,0.,2.83478351060189));
#35258=CARTESIAN_POINT('',(-6.1,0.,3.9));
#35259=CARTESIAN_POINT('',(-2.69069170170098,0.,6.24409180890091));
#35260=CARTESIAN_POINT('',(-3.42547521230288,0.,5.50930829829902));
#35261=CARTESIAN_POINT('',(-2.69069170170098,0.,8.2));
#35262=CARTESIAN_POINT('',(-2.69069170170098,0.,-0.0866499732000181));
#35263=CARTESIAN_POINT('',(-3.13664997320002,0.,8.2));
#35264=CARTESIAN_POINT('',(-12.1,0.,2.57175827820944E-16));
#35265=CARTESIAN_POINT('Origin',(-10.,0.,0.));
#35266=CARTESIAN_POINT('Origin',(-2.69069170170098,0.,8.2));
#35267=CARTESIAN_POINT('',(-2.69069170170098,500.,8.2));
#35268=CARTESIAN_POINT('',(-2.69069170170098,0.,8.2));
#35269=CARTESIAN_POINT('',(-3.13664997320002,500.,8.2));
#35270=CARTESIAN_POINT('Origin',(-2.69069170170098,0.,6.24409180890091));
#35271=CARTESIAN_POINT('',(-2.69069170170098,500.,6.24409180890091));
#35272=CARTESIAN_POINT('',(-2.69069170170098,0.,6.24409180890091));
#35273=CARTESIAN_POINT('',(-2.69069170170098,500.,-0.0866499732000181));
#35274=CARTESIAN_POINT('Origin',(-6.1,0.,3.9));
#35275=CARTESIAN_POINT('',(-6.1,500.,-2.83478351060189));
#35276=CARTESIAN_POINT('',(-6.1,0.,-2.83478351060189));
#35277=CARTESIAN_POINT('',(-6.1,500.,2.83478351060189));
#35278=CARTESIAN_POINT('',(-6.1,500.,-1.25869587765047));
#35279=CARTESIAN_POINT('',(-6.1,0.,2.83478351060189));
#35280=CARTESIAN_POINT('Origin',(-13.9,0.,3.9));
#35281=CARTESIAN_POINT('',(-12.8347835106019,500.,3.9));
#35282=CARTESIAN_POINT('',(-12.8347835106019,0.,3.9));
#35283=CARTESIAN_POINT('',(-7.16521648939811,500.,3.9));
#35284=CARTESIAN_POINT('',(-7.16521648939811,0.,3.9));
#35285=CARTESIAN_POINT('',(-8.74130412234953,500.,3.9));
#35286=CARTESIAN_POINT('Origin',(-13.9,0.,-3.9));
#35287=CARTESIAN_POINT('',(-13.9,500.,2.83478351060189));
#35288=CARTESIAN_POINT('',(-13.9,0.,2.83478351060189));
#35289=CARTESIAN_POINT('',(-13.9,500.,-2.83478351060189));
#35290=CARTESIAN_POINT('',(-13.9,500.,-5.15869587765047));
#35291=CARTESIAN_POINT('',(-13.9,0.,-2.83478351060189));
#35292=CARTESIAN_POINT('Origin',(-10.,0.,0.));
#35293=CARTESIAN_POINT('',(-12.1,500.,-2.57175827820944E-16));
#35294=CARTESIAN_POINT('',(-12.1,0.,2.57175827820944E-16));
#35295=CARTESIAN_POINT('Origin',(-10.,500.,0.));
#35296=CARTESIAN_POINT('Origin',(-6.1,0.,-3.9));
#35297=CARTESIAN_POINT('',(-7.16521648939811,500.,-3.9));
#35298=CARTESIAN_POINT('',(-7.16521648939811,0.,-3.9));
#35299=CARTESIAN_POINT('',(-12.8347835106019,500.,-3.9));
#35300=CARTESIAN_POINT('',(-12.8347835106019,0.,-3.9));
#35301=CARTESIAN_POINT('',(-4.84130412234953,500.,-3.9));
#35302=CARTESIAN_POINT('Origin',(-15.509308298299,0.,-6.57452478769713));
#35303=CARTESIAN_POINT('',(-15.509308298299,500.,-8.2));
#35304=CARTESIAN_POINT('',(-15.509308298299,0.,-8.2));
#35305=CARTESIAN_POINT('',(-15.509308298299,500.,-6.57452478769713));
#35306=CARTESIAN_POINT('',(-15.509308298299,500.,-6.49595827149903));
#35307=CARTESIAN_POINT('',(-15.509308298299,0.,-6.57452478769713));
#35308=CARTESIAN_POINT('Origin',(-12.8347835106019,0.,-3.9));
#35309=CARTESIAN_POINT('',(-11.1510876329514,500.,-2.21630412234953));
#35310=CARTESIAN_POINT('Origin',(-16.5745247876971,0.,-5.50930829829902));
#35311=CARTESIAN_POINT('',(-16.5745247876971,500.,-5.50930829829902));
#35312=CARTESIAN_POINT('',(-13.5535665161981,500.,-2.48835002679998));
#35313=CARTESIAN_POINT('',(-16.5745247876971,0.,-5.50930829829902));
#35314=CARTESIAN_POINT('Origin',(-18.2,0.,-5.50930829829902));
#35315=CARTESIAN_POINT('',(-18.2,500.,-5.50930829829902));
#35316=CARTESIAN_POINT('',(-10.8913041223495,500.,-5.50930829829901));
#35317=CARTESIAN_POINT('',(-18.2,0.,-5.50930829829902));
#35318=CARTESIAN_POINT('Origin',(-18.2,0.,-3.1));
#35319=CARTESIAN_POINT('',(-18.2,500.,-3.1));
#35320=CARTESIAN_POINT('',(-18.2,500.,-4.75869587765048));
#35321=CARTESIAN_POINT('',(-18.2,0.,-3.1));
#35322=CARTESIAN_POINT('Origin',(-18.5210615995951,0.,-3.1));
#35323=CARTESIAN_POINT('',(-18.5210615995951,500.,-3.1));
#35324=CARTESIAN_POINT('',(-11.0518349221471,500.,-3.1));
#35325=CARTESIAN_POINT('',(-18.5210615995951,0.,-3.1));
#35326=CARTESIAN_POINT('Origin',(-20.,0.,-4.57893840040487));
#35327=CARTESIAN_POINT('',(-20.,500.,-4.57893840040487));
#35328=CARTESIAN_POINT('',(-16.3552653998988,500.,-0.934203800303655));
#35329=CARTESIAN_POINT('',(-20.,0.,-4.57893840040487));
#35330=CARTESIAN_POINT('Origin',(-20.,0.,-9.5));
#35331=CARTESIAN_POINT('',(-20.,500.,-9.5));
#35332=CARTESIAN_POINT('',(-20.,500.,-7.95869587765048));
#35333=CARTESIAN_POINT('',(-20.,0.,-9.5));
#35334=CARTESIAN_POINT('Origin',(-19.5,0.,-9.49999999999999));
#35335=CARTESIAN_POINT('',(-19.5,500.,-10.));
#35336=CARTESIAN_POINT('Origin',(-19.5,500.,-9.49999999999999));
#35337=CARTESIAN_POINT('',(-19.5,0.,-10.));
#35338=CARTESIAN_POINT('Origin',(-14.5789384004049,0.,-10.));
#35339=CARTESIAN_POINT('',(-14.5789384004049,500.,-10.));
#35340=CARTESIAN_POINT('',(-9.08077332255196,500.,-9.99999999999999));
#35341=CARTESIAN_POINT('',(-14.5789384004049,0.,-10.));
#35342=CARTESIAN_POINT('Origin',(-13.1,0.,-8.52106159959513));
#35343=CARTESIAN_POINT('',(-13.1,500.,-8.52106159959513));
#35344=CARTESIAN_POINT('',(-10.1947346001012,500.,-5.61579619969635));
#35345=CARTESIAN_POINT('',(-13.1,0.,-8.52106159959513));
#35346=CARTESIAN_POINT('Origin',(-13.1,0.,-8.2));
#35347=CARTESIAN_POINT('',(-13.1,500.,-8.2));
#35348=CARTESIAN_POINT('',(-13.1,500.,-7.30869587765047));
#35349=CARTESIAN_POINT('',(-13.1,0.,-8.2));
#35350=CARTESIAN_POINT('Origin',(-15.509308298299,0.,-8.2));
#35351=CARTESIAN_POINT('',(-9.54595827149904,500.,-8.2));
#35352=CARTESIAN_POINT('Origin',(-4.49069170170099,0.,6.57452478769713));
#35353=CARTESIAN_POINT('',(-4.49069170170099,500.,8.2));
#35354=CARTESIAN_POINT('',(-4.49069170170099,0.,8.2));
#35355=CARTESIAN_POINT('',(-4.49069170170099,500.,6.57452478769713));
#35356=CARTESIAN_POINT('',(-4.49069170170098,500.,0.0785665161980925));
#35357=CARTESIAN_POINT('',(-4.49069170170099,0.,6.57452478769713));
#35358=CARTESIAN_POINT('Origin',(-7.16521648939811,0.,3.9));
#35359=CARTESIAN_POINT('',(-8.84891236704858,500.,2.21630412234953));
#35360=CARTESIAN_POINT('Origin',(-3.42547521230288,0.,5.50930829829902));
#35361=CARTESIAN_POINT('',(-6.44643348380191,500.,2.48835002679998));
#35362=CARTESIAN_POINT('Origin',(-5.42106159959513,0.,10.));
#35363=CARTESIAN_POINT('',(-5.42106159959513,500.,10.));
#35364=CARTESIAN_POINT('',(-4.5018349221471,500.,10.));
#35365=CARTESIAN_POINT('',(-5.42106159959513,0.,10.));
#35366=CARTESIAN_POINT('Origin',(-6.9,0.,8.52106159959513));
#35367=CARTESIAN_POINT('',(-6.9,500.,8.52106159959513));
#35368=CARTESIAN_POINT('',(-9.80526539989878,500.,5.61579619969636));
#35369=CARTESIAN_POINT('',(-6.9,0.,8.52106159959513));
#35370=CARTESIAN_POINT('Origin',(-6.9,0.,8.2));
#35371=CARTESIAN_POINT('',(-6.9,500.,8.2));
#35372=CARTESIAN_POINT('',(-6.9,500.,0.891304122349527));
#35373=CARTESIAN_POINT('',(-6.9,0.,8.2));
#35374=CARTESIAN_POINT('Origin',(-4.49069170170099,0.,8.2));
#35375=CARTESIAN_POINT('',(-4.03664997320002,500.,8.2));
#35376=CARTESIAN_POINT('Origin',(-16.5745247876971,0.,5.50930829829901));
#35377=CARTESIAN_POINT('',(-18.2,500.,5.50930829829901));
#35378=CARTESIAN_POINT('',(-18.2,0.,5.50930829829901));
#35379=CARTESIAN_POINT('',(-16.5745247876971,500.,5.50930829829901));
#35380=CARTESIAN_POINT('',(-10.0785665161981,500.,5.50930829829901));
#35381=CARTESIAN_POINT('',(-16.5745247876971,0.,5.50930829829901));
#35382=CARTESIAN_POINT('Origin',(-13.9,0.,2.83478351060189));
#35383=CARTESIAN_POINT('',(-9.00760824469906,500.,-2.05760824469905));
#35384=CARTESIAN_POINT('Origin',(-15.509308298299,0.,6.57452478769712));
#35385=CARTESIAN_POINT('',(-15.509308298299,500.,6.57452478769712));
#35386=CARTESIAN_POINT('',(-9.27965414914951,500.,0.34487063854762));
#35387=CARTESIAN_POINT('',(-15.509308298299,0.,6.57452478769712));
#35388=CARTESIAN_POINT('Origin',(-15.509308298299,0.,8.19999999999999));
#35389=CARTESIAN_POINT('',(-15.509308298299,500.,8.19999999999999));
#35390=CARTESIAN_POINT('',(-15.509308298299,500.,0.891304122349518));
#35391=CARTESIAN_POINT('',(-15.509308298299,0.,8.19999999999999));
#35392=CARTESIAN_POINT('Origin',(-13.1,0.,8.2));
#35393=CARTESIAN_POINT('',(-13.1,500.,8.2));
#35394=CARTESIAN_POINT('',(-8.34130412234954,500.,8.2));
#35395=CARTESIAN_POINT('',(-13.1,0.,8.2));
#35396=CARTESIAN_POINT('Origin',(-13.1,0.,8.52106159959513));
#35397=CARTESIAN_POINT('',(-13.1,500.,8.52106159959513));
#35398=CARTESIAN_POINT('',(-13.1,500.,1.05183492214709));
#35399=CARTESIAN_POINT('',(-13.1,0.,8.52106159959513));
#35400=CARTESIAN_POINT('Origin',(-14.5789384004049,0.,10.));
#35401=CARTESIAN_POINT('',(-14.5789384004049,500.,10.));
#35402=CARTESIAN_POINT('',(-7.72550792265318,500.,3.14656952224831));
#35403=CARTESIAN_POINT('',(-14.5789384004049,0.,10.));
#35404=CARTESIAN_POINT('Origin',(-19.5,0.,9.99999999999999));
#35405=CARTESIAN_POINT('',(-19.5,500.,9.99999999999999));
#35406=CARTESIAN_POINT('',(-11.5413041223495,500.,10.));
#35407=CARTESIAN_POINT('',(-19.5,0.,9.99999999999999));
#35408=CARTESIAN_POINT('Origin',(-19.5,0.,9.49999999999999));
#35409=CARTESIAN_POINT('',(-20.,500.,9.49999999999999));
#35410=CARTESIAN_POINT('Origin',(-19.5,500.,9.49999999999999));
#35411=CARTESIAN_POINT('',(-20.,0.,9.49999999999999));
#35412=CARTESIAN_POINT('Origin',(-20.,0.,4.57893840040487));
#35413=CARTESIAN_POINT('',(-20.,500.,4.57893840040487));
#35414=CARTESIAN_POINT('',(-20.,500.,-0.919226677448038));
#35415=CARTESIAN_POINT('',(-20.,0.,4.57893840040487));
#35416=CARTESIAN_POINT('Origin',(-18.5210615995951,0.,3.1));
#35417=CARTESIAN_POINT('',(-18.5210615995951,500.,3.1));
#35418=CARTESIAN_POINT('',(-12.4071003220459,500.,-3.01396127754926));
#35419=CARTESIAN_POINT('',(-18.5210615995951,0.,3.1));
#35420=CARTESIAN_POINT('Origin',(-18.2,0.,3.1));
#35421=CARTESIAN_POINT('',(-18.2,500.,3.1));
#35422=CARTESIAN_POINT('',(-10.8913041223495,500.,3.1));
#35423=CARTESIAN_POINT('',(-18.2,0.,3.1));
#35424=CARTESIAN_POINT('Origin',(-18.2,0.,5.50930829829901));
#35425=CARTESIAN_POINT('',(-18.2,500.,-0.454041728500963));
#35426=CARTESIAN_POINT('Origin',(-6.1,0.,-2.83478351060189));
#35427=CARTESIAN_POINT('',(-4.575,500.,-4.35978351060189));
#35428=CARTESIAN_POINT('Origin',(-4.49069170170098,0.,-6.57452478769712));
#35429=CARTESIAN_POINT('',(-4.49069170170098,500.,-6.57452478769712));
#35430=CARTESIAN_POINT('',(-4.30295409554955,500.,-6.76226239384856));
#35431=CARTESIAN_POINT('',(-4.49069170170098,0.,-6.57452478769712));
#35432=CARTESIAN_POINT('Origin',(-4.49069170170098,0.,-8.19999999999999));
#35433=CARTESIAN_POINT('',(-4.49069170170098,500.,-8.19999999999999));
#35434=CARTESIAN_POINT('',(-4.49069170170098,500.,-7.30869587765047));
#35435=CARTESIAN_POINT('',(-4.49069170170098,0.,-8.19999999999999));
#35436=CARTESIAN_POINT('Origin',(-6.9,0.,-8.2));
#35437=CARTESIAN_POINT('',(-6.9,500.,-8.2));
#35438=CARTESIAN_POINT('',(-5.24130412234953,500.,-8.19999999999999));
#35439=CARTESIAN_POINT('',(-6.9,0.,-8.2));
#35440=CARTESIAN_POINT('Origin',(-6.9,0.,-8.52106159959513));
#35441=CARTESIAN_POINT('',(-6.9,500.,-8.52106159959513));
#35442=CARTESIAN_POINT('',(-6.9,500.,-7.46922667744804));
#35443=CARTESIAN_POINT('',(-6.9,0.,-8.52106159959513));
#35444=CARTESIAN_POINT('Origin',(-5.42106159959513,0.,-9.99999999999999));
#35445=CARTESIAN_POINT('',(-5.42106159959513,500.,-9.99999999999999));
#35446=CARTESIAN_POINT('',(-5.85710032204587,500.,-9.56396127754925));
#35447=CARTESIAN_POINT('',(-5.42106159959513,0.,-9.99999999999999));
#35448=CARTESIAN_POINT('Origin',(-0.500000000000003,0.,-9.99999999999999));
#35449=CARTESIAN_POINT('',(-2.04130412234953,500.,-9.99999999999999));
#35450=CARTESIAN_POINT('Origin',(-3.58260824469906,500.,-6.41739175530094));
#35451=CARTESIAN_POINT('',(0.,0.,0.));
#35452=CARTESIAN_POINT('Origin',(-10.,520.056498641762,4.99200000000021));
#35453=CARTESIAN_POINT('',(-20.75,520.056498641762,4.99200000000021));
#35454=CARTESIAN_POINT('Origin',(-10.,520.056498641762,4.99200000000021));
#35455=CARTESIAN_POINT('',(-13.175,520.056498641762,4.99200000000021));
#35456=CARTESIAN_POINT('Origin',(-9.99999999999998,520.056498641762,4.99200000000021));
#35457=CARTESIAN_POINT('Origin',(-9.99999999999996,520.056498641762,-3.50799999999979));
#35458=CARTESIAN_POINT('',(-19.15,520.056498641762,3.49200000000021));
#35459=CARTESIAN_POINT('Origin',(-9.99999999999996,520.056498641762,3.49200000000021));
#35460=CARTESIAN_POINT('',(-19.15,520.056498641762,-4.00799999999979));
#35461=CARTESIAN_POINT('',(-19.15,520.056498641762,-3.50799999999979));
#35462=CARTESIAN_POINT('Origin',(-9.99999999999996,520.056498641762,-4.00799999999979));
#35463=CARTESIAN_POINT('Origin',(-10.,520.056498641762,-4.00799999999979));
#35464=CARTESIAN_POINT('',(-20.75,520.056498641762,-4.00799999999979));
#35465=CARTESIAN_POINT('Origin',(-10.,520.056498641762,-4.00799999999979));
#35466=CARTESIAN_POINT('Origin',(-10.,520.056498641762,3.49200000000021));
#35467=CARTESIAN_POINT('',(-20.75,520.056498641762,3.49200000000021));
#35468=CARTESIAN_POINT('Origin',(-10.,520.056498641762,3.49200000000021));
#35469=CARTESIAN_POINT('Origin',(-10.,520.056498641762,-3.50799999999979));
#35470=CARTESIAN_POINT('',(-20.75,520.056498641762,-9.50799999999979));
#35471=CARTESIAN_POINT('',(-20.75,520.056498641762,-3.50799999999979));
#35472=CARTESIAN_POINT('Origin',(-10.,520.056498641762,-9.50799999999979));
#35473=CARTESIAN_POINT('Origin',(-10.,520.056498641762,3.49200000000021));
#35474=CARTESIAN_POINT('',(-20.75,520.056498641762,3.49200000000021));
#35475=CARTESIAN_POINT('Origin',(-10.,520.056498641762,-9.50799999999979));
#35476=CARTESIAN_POINT('',(-13.175,520.056498641762,-9.50799999999979));
#35477=CARTESIAN_POINT('Origin',(-9.99999999999998,520.056498641762,-9.50799999999979));
#35478=CARTESIAN_POINT('Origin',(-9.99999999999998,520.056498641762,-3.50799999999979));
#35479=CARTESIAN_POINT('',(-13.175,520.056498641762,-3.50799999999979));
#35480=CARTESIAN_POINT('',(0.,0.,0.));
#35481=CARTESIAN_POINT('Origin',(-25.5,-48.4435013582375,-10.));
#35482=CARTESIAN_POINT('',(-23.345,-48.4435013582375,-10.));
#35483=CARTESIAN_POINT('Origin',(-25.5,-48.4435013582375,-10.));
#35484=CARTESIAN_POINT('',(-23.345,-48.4435013582375,-13.));
#35485=CARTESIAN_POINT('',(-23.345,-48.4435013582375,-10.));
#35486=CARTESIAN_POINT('Origin',(-25.5,-48.4435013582375,-13.));
#35487=CARTESIAN_POINT('Origin',(-27.1652164893981,4.65750316817282,-10.));
#35488=CARTESIAN_POINT('',(-27.1652164893981,4.65750316817282,-10.));
#35489=CARTESIAN_POINT('',(-27.1652164893981,30.6870120381804,-10.));
#35490=CARTESIAN_POINT('',(-27.1652164893981,30.6870120381804,-10.));
#35491=CARTESIAN_POINT('',(-27.1652164893981,30.6870120381804,-13.));
#35492=CARTESIAN_POINT('',(-27.1652164893981,30.6870120381804,-10.));
#35493=CARTESIAN_POINT('',(-27.1652164893981,4.65750316817282,-13.));
#35494=CARTESIAN_POINT('',(-27.1652164893981,30.6870120381804,-13.));
#35495=CARTESIAN_POINT('',(-27.1652164893981,4.65750316817282,-10.));
#35496=CARTESIAN_POINT('Origin',(-32.8347835106019,4.65750316817282,-10.));
#35497=CARTESIAN_POINT('',(-32.8347835106019,4.65750316817282,-10.));
#35498=CARTESIAN_POINT('',(-27.1652164893981,4.65750316817282,-10.));
#35499=CARTESIAN_POINT('',(-32.8347835106019,4.65750316817282,-13.));
#35500=CARTESIAN_POINT('',(-27.1652164893981,4.65750316817282,-13.));
#35501=CARTESIAN_POINT('',(-32.8347835106019,4.65750316817282,-10.));
#35502=CARTESIAN_POINT('Origin',(-32.8347835106019,30.6870120381804,-10.));
#35503=CARTESIAN_POINT('',(-32.8347835106019,30.6870120381804,-10.));
#35504=CARTESIAN_POINT('',(-32.8347835106019,4.65750316817282,-10.));
#35505=CARTESIAN_POINT('',(-32.8347835106019,30.6870120381804,-13.));
#35506=CARTESIAN_POINT('',(-32.8347835106019,4.65750316817282,-13.));
#35507=CARTESIAN_POINT('',(-32.8347835106019,30.6870120381804,-10.));
#35508=CARTESIAN_POINT('Origin',(-27.1652164893981,30.6870120381804,-10.));
#35509=CARTESIAN_POINT('',(-32.8347835106019,30.6870120381804,-10.));
#35510=CARTESIAN_POINT('',(-32.8347835106019,30.6870120381804,-13.));
#35511=CARTESIAN_POINT('Origin',(2.83478351060189,4.65750316817282,-9.99999999999999));
#35512=CARTESIAN_POINT('',(2.83478351060189,4.65750316817282,-9.99999999999999));
#35513=CARTESIAN_POINT('',(2.83478351060189,30.6870120381804,-9.99999999999999));
#35514=CARTESIAN_POINT('',(2.83478351060189,30.6870120381804,-9.99999999999999));
#35515=CARTESIAN_POINT('',(2.83478351060189,30.6870120381804,-13.));
#35516=CARTESIAN_POINT('',(2.83478351060189,30.6870120381804,-9.99999999999999));
#35517=CARTESIAN_POINT('',(2.83478351060189,4.65750316817282,-13.));
#35518=CARTESIAN_POINT('',(2.8347835106019,30.6870120381804,-13.));
#35519=CARTESIAN_POINT('',(2.83478351060189,4.65750316817282,-9.99999999999999));
#35520=CARTESIAN_POINT('Origin',(-2.83478351060189,4.65750316817282,-9.99999999999999));
#35521=CARTESIAN_POINT('',(-2.83478351060189,4.65750316817282,-9.99999999999999));
#35522=CARTESIAN_POINT('',(2.83478351060189,4.65750316817282,-9.99999999999999));
#35523=CARTESIAN_POINT('',(-2.83478351060189,4.65750316817282,-13.));
#35524=CARTESIAN_POINT('',(2.8347835106019,4.65750316817282,-13.));
#35525=CARTESIAN_POINT('',(-2.83478351060189,4.65750316817282,-9.99999999999999));
#35526=CARTESIAN_POINT('Origin',(-2.83478351060189,30.6870120381804,-9.99999999999999));
#35527=CARTESIAN_POINT('',(-2.83478351060189,30.6870120381804,-9.99999999999999));
#35528=CARTESIAN_POINT('',(-2.83478351060189,4.65750316817282,-9.99999999999999));
#35529=CARTESIAN_POINT('',(-2.83478351060189,30.6870120381804,-13.));
#35530=CARTESIAN_POINT('',(-2.83478351060189,4.65750316817282,-13.));
#35531=CARTESIAN_POINT('',(-2.83478351060189,30.6870120381804,-9.99999999999999));
#35532=CARTESIAN_POINT('Origin',(2.83478351060189,30.6870120381804,-9.99999999999999));
#35533=CARTESIAN_POINT('',(-2.83478351060189,30.6870120381804,-9.99999999999999));
#35534=CARTESIAN_POINT('',(-2.83478351060189,30.6870120381804,-13.));
#35535=CARTESIAN_POINT('Origin',(5.50000000000001,-48.4435013582379,-9.99999999999999));
#35536=CARTESIAN_POINT('',(7.65500000000001,-48.4435013582379,-9.99999999999999));
#35537=CARTESIAN_POINT('Origin',(5.50000000000001,-48.4435013582379,-9.99999999999999));
#35538=CARTESIAN_POINT('',(7.65500000000001,-48.4435013582379,-13.));
#35539=CARTESIAN_POINT('',(7.65500000000001,-48.4435013582379,-9.99999999999999));
#35540=CARTESIAN_POINT('Origin',(5.50000000000001,-48.4435013582379,-13.));
#35541=CARTESIAN_POINT('Origin',(5.50000000000001,-17.4435013582379,-9.99999999999999));
#35542=CARTESIAN_POINT('',(7.65500000000001,-17.4435013582379,-9.99999999999999));
#35543=CARTESIAN_POINT('Origin',(5.50000000000001,-17.4435013582379,-9.99999999999999));
#35544=CARTESIAN_POINT('',(7.65500000000001,-17.4435013582379,-13.));
#35545=CARTESIAN_POINT('',(7.65500000000001,-17.4435013582379,-9.99999999999999));
#35546=CARTESIAN_POINT('Origin',(5.50000000000001,-17.4435013582379,-13.));
#35547=CARTESIAN_POINT('Origin',(-17.1652164893981,4.65750316817282,-10.));
#35548=CARTESIAN_POINT('',(-17.1652164893981,4.65750316817282,-10.));
#35549=CARTESIAN_POINT('',(-17.1652164893981,30.6870120381804,-10.));
#35550=CARTESIAN_POINT('',(-17.1652164893981,30.6870120381804,-10.));
#35551=CARTESIAN_POINT('',(-17.1652164893981,30.6870120381804,-13.));
#35552=CARTESIAN_POINT('',(-17.1652164893981,30.6870120381804,-10.));
#35553=CARTESIAN_POINT('',(-17.1652164893981,4.65750316817282,-13.));
#35554=CARTESIAN_POINT('',(-17.1652164893981,30.6870120381804,-13.));
#35555=CARTESIAN_POINT('',(-17.1652164893981,4.65750316817282,-10.));
#35556=CARTESIAN_POINT('Origin',(-22.8347835106019,4.65750316817282,-10.));
#35557=CARTESIAN_POINT('',(-22.8347835106019,4.65750316817282,-10.));
#35558=CARTESIAN_POINT('',(-17.1652164893981,4.65750316817282,-10.));
#35559=CARTESIAN_POINT('',(-22.8347835106019,4.65750316817282,-13.));
#35560=CARTESIAN_POINT('',(-17.1652164893981,4.65750316817282,-13.));
#35561=CARTESIAN_POINT('',(-22.8347835106019,4.65750316817282,-10.));
#35562=CARTESIAN_POINT('Origin',(-22.8347835106019,30.6870120381804,-10.));
#35563=CARTESIAN_POINT('',(-22.8347835106019,30.6870120381804,-10.));
#35564=CARTESIAN_POINT('',(-22.8347835106019,4.65750316817282,-10.));
#35565=CARTESIAN_POINT('',(-22.8347835106019,30.6870120381804,-13.));
#35566=CARTESIAN_POINT('',(-22.8347835106019,4.65750316817282,-13.));
#35567=CARTESIAN_POINT('',(-22.8347835106019,30.6870120381804,-10.));
#35568=CARTESIAN_POINT('Origin',(-17.1652164893981,30.6870120381804,-10.));
#35569=CARTESIAN_POINT('',(-22.8347835106019,30.6870120381804,-10.));
#35570=CARTESIAN_POINT('',(-22.8347835106019,30.6870120381804,-13.));
#35571=CARTESIAN_POINT('Origin',(-10.,-32.9435013582377,-10.));
#35572=CARTESIAN_POINT('',(1.493,-32.9435013582377,-9.99999999999999));
#35573=CARTESIAN_POINT('Origin',(-10.,-32.9435013582377,-10.));
#35574=CARTESIAN_POINT('',(1.493,-32.9435013582377,-13.));
#35575=CARTESIAN_POINT('',(1.493,-32.9435013582377,-9.99999999999999));
#35576=CARTESIAN_POINT('Origin',(-9.99999999999999,-32.9435013582377,-13.));
#35577=CARTESIAN_POINT('Origin',(-25.5,-17.4435013582375,-10.));
#35578=CARTESIAN_POINT('',(-23.345,-17.4435013582375,-10.));
#35579=CARTESIAN_POINT('Origin',(-25.5,-17.4435013582375,-10.));
#35580=CARTESIAN_POINT('',(-23.345,-17.4435013582375,-13.));
#35581=CARTESIAN_POINT('',(-23.345,-17.4435013582375,-10.));
#35582=CARTESIAN_POINT('Origin',(-25.5,-17.4435013582375,-13.));
#35583=CARTESIAN_POINT('Origin',(12.8347835106019,35.2970569134824,-9.99999999999998));
#35584=CARTESIAN_POINT('',(15.,35.2970569134824,-9.99999999999998));
#35585=CARTESIAN_POINT('',(12.8347835106019,35.2970569134824,-9.99999999999998));
#35586=CARTESIAN_POINT('',(15.,35.2970569134824,-9.99999999999998));
#35587=CARTESIAN_POINT('',(15.,35.2970569134824,-13.));
#35588=CARTESIAN_POINT('',(15.,35.2970569134824,-9.99999999999998));
#35589=CARTESIAN_POINT('',(12.8347835106019,35.2970569134824,-13.));
#35590=CARTESIAN_POINT('',(15.,35.2970569134824,-13.));
#35591=CARTESIAN_POINT('',(12.8347835106019,35.2970569134824,-9.99999999999998));
#35592=CARTESIAN_POINT('Origin',(12.8347835106019,0.,-9.99999999999998));
#35593=CARTESIAN_POINT('',(12.8347835106019,0.,-9.99999999999998));
#35594=CARTESIAN_POINT('',(12.8347835106019,500.,-9.99999999999998));
#35595=CARTESIAN_POINT('',(12.8347835106019,0.,-13.));
#35596=CARTESIAN_POINT('',(12.8347835106019,500.,-13.));
#35597=CARTESIAN_POINT('',(12.8347835106019,0.,-9.99999999999998));
#35598=CARTESIAN_POINT('Origin',(7.16521648939811,0.,-9.99999999999999));
#35599=CARTESIAN_POINT('',(7.16521648939811,0.,-9.99999999999999));
#35600=CARTESIAN_POINT('',(12.8347835106019,0.,-9.99999999999998));
#35601=CARTESIAN_POINT('',(7.16521648939812,0.,-13.));
#35602=CARTESIAN_POINT('',(12.8347835106019,0.,-13.));
#35603=CARTESIAN_POINT('',(7.16521648939811,0.,-9.99999999999999));
#35604=CARTESIAN_POINT('Origin',(7.16521648939811,35.2970569134824,-9.99999999999999));
#35605=CARTESIAN_POINT('',(7.16521648939811,35.2970569134824,-9.99999999999999));
#35606=CARTESIAN_POINT('',(7.16521648939811,0.,-9.99999999999999));
#35607=CARTESIAN_POINT('',(7.16521648939812,35.2970569134824,-13.));
#35608=CARTESIAN_POINT('',(7.16521648939812,0.,-13.));
#35609=CARTESIAN_POINT('',(7.16521648939811,35.2970569134824,-9.99999999999999));
#35610=CARTESIAN_POINT('Origin',(-7.16521648939811,35.2970569134824,-10.));
#35611=CARTESIAN_POINT('',(-7.16521648939811,35.2970569134824,-10.));
#35612=CARTESIAN_POINT('',(15.,35.2970569134824,-9.99999999999998));
#35613=CARTESIAN_POINT('',(-7.16521648939811,35.2970569134824,-13.));
#35614=CARTESIAN_POINT('',(15.,35.2970569134824,-13.));
#35615=CARTESIAN_POINT('',(-7.16521648939811,35.2970569134824,-10.));
#35616=CARTESIAN_POINT('Origin',(-7.16521648939811,0.,-10.));
#35617=CARTESIAN_POINT('',(-7.16521648939811,0.,-10.));
#35618=CARTESIAN_POINT('',(-7.16521648939811,500.,-10.));
#35619=CARTESIAN_POINT('',(-7.16521648939811,0.,-13.));
#35620=CARTESIAN_POINT('',(-7.1652164893981,500.,-13.));
#35621=CARTESIAN_POINT('',(-7.16521648939811,0.,-10.));
#35622=CARTESIAN_POINT('Origin',(-12.8347835106019,0.,-10.));
#35623=CARTESIAN_POINT('',(-12.8347835106019,0.,-10.));
#35624=CARTESIAN_POINT('',(-7.16521648939811,0.,-10.));
#35625=CARTESIAN_POINT('',(-12.8347835106019,0.,-13.));
#35626=CARTESIAN_POINT('',(-7.1652164893981,0.,-13.));
#35627=CARTESIAN_POINT('',(-12.8347835106019,0.,-10.));
#35628=CARTESIAN_POINT('Origin',(-12.8347835106019,35.2970569134824,-10.));
#35629=CARTESIAN_POINT('',(-12.8347835106019,35.2970569134824,-10.));
#35630=CARTESIAN_POINT('',(-12.8347835106019,0.,-10.));
#35631=CARTESIAN_POINT('',(-12.8347835106019,35.2970569134824,-13.));
#35632=CARTESIAN_POINT('',(-12.8347835106019,0.,-13.));
#35633=CARTESIAN_POINT('',(-12.8347835106019,35.2970569134824,-10.));
#35634=CARTESIAN_POINT('Origin',(-33.8864916534318,35.2970569134824,-10.));
#35635=CARTESIAN_POINT('',(-33.8864916534318,35.2970569134824,-10.));
#35636=CARTESIAN_POINT('',(15.,35.2970569134824,-9.99999999999998));
#35637=CARTESIAN_POINT('',(-33.8864916534318,35.2970569134824,-13.));
#35638=CARTESIAN_POINT('',(15.,35.2970569134824,-13.));
#35639=CARTESIAN_POINT('',(-33.8864916534318,35.2970569134824,-10.));
#35640=CARTESIAN_POINT('Origin',(-33.8864916534318,30.2970569134824,-10.));
#35641=CARTESIAN_POINT('',(-38.8864916534318,30.2970569134824,-10.));
#35642=CARTESIAN_POINT('Origin',(-33.8864916534318,30.2970569134824,-10.));
#35643=CARTESIAN_POINT('',(-38.8864916534318,30.2970569134824,-13.));
#35644=CARTESIAN_POINT('Origin',(-33.8864916534318,30.2970569134824,-13.));
#35645=CARTESIAN_POINT('',(-38.8864916534318,30.2970569134824,-10.));
#35646=CARTESIAN_POINT('Origin',(-38.8864916534318,-56.2946587134524,-10.));
#35647=CARTESIAN_POINT('',(-38.8864916534318,-56.2946587134524,-10.));
#35648=CARTESIAN_POINT('',(-38.8864916534318,30.2970569134824,-10.));
#35649=CARTESIAN_POINT('',(-38.8864916534318,-56.2946587134524,-13.));
#35650=CARTESIAN_POINT('',(-38.8864916534318,30.2970569134824,-13.));
#35651=CARTESIAN_POINT('',(-38.8864916534318,-56.2946587134524,-10.));
#35652=CARTESIAN_POINT('Origin',(-33.8864916534318,-56.2946587134524,-10.));
#35653=CARTESIAN_POINT('',(-33.8864916534318,-61.2946587134525,-10.));
#35654=CARTESIAN_POINT('Origin',(-33.8864916534318,-56.2946587134524,-10.));
#35655=CARTESIAN_POINT('',(-33.8864916534318,-61.2946587134525,-13.));
#35656=CARTESIAN_POINT('Origin',(-33.8864916534318,-56.2946587134524,-13.));
#35657=CARTESIAN_POINT('',(-33.8864916534318,-61.2946587134525,-10.));
#35658=CARTESIAN_POINT('Origin',(15.,-61.2946587134524,-9.99999999999998));
#35659=CARTESIAN_POINT('',(15.,-61.2946587134524,-9.99999999999998));
#35660=CARTESIAN_POINT('',(-33.8864916534318,-61.2946587134525,-10.));
#35661=CARTESIAN_POINT('',(15.,-61.2946587134524,-13.));
#35662=CARTESIAN_POINT('',(-33.8864916534318,-61.2946587134525,-13.));
#35663=CARTESIAN_POINT('',(15.,-61.2946587134524,-9.99999999999998));
#35664=CARTESIAN_POINT('Origin',(15.,-56.2946587134524,-9.99999999999998));
#35665=CARTESIAN_POINT('',(20.,-56.2946587134525,-9.99999999999998));
#35666=CARTESIAN_POINT('Origin',(15.,-56.2946587134524,-9.99999999999998));
#35667=CARTESIAN_POINT('',(20.,-56.2946587134525,-13.));
#35668=CARTESIAN_POINT('Origin',(15.,-56.2946587134524,-13.));
#35669=CARTESIAN_POINT('',(20.,-56.2946587134525,-9.99999999999998));
#35670=CARTESIAN_POINT('Origin',(20.,30.2970569134825,-9.99999999999998));
#35671=CARTESIAN_POINT('',(20.,30.2970569134825,-9.99999999999998));
#35672=CARTESIAN_POINT('',(20.,-56.2946587134525,-9.99999999999998));
#35673=CARTESIAN_POINT('',(20.,30.2970569134825,-13.));
#35674=CARTESIAN_POINT('',(20.,-56.2946587134525,-13.));
#35675=CARTESIAN_POINT('',(20.,30.2970569134825,-9.99999999999998));
#35676=CARTESIAN_POINT('Origin',(15.,30.2970569134825,-9.99999999999998));
#35677=CARTESIAN_POINT('Origin',(15.,30.2970569134825,-9.99999999999998));
#35678=CARTESIAN_POINT('Origin',(15.,30.2970569134825,-13.));
#35679=CARTESIAN_POINT('Origin',(-9.44324582671591,-12.998800899985,-13.));
#35680=CARTESIAN_POINT('Origin',(-9.44324582671591,-12.998800899985,-10.));
#35681=CARTESIAN_POINT('',(0.,0.,0.));
#35682=CARTESIAN_POINT('Origin',(0.,-32.9435013582377,8.74200000000021));
#35683=CARTESIAN_POINT('',(-4.19052498068885,-34.4435013582377,8.74200000000021));
#35684=CARTESIAN_POINT('Ctrl Pts',(-4.19052498068884,-34.4435013582377,
8.74200000000021));
#35685=CARTESIAN_POINT('Ctrl Pts',(-4.19052498068884,-34.4435013582377,
8.9312241160178));
#35686=CARTESIAN_POINT('Ctrl Pts',(-4.1803170480147,-34.4055199393726,9.13248256201596));
#35687=CARTESIAN_POINT('Ctrl Pts',(-4.14393283331602,-34.2521973359119,
9.50179602754586));
#35688=CARTESIAN_POINT('Ctrl Pts',(-4.11833409225485,-34.1368970199764,
9.66992468182113));
#35689=CARTESIAN_POINT('Ctrl Pts',(-4.0706574299838,-33.871444598845,9.93537710295256));
#35690=CARTESIAN_POINT('Ctrl Pts',(-4.04541244329492,-33.7033082151408,
10.0506918889611));
#35691=CARTESIAN_POINT('Ctrl Pts',(-4.00984509853063,-33.3339673419624,
10.2040250565453));
#35692=CARTESIAN_POINT('Ctrl Pts',(-3.99999999999997,-33.1326990173526,
10.2420000000002));
#35693=CARTESIAN_POINT('Ctrl Pts',(-3.99999999999997,-32.7543036991228,
10.2420000000002));
#35694=CARTESIAN_POINT('Ctrl Pts',(-4.00984509853063,-32.553035374513,10.2040250565453));
#35695=CARTESIAN_POINT('Ctrl Pts',(-4.04541244329492,-32.1836945013346,
10.0506918889611));
#35696=CARTESIAN_POINT('Ctrl Pts',(-4.0706574299838,-32.0155581176304,9.93537710295256));
#35697=CARTESIAN_POINT('Ctrl Pts',(-4.11833409225485,-31.750105696499,9.66992468182113));
#35698=CARTESIAN_POINT('Ctrl Pts',(-4.14393283331602,-31.6348053805635,
9.50179602754586));
#35699=CARTESIAN_POINT('Ctrl Pts',(-4.1803170480147,-31.4814827771028,9.13248256201596));
#35700=CARTESIAN_POINT('Ctrl Pts',(-4.19052498068884,-31.4435013582377,
8.9312241160178));
#35701=CARTESIAN_POINT('Ctrl Pts',(-4.19052498068884,-31.4435013582377,
8.55277588398262));
#35702=CARTESIAN_POINT('Ctrl Pts',(-4.1803170480147,-31.4814827771028,8.35151743798446));
#35703=CARTESIAN_POINT('Ctrl Pts',(-4.14393283331602,-31.6348053805635,
7.98220397245457));
#35704=CARTESIAN_POINT('Ctrl Pts',(-4.11833409225485,-31.750105696499,7.8140753181793));
#35705=CARTESIAN_POINT('Ctrl Pts',(-4.0706574299838,-32.0155581176304,7.54862289704786));
#35706=CARTESIAN_POINT('Ctrl Pts',(-4.04541244329492,-32.1836945013346,
7.43330811103931));
#35707=CARTESIAN_POINT('Ctrl Pts',(-4.00984509853063,-32.553035374513,7.27997494345513));
#35708=CARTESIAN_POINT('Ctrl Pts',(-3.99999999999997,-32.7543036991228,
7.24200000000021));
#35709=CARTESIAN_POINT('Ctrl Pts',(-3.99999999999997,-33.1326990173526,
7.24200000000021));
#35710=CARTESIAN_POINT('Ctrl Pts',(-4.00984509853063,-33.3339673419624,
7.27997494345513));
#35711=CARTESIAN_POINT('Ctrl Pts',(-4.04541244329492,-33.7033082151408,
7.4333081110393));
#35712=CARTESIAN_POINT('Ctrl Pts',(-4.0706574299838,-33.871444598845,7.54862289704786));
#35713=CARTESIAN_POINT('Ctrl Pts',(-4.11833409225485,-34.1368970199764,
7.81407531817929));
#35714=CARTESIAN_POINT('Ctrl Pts',(-4.14393283331602,-34.2521973359119,
7.98220397245456));
#35715=CARTESIAN_POINT('Ctrl Pts',(-4.1803170480147,-34.4055199393726,8.35151743798446));
#35716=CARTESIAN_POINT('Ctrl Pts',(-4.19052498068884,-34.4435013582377,
8.55277588398262));
#35717=CARTESIAN_POINT('Ctrl Pts',(-4.19052498068884,-34.4435013582377,
8.74200000000021));
#35718=CARTESIAN_POINT('',(-7.20167460791274,-34.4435013582377,8.74200000000021));
#35719=CARTESIAN_POINT('',(0.,-34.4435013582377,8.74200000000021));
#35720=CARTESIAN_POINT('Ctrl Pts',(-7.20167460791274,-34.4435013582377,
8.74200000000021));
#35721=CARTESIAN_POINT('Ctrl Pts',(-7.20167460791274,-34.4435013582377,
8.55007054774266));
#35722=CARTESIAN_POINT('Ctrl Pts',(-7.17982819701525,-34.4045170660368,
8.34794581242564));
#35723=CARTESIAN_POINT('Ctrl Pts',(-7.10528338281718,-34.2506168512765,
7.97957260321972));
#35724=CARTESIAN_POINT('Ctrl Pts',(-7.05406308684607,-34.1358048644253,
7.81298316262817));
#35725=CARTESIAN_POINT('Ctrl Pts',(-6.96084522509015,-33.8727957338775,
7.54997403208039));
#35726=CARTESIAN_POINT('Ctrl Pts',(-6.91224663391283,-33.7061091122768,
7.43495623663964));
#35727=CARTESIAN_POINT('Ctrl Pts',(-6.84394343734937,-33.3373267297171,
7.2808923176838));
#35728=CARTESIAN_POINT('Ctrl Pts',(-6.82499999999995,-33.1350261734663,
7.24200000000021));
#35729=CARTESIAN_POINT('Ctrl Pts',(-6.82499999999995,-32.7519765430091,
7.24200000000021));
#35730=CARTESIAN_POINT('Ctrl Pts',(-6.84394343734937,-32.5496759867583,
7.28089231768381));
#35731=CARTESIAN_POINT('Ctrl Pts',(-6.91224663391283,-32.1808936041986,
7.43495623663964));
#35732=CARTESIAN_POINT('Ctrl Pts',(-6.96084522509015,-32.0142069825979,
7.54997403208039));
#35733=CARTESIAN_POINT('Ctrl Pts',(-7.05406308684607,-31.7511978520501,
7.81298316262817));
#35734=CARTESIAN_POINT('Ctrl Pts',(-7.10528338281718,-31.6363858651989,
7.97957260321973));
#35735=CARTESIAN_POINT('Ctrl Pts',(-7.17982819701525,-31.4824856504386,
8.34794581242565));
#35736=CARTESIAN_POINT('Ctrl Pts',(-7.20167460791274,-31.4435013582377,
8.55007054774266));
#35737=CARTESIAN_POINT('Ctrl Pts',(-7.20167460791274,-31.4435013582377,
8.93392945225776));
#35738=CARTESIAN_POINT('Ctrl Pts',(-7.17982819701525,-31.4824856504386,
9.13605418757478));
#35739=CARTESIAN_POINT('Ctrl Pts',(-7.10528338281718,-31.6363858651989,
9.5044273967807));
#35740=CARTESIAN_POINT('Ctrl Pts',(-7.05406308684607,-31.7511978520501,
9.67101683737225));
#35741=CARTESIAN_POINT('Ctrl Pts',(-6.96084522509015,-32.0142069825979,
9.93402596792003));
#35742=CARTESIAN_POINT('Ctrl Pts',(-6.91224663391283,-32.1808936041986,
10.0490437633608));
#35743=CARTESIAN_POINT('Ctrl Pts',(-6.84394343734937,-32.5496759867583,
10.2031076823166));
#35744=CARTESIAN_POINT('Ctrl Pts',(-6.82499999999995,-32.7519765430091,
10.2420000000002));
#35745=CARTESIAN_POINT('Ctrl Pts',(-6.82499999999995,-33.1350261734663,
10.2420000000002));
#35746=CARTESIAN_POINT('Ctrl Pts',(-6.84394343734937,-33.3373267297171,
10.2031076823166));
#35747=CARTESIAN_POINT('Ctrl Pts',(-6.91224663391283,-33.7061091122768,
10.0490437633608));
#35748=CARTESIAN_POINT('Ctrl Pts',(-6.96084522509015,-33.8727957338775,
9.93402596792003));
#35749=CARTESIAN_POINT('Ctrl Pts',(-7.05406308684607,-34.1358048644253,
9.67101683737225));
#35750=CARTESIAN_POINT('Ctrl Pts',(-7.10528338281718,-34.2506168512765,
9.50442739678069));
#35751=CARTESIAN_POINT('Ctrl Pts',(-7.17982819701525,-34.4045170660368,
9.13605418757477));
#35752=CARTESIAN_POINT('Ctrl Pts',(-7.20167460791274,-34.4435013582377,
8.93392945225776));
#35753=CARTESIAN_POINT('Ctrl Pts',(-7.20167460791274,-34.4435013582377,
8.74200000000021));
#35754=CARTESIAN_POINT('Origin',(0.,-32.9435013582377,8.74200000000021));
#35755=CARTESIAN_POINT('',(-13.175,-32.9435013582377,7.24200000000021));
#35756=CARTESIAN_POINT('',(-12.7983253920872,-34.4435013582377,8.74200000000021));
#35757=CARTESIAN_POINT('Ctrl Pts',(-13.175,-32.9435013582377,7.24200000000021));
#35758=CARTESIAN_POINT('Ctrl Pts',(-13.175,-33.1350261734663,7.24200000000021));
#35759=CARTESIAN_POINT('Ctrl Pts',(-13.1560565626506,-33.3373267297171,
7.2808923176838));
#35760=CARTESIAN_POINT('Ctrl Pts',(-13.0877533660871,-33.7061091122768,
7.43495623663964));
#35761=CARTESIAN_POINT('Ctrl Pts',(-13.0391547749098,-33.8727957338775,
7.54997403208039));
#35762=CARTESIAN_POINT('Ctrl Pts',(-12.9459369131539,-34.1358048644253,
7.81298316262817));
#35763=CARTESIAN_POINT('Ctrl Pts',(-12.8947166171828,-34.2506168512765,
7.97957260321972));
#35764=CARTESIAN_POINT('Ctrl Pts',(-12.8201718029847,-34.4045170660368,
8.34794581242564));
#35765=CARTESIAN_POINT('Ctrl Pts',(-12.7983253920872,-34.4435013582377,
8.55007054774266));
#35766=CARTESIAN_POINT('Ctrl Pts',(-12.7983253920872,-34.4435013582377,
8.74200000000021));
#35767=CARTESIAN_POINT('',(-13.175,-32.9435013582377,10.2420000000002));
#35768=CARTESIAN_POINT('Ctrl Pts',(-13.175,-32.9435013582377,10.2420000000002));
#35769=CARTESIAN_POINT('Ctrl Pts',(-13.175,-32.7519765430091,10.2420000000002));
#35770=CARTESIAN_POINT('Ctrl Pts',(-13.1560565626506,-32.5496759867583,
10.2031076823166));
#35771=CARTESIAN_POINT('Ctrl Pts',(-13.0877533660871,-32.1808936041986,
10.0490437633608));
#35772=CARTESIAN_POINT('Ctrl Pts',(-13.0391547749098,-32.0142069825979,
9.93402596792003));
#35773=CARTESIAN_POINT('Ctrl Pts',(-12.9459369131539,-31.7511978520501,
9.67101683737225));
#35774=CARTESIAN_POINT('Ctrl Pts',(-12.8947166171828,-31.6363858651989,
9.5044273967807));
#35775=CARTESIAN_POINT('Ctrl Pts',(-12.8201718029847,-31.4824856504386,
9.13605418757478));
#35776=CARTESIAN_POINT('Ctrl Pts',(-12.7983253920872,-31.4435013582377,
8.93392945225776));
#35777=CARTESIAN_POINT('Ctrl Pts',(-12.7983253920872,-31.4435013582377,
8.55007054774266));
#35778=CARTESIAN_POINT('Ctrl Pts',(-12.8201718029847,-31.4824856504386,
8.34794581242564));
#35779=CARTESIAN_POINT('Ctrl Pts',(-12.8947166171828,-31.6363858651989,
7.97957260321972));
#35780=CARTESIAN_POINT('Ctrl Pts',(-12.9459369131539,-31.7511978520501,
7.81298316262817));
#35781=CARTESIAN_POINT('Ctrl Pts',(-13.0391547749098,-32.0142069825979,
7.54997403208039));
#35782=CARTESIAN_POINT('Ctrl Pts',(-13.0877533660871,-32.1808936041986,
7.43495623663964));
#35783=CARTESIAN_POINT('Ctrl Pts',(-13.1560565626506,-32.5496759867583,
7.28089231768381));
#35784=CARTESIAN_POINT('Ctrl Pts',(-13.175,-32.7519765430091,7.24200000000021));
#35785=CARTESIAN_POINT('Ctrl Pts',(-13.175,-32.9435013582377,7.24200000000021));
#35786=CARTESIAN_POINT('Ctrl Pts',(-12.7983253920872,-34.4435013582377,
8.74200000000021));
#35787=CARTESIAN_POINT('Ctrl Pts',(-12.7983253920872,-34.4435013582377,
8.93392945225776));
#35788=CARTESIAN_POINT('Ctrl Pts',(-12.8201718029847,-34.4045170660368,
9.13605418757477));
#35789=CARTESIAN_POINT('Ctrl Pts',(-12.8947166171828,-34.2506168512765,
9.5044273967807));
#35790=CARTESIAN_POINT('Ctrl Pts',(-12.9459369131539,-34.1358048644253,
9.67101683737225));
#35791=CARTESIAN_POINT('Ctrl Pts',(-13.0391547749098,-33.8727957338775,
9.93402596792003));
#35792=CARTESIAN_POINT('Ctrl Pts',(-13.0877533660871,-33.7061091122768,
10.0490437633608));
#35793=CARTESIAN_POINT('Ctrl Pts',(-13.1560565626506,-33.3373267297171,
10.2031076823166));
#35794=CARTESIAN_POINT('Ctrl Pts',(-13.175,-33.1350261734663,10.2420000000002));
#35795=CARTESIAN_POINT('Ctrl Pts',(-13.175,-32.9435013582377,10.2420000000002));
#35796=CARTESIAN_POINT('',(-15.8094750193111,-34.4435013582377,8.74200000000021));
#35797=CARTESIAN_POINT('',(0.,-34.4435013582377,8.74200000000021));
#35798=CARTESIAN_POINT('',(-16.,-32.9435013582377,10.2420000000002));
#35799=CARTESIAN_POINT('Ctrl Pts',(-16.,-32.9435013582377,10.2420000000002));
#35800=CARTESIAN_POINT('Ctrl Pts',(-16.,-33.1326990173526,10.2420000000002));
#35801=CARTESIAN_POINT('Ctrl Pts',(-15.9901549014694,-33.3339673419624,
10.2040250565453));
#35802=CARTESIAN_POINT('Ctrl Pts',(-15.9545875567051,-33.7033082151408,
10.0506918889611));
#35803=CARTESIAN_POINT('Ctrl Pts',(-15.9293425700162,-33.871444598845,9.93537710295256));
#35804=CARTESIAN_POINT('Ctrl Pts',(-15.8816659077451,-34.1368970199764,
9.66992468182113));
#35805=CARTESIAN_POINT('Ctrl Pts',(-15.856067166684,-34.2521973359119,9.50179602754586));
#35806=CARTESIAN_POINT('Ctrl Pts',(-15.8196829519853,-34.4055199393726,
9.13248256201596));
#35807=CARTESIAN_POINT('Ctrl Pts',(-15.8094750193111,-34.4435013582377,
8.9312241160178));
#35808=CARTESIAN_POINT('Ctrl Pts',(-15.8094750193111,-34.4435013582377,
8.74200000000021));
#35809=CARTESIAN_POINT('',(-16.,-32.9435013582377,7.24200000000021));
#35810=CARTESIAN_POINT('Ctrl Pts',(-16.,-32.9435013582377,7.24200000000021));
#35811=CARTESIAN_POINT('Ctrl Pts',(-16.,-32.7543036991228,7.24200000000021));
#35812=CARTESIAN_POINT('Ctrl Pts',(-15.9901549014694,-32.553035374513,7.27997494345513));
#35813=CARTESIAN_POINT('Ctrl Pts',(-15.9545875567051,-32.1836945013346,
7.43330811103931));
#35814=CARTESIAN_POINT('Ctrl Pts',(-15.9293425700162,-32.0155581176304,
7.54862289704786));
#35815=CARTESIAN_POINT('Ctrl Pts',(-15.8816659077451,-31.750105696499,7.8140753181793));
#35816=CARTESIAN_POINT('Ctrl Pts',(-15.856067166684,-31.6348053805635,7.98220397245456));
#35817=CARTESIAN_POINT('Ctrl Pts',(-15.8196829519853,-31.4814827771028,
8.35151743798446));
#35818=CARTESIAN_POINT('Ctrl Pts',(-15.8094750193111,-31.4435013582377,
8.55277588398262));
#35819=CARTESIAN_POINT('Ctrl Pts',(-15.8094750193111,-31.4435013582377,
8.9312241160178));
#35820=CARTESIAN_POINT('Ctrl Pts',(-15.8196829519853,-31.4814827771028,
9.13248256201596));
#35821=CARTESIAN_POINT('Ctrl Pts',(-15.856067166684,-31.6348053805635,9.50179602754586));
#35822=CARTESIAN_POINT('Ctrl Pts',(-15.8816659077451,-31.750105696499,9.66992468182113));
#35823=CARTESIAN_POINT('Ctrl Pts',(-15.9293425700162,-32.0155581176304,
9.93537710295256));
#35824=CARTESIAN_POINT('Ctrl Pts',(-15.9545875567051,-32.1836945013346,
10.0506918889611));
#35825=CARTESIAN_POINT('Ctrl Pts',(-15.9901549014694,-32.553035374513,10.2040250565453));
#35826=CARTESIAN_POINT('Ctrl Pts',(-16.,-32.7543036991228,10.2420000000002));
#35827=CARTESIAN_POINT('Ctrl Pts',(-16.,-32.9435013582377,10.2420000000002));
#35828=CARTESIAN_POINT('Ctrl Pts',(-15.8094750193111,-34.4435013582377,
8.74200000000021));
#35829=CARTESIAN_POINT('Ctrl Pts',(-15.8094750193111,-34.4435013582377,
8.55277588398262));
#35830=CARTESIAN_POINT('Ctrl Pts',(-15.8196829519853,-34.4055199393726,
8.35151743798446));
#35831=CARTESIAN_POINT('Ctrl Pts',(-15.856067166684,-34.2521973359119,7.98220397245456));
#35832=CARTESIAN_POINT('Ctrl Pts',(-15.8816659077451,-34.1368970199764,
7.81407531817929));
#35833=CARTESIAN_POINT('Ctrl Pts',(-15.9293425700162,-33.871444598845,7.54862289704786));
#35834=CARTESIAN_POINT('Ctrl Pts',(-15.9545875567051,-33.7033082151408,
7.4333081110393));
#35835=CARTESIAN_POINT('Ctrl Pts',(-15.9901549014694,-33.3339673419624,
7.27997494345513));
#35836=CARTESIAN_POINT('Ctrl Pts',(-16.,-33.1326990173526,7.24200000000021));
#35837=CARTESIAN_POINT('Ctrl Pts',(-16.,-32.9435013582377,7.24200000000021));
#35838=CARTESIAN_POINT('Origin',(-9.99999999999999,-32.9435013582377,-3.50799999999979));
#35839=CARTESIAN_POINT('',(-16.,-32.9435013582377,10.9920000000002));
#35840=CARTESIAN_POINT('Origin',(-9.99999999999999,-32.9435013582377,10.9920000000002));
#35841=CARTESIAN_POINT('',(-16.,-32.9435013582377,-3.50799999999979));
#35842=CARTESIAN_POINT('',(-16.,-32.9435013582377,4.99200000000021));
#35843=CARTESIAN_POINT('',(-16.,-32.9435013582377,-3.50799999999979));
#35844=CARTESIAN_POINT('Origin',(-9.99999999999999,-32.9435013582377,4.99200000000021));
#35845=CARTESIAN_POINT('Origin',(-10.,-32.9435013582377,10.9920000000002));
#35846=CARTESIAN_POINT('',(-13.175,-32.9435013582377,10.9920000000002));
#35847=CARTESIAN_POINT('Origin',(-9.99999999999998,-32.9435013582377,10.9920000000002));
#35848=CARTESIAN_POINT('Origin',(-10.,-32.9435013582377,3.49200000000021));
#35849=CARTESIAN_POINT('',(-20.75,-32.9435013582377,3.49200000000021));
#35850=CARTESIAN_POINT('Origin',(-10.,-32.9435013582377,3.49200000000021));
#35851=CARTESIAN_POINT('',(-19.15,-32.9435013582377,3.49200000000021));
#35852=CARTESIAN_POINT('Origin',(-9.99999999999996,-32.9435013582377,3.49200000000021));
#35853=CARTESIAN_POINT('Origin',(-10.,-32.9435013582377,3.49200000000021));
#35854=CARTESIAN_POINT('',(-20.75,-32.9435013582377,4.99200000000021));
#35855=CARTESIAN_POINT('Origin',(-10.,-32.9435013582377,4.99200000000021));
#35856=CARTESIAN_POINT('',(-20.75,-32.9435013582377,3.49200000000021));
#35857=CARTESIAN_POINT('Origin',(-10.,-32.9435013582377,4.99200000000021));
#35858=CARTESIAN_POINT('Origin',(-9.99999999999996,-32.9435013582377,-3.50799999999979));
#35859=CARTESIAN_POINT('',(-19.15,-32.9435013582377,-2.00799999999979));
#35860=CARTESIAN_POINT('',(-19.15,-32.9435013582377,-3.50799999999979));
#35861=CARTESIAN_POINT('Origin',(-9.99999999999996,-32.9435013582377,-2.00799999999979));
#35862=CARTESIAN_POINT('Origin',(-9.99999999999998,-32.9435013582377,-3.50799999999979));
#35863=CARTESIAN_POINT('',(-13.175,-32.9435013582377,-3.50799999999979));
#35864=CARTESIAN_POINT('Origin',(-9.99999999999998,-32.9435013582377,-3.50799999999979));
#35865=CARTESIAN_POINT('',(-13.175,-32.9435013582377,-3.50799999999979));
#35866=CARTESIAN_POINT('',(-13.175,-32.9435013582377,-3.50799999999979));
#35867=CARTESIAN_POINT('Origin',(-10.,-32.9435013582377,-3.50799999999979));
#35868=CARTESIAN_POINT('',(-20.75,-32.9435013582377,-2.00799999999979));
#35869=CARTESIAN_POINT('Origin',(-10.,-32.9435013582377,-2.00799999999979));
#35870=CARTESIAN_POINT('',(-20.75,-32.9435013582377,-3.50799999999979));
#35871=CARTESIAN_POINT('',(-20.75,-32.9435013582377,-3.50799999999979));
#35872=CARTESIAN_POINT('Origin',(-10.,-32.9435013582377,-3.50799999999979));
#35873=CARTESIAN_POINT('Origin',(-10.,-32.9435013582377,-2.00799999999979));
#35874=CARTESIAN_POINT('Origin',(-10.,-32.9435013582377,-3.50799999999979));
#35875=CARTESIAN_POINT('',(0.,0.,0.));
#35876=CARTESIAN_POINT('Origin',(-9.99999999999996,243.556498641762,-1.25799999999979));
#35877=CARTESIAN_POINT('',(1.50000000000004,-32.9435013582377,-1.25799999999979));
#35878=CARTESIAN_POINT('',(-21.5,-32.9435013582377,-1.25799999999979));
#35879=CARTESIAN_POINT('Origin',(-9.99999999999996,-32.9435013582377,-1.25799999999979));
#35880=CARTESIAN_POINT('',(-21.5,520.056498641762,-1.25799999999979));
#35881=CARTESIAN_POINT('',(-21.5,520.056498641762,-1.25799999999979));
#35882=CARTESIAN_POINT('',(1.50000000000004,520.056498641762,-1.25799999999979));
#35883=CARTESIAN_POINT('Origin',(-9.99999999999996,520.056498641762,-1.25799999999979));
#35884=CARTESIAN_POINT('',(1.50000000000004,-32.9435013582377,-1.25799999999979));
#35885=CARTESIAN_POINT('',(-19.5,-32.9435013582377,-1.25799999999979));
#35886=CARTESIAN_POINT('',(-0.499999999999963,-32.9435013582377,-1.25799999999979));
#35887=CARTESIAN_POINT('Origin',(-9.99999999999996,-32.9435013582377,-1.25799999999979));
#35888=CARTESIAN_POINT('',(-0.499999999999963,520.056498641762,-1.25799999999979));
#35889=CARTESIAN_POINT('',(-0.499999999999963,-32.9435013582377,-1.25799999999979));
#35890=CARTESIAN_POINT('',(-19.5,520.056498641762,-1.25799999999979));
#35891=CARTESIAN_POINT('Origin',(-9.99999999999996,520.056498641762,-1.25799999999979));
#35892=CARTESIAN_POINT('',(-19.5,520.056498641762,-1.25799999999979));
#35893=CARTESIAN_POINT('Origin',(-0.499999999999963,520.056498641762,0.742000000000206));
#35894=CARTESIAN_POINT('',(-0.499999999999963,-32.9435013582377,2.74200000000021));
#35895=CARTESIAN_POINT('',(-0.499999999999963,-32.9435013582377,0.742000000000206));
#35896=CARTESIAN_POINT('',(-0.499999999999963,520.056498641762,2.74200000000021));
#35897=CARTESIAN_POINT('',(-0.499999999999963,-32.9435013582377,2.74200000000021));
#35898=CARTESIAN_POINT('',(-0.499999999999963,520.056498641762,0.742000000000206));
#35899=CARTESIAN_POINT('Origin',(-9.99999999999996,520.056498641762,0.742000000000206));
#35900=CARTESIAN_POINT('',(-19.5,520.056498641762,2.74200000000021));
#35901=CARTESIAN_POINT('Origin',(-9.99999999999996,520.056498641762,2.74200000000021));
#35902=CARTESIAN_POINT('',(-19.5,520.056498641762,0.742000000000206));
#35903=CARTESIAN_POINT('Origin',(-19.5,-32.9435013582377,0.742000000000206));
#35904=CARTESIAN_POINT('',(-19.5,-32.9435013582377,2.74200000000021));
#35905=CARTESIAN_POINT('',(-19.5,520.056498641762,2.74200000000021));
#35906=CARTESIAN_POINT('',(-19.5,-32.9435013582377,0.742000000000206));
#35907=CARTESIAN_POINT('Origin',(-9.99999999999996,-32.9435013582377,0.742000000000206));
#35908=CARTESIAN_POINT('Origin',(-9.99999999999996,-32.9435013582377,2.74200000000021));
#35909=CARTESIAN_POINT('Origin',(-21.5,520.056498641762,0.742000000000206));
#35910=CARTESIAN_POINT('',(-21.5,-32.9435013582377,2.74200000000021));
#35911=CARTESIAN_POINT('',(-21.5,-32.9435013582377,0.742000000000206));
#35912=CARTESIAN_POINT('',(-21.5,520.056498641762,2.74200000000021));
#35913=CARTESIAN_POINT('',(-21.5,520.056498641762,2.74200000000021));
#35914=CARTESIAN_POINT('',(-21.5,520.056498641762,0.742000000000206));
#35915=CARTESIAN_POINT('Origin',(-9.99999999999996,520.056498641762,0.742000000000206));
#35916=CARTESIAN_POINT('',(1.50000000000004,520.056498641762,2.74200000000021));
#35917=CARTESIAN_POINT('Origin',(-9.99999999999996,520.056498641762,2.74200000000021));
#35918=CARTESIAN_POINT('',(1.50000000000004,520.056498641762,0.742000000000206));
#35919=CARTESIAN_POINT('Origin',(1.50000000000004,-32.9435013582377,0.742000000000206));
#35920=CARTESIAN_POINT('',(1.50000000000004,-32.9435013582377,2.74200000000021));
#35921=CARTESIAN_POINT('',(1.50000000000004,-32.9435013582377,2.74200000000021));
#35922=CARTESIAN_POINT('',(1.50000000000004,-32.9435013582377,0.742000000000206));
#35923=CARTESIAN_POINT('Origin',(-9.99999999999996,-32.9435013582377,0.742000000000206));
#35924=CARTESIAN_POINT('Origin',(-9.99999999999996,-32.9435013582377,2.74200000000021));
#35925=CARTESIAN_POINT('Origin',(-9.99999999999996,243.556498641762,2.74200000000021));
#35926=CARTESIAN_POINT('',(0.,0.,0.));
#35927=CARTESIAN_POINT('Origin',(-22.5,232.431902763327,-19.1700672509895));
#35928=CARTESIAN_POINT('',(-22.5,234.931902763327,-19.1700672509895));
#35929=CARTESIAN_POINT('Origin',(-22.5,232.431902763327,-19.1700672509895));
#35930=CARTESIAN_POINT('',(-24.5,234.931902763327,-19.1700672509894));
#35931=CARTESIAN_POINT('',(-22.5,234.931902763327,-19.1700672509895));
#35932=CARTESIAN_POINT('Origin',(-24.5,232.431902763327,-19.1700672509895));
#35933=CARTESIAN_POINT('Origin',(-22.5,182.525945920127,23.982775519786));
#35934=CARTESIAN_POINT('',(-22.5,182.525945920127,23.982775519786));
#35935=CARTESIAN_POINT('',(-22.5,182.525945920127,17.2567109421317));
#35936=CARTESIAN_POINT('',(-22.5,182.525945920127,17.2567109421317));
#35937=CARTESIAN_POINT('',(-24.5,182.525945920127,17.2567109421317));
#35938=CARTESIAN_POINT('',(-22.5,182.525945920127,17.2567109421317));
#35939=CARTESIAN_POINT('',(-24.5,182.525945920127,23.982775519786));
#35940=CARTESIAN_POINT('',(-24.5,182.525945920127,17.2567109421317));
#35941=CARTESIAN_POINT('',(-22.5,182.525945920127,23.982775519786));
#35942=CARTESIAN_POINT('Origin',(-22.5,183.91845147722,23.982775519786));
#35943=CARTESIAN_POINT('',(-22.5,185.310957034312,23.982775519786));
#35944=CARTESIAN_POINT('Origin',(-22.5,183.91845147722,23.982775519786));
#35945=CARTESIAN_POINT('',(-24.5,185.310957034312,23.982775519786));
#35946=CARTESIAN_POINT('Origin',(-24.5,183.91845147722,23.982775519786));
#35947=CARTESIAN_POINT('',(-22.5,185.310957034312,23.982775519786));
#35948=CARTESIAN_POINT('Origin',(-22.5,185.310957034312,17.2567109421317));
#35949=CARTESIAN_POINT('',(-22.5,185.310957034312,17.2567109421317));
#35950=CARTESIAN_POINT('',(-22.5,185.310957034312,23.982775519786));
#35951=CARTESIAN_POINT('',(-24.5,185.310957034312,17.2567109421317));
#35952=CARTESIAN_POINT('',(-24.5,185.310957034312,23.982775519786));
#35953=CARTESIAN_POINT('',(-22.5,185.310957034312,17.2567109421317));
#35954=CARTESIAN_POINT('Origin',(-22.5,183.91845147722,17.2567109421317));
#35955=CARTESIAN_POINT('Origin',(-22.5,183.91845147722,17.2567109421317));
#35956=CARTESIAN_POINT('Origin',(-24.5,183.91845147722,17.2567109421317));
#35957=CARTESIAN_POINT('Origin',(-22.5,211.657861025925,0.886420913981472));
#35958=CARTESIAN_POINT('',(-22.5,214.124612099013,0.886420913981471));
#35959=CARTESIAN_POINT('Origin',(-22.5,211.657861025925,0.886420913981472));
#35960=CARTESIAN_POINT('',(-24.5,214.124612099013,0.886420913981472));
#35961=CARTESIAN_POINT('',(-22.5,214.124612099013,0.886420913981472));
#35962=CARTESIAN_POINT('Origin',(-24.5,211.657861025925,0.886420913981472));
#35963=CARTESIAN_POINT('Origin',(-22.5,221.602473620571,-19.1135790860185));
#35964=CARTESIAN_POINT('',(-22.5,224.069224693659,-19.1135790860185));
#35965=CARTESIAN_POINT('Origin',(-22.5,221.602473620571,-19.1135790860185));
#35966=CARTESIAN_POINT('',(-24.5,224.069224693659,-19.1135790860185));
#35967=CARTESIAN_POINT('',(-22.5,224.069224693659,-19.1135790860185));
#35968=CARTESIAN_POINT('Origin',(-24.5,221.602473620571,-19.1135790860185));
#35969=CARTESIAN_POINT('Origin',(-22.5,211.657861025925,-19.1135790860185));
#35970=CARTESIAN_POINT('',(-22.5,214.124612099013,-19.1135790860185));
#35971=CARTESIAN_POINT('Origin',(-22.5,211.657861025925,-19.1135790860185));
#35972=CARTESIAN_POINT('',(-24.5,214.124612099013,-19.1135790860185));
#35973=CARTESIAN_POINT('',(-22.5,214.124612099013,-19.1135790860185));
#35974=CARTESIAN_POINT('Origin',(-24.5,211.657861025925,-19.1135790860185));
#35975=CARTESIAN_POINT('Origin',(-22.5,211.657861025925,20.8864209139815));
#35976=CARTESIAN_POINT('',(-22.5,214.124612099013,20.8864209139815));
#35977=CARTESIAN_POINT('Origin',(-22.5,211.657861025925,20.8864209139815));
#35978=CARTESIAN_POINT('',(-24.5,214.124612099013,20.8864209139815));
#35979=CARTESIAN_POINT('',(-22.5,214.124612099013,20.8864209139815));
#35980=CARTESIAN_POINT('Origin',(-24.5,211.657861025925,20.8864209139815));
#35981=CARTESIAN_POINT('Origin',(-22.5,201.657861025925,20.8864209139815));
#35982=CARTESIAN_POINT('',(-22.5,204.124612099013,20.8864209139815));
#35983=CARTESIAN_POINT('Origin',(-22.5,201.657861025925,20.8864209139815));
#35984=CARTESIAN_POINT('',(-24.5,204.124612099013,20.8864209139815));
#35985=CARTESIAN_POINT('',(-22.5,204.124612099013,20.8864209139815));
#35986=CARTESIAN_POINT('Origin',(-24.5,201.657861025925,20.8864209139815));
#35987=CARTESIAN_POINT('Origin',(-22.5,189.00788651778,10.7107295366928));
#35988=CARTESIAN_POINT('',(-22.5,189.00788651778,10.7107295366928));
#35989=CARTESIAN_POINT('',(-22.5,189.00788651778,-9.36247421041762));
#35990=CARTESIAN_POINT('',(-22.5,189.00788651778,-9.36247421041762));
#35991=CARTESIAN_POINT('',(-24.5,189.00788651778,-9.36247421041762));
#35992=CARTESIAN_POINT('',(-22.5,189.00788651778,-9.36247421041762));
#35993=CARTESIAN_POINT('',(-24.5,189.00788651778,10.7107295366928));
#35994=CARTESIAN_POINT('',(-24.5,189.00788651778,-9.36247421041762));
#35995=CARTESIAN_POINT('',(-22.5,189.00788651778,10.7107295366928));
#35996=CARTESIAN_POINT('Origin',(-22.5,191.707791115344,10.7107295366928));
#35997=CARTESIAN_POINT('',(-22.5,194.407695712909,10.7107295366928));
#35998=CARTESIAN_POINT('Origin',(-22.5,191.707791115344,10.7107295366928));
#35999=CARTESIAN_POINT('',(-24.5,194.407695712909,10.7107295366928));
#36000=CARTESIAN_POINT('Origin',(-24.5,191.707791115344,10.7107295366928));
#36001=CARTESIAN_POINT('',(-22.5,194.407695712909,10.7107295366928));
#36002=CARTESIAN_POINT('Origin',(-22.5,194.407695712909,-9.36247421041762));
#36003=CARTESIAN_POINT('',(-22.5,194.407695712909,-9.36247421041762));
#36004=CARTESIAN_POINT('',(-22.5,194.407695712909,10.7107295366928));
#36005=CARTESIAN_POINT('',(-24.5,194.407695712909,-9.36247421041762));
#36006=CARTESIAN_POINT('',(-24.5,194.407695712909,10.7107295366928));
#36007=CARTESIAN_POINT('',(-22.5,194.407695712909,-9.36247421041762));
#36008=CARTESIAN_POINT('Origin',(-22.5,191.707791115344,-9.36247421041762));
#36009=CARTESIAN_POINT('Origin',(-22.5,191.707791115344,-9.36247421041762));
#36010=CARTESIAN_POINT('Origin',(-24.5,191.707791115344,-9.36247421041762));
#36011=CARTESIAN_POINT('Origin',(-22.5,237.949377612184,-16.017224480214));
#36012=CARTESIAN_POINT('',(-22.5,237.949377612184,-16.017224480214));
#36013=CARTESIAN_POINT('',(-22.5,237.949377612184,-22.7432890578683));
#36014=CARTESIAN_POINT('',(-22.5,237.949377612184,-16.017224480214));
#36015=CARTESIAN_POINT('',(-24.5,237.949377612184,-22.7432890578683));
#36016=CARTESIAN_POINT('',(-22.5,237.949377612184,-22.7432890578683));
#36017=CARTESIAN_POINT('',(-24.5,237.949377612184,-16.017224480214));
#36018=CARTESIAN_POINT('',(-24.5,237.949377612184,-16.017224480214));
#36019=CARTESIAN_POINT('',(-22.5,237.949377612184,-16.017224480214));
#36020=CARTESIAN_POINT('Origin',(-22.5,239.341883169277,-16.017224480214));
#36021=CARTESIAN_POINT('',(-22.5,240.734388726369,-16.017224480214));
#36022=CARTESIAN_POINT('Origin',(-22.5,239.341883169277,-16.017224480214));
#36023=CARTESIAN_POINT('',(-24.5,240.734388726369,-16.017224480214));
#36024=CARTESIAN_POINT('Origin',(-24.5,239.341883169277,-16.017224480214));
#36025=CARTESIAN_POINT('',(-22.5,240.734388726369,-16.017224480214));
#36026=CARTESIAN_POINT('Origin',(-22.5,240.734388726369,-22.7432890578683));
#36027=CARTESIAN_POINT('',(-22.5,240.734388726369,-22.7432890578683));
#36028=CARTESIAN_POINT('',(-22.5,240.734388726369,-22.7432890578683));
#36029=CARTESIAN_POINT('',(-24.5,240.734388726369,-22.7432890578683));
#36030=CARTESIAN_POINT('',(-24.5,240.734388726369,-22.7432890578683));
#36031=CARTESIAN_POINT('',(-22.5,240.734388726369,-22.7432890578683));
#36032=CARTESIAN_POINT('Origin',(-22.5,239.341883169277,-22.7432890578683));
#36033=CARTESIAN_POINT('Origin',(-22.5,239.341883169277,-22.7432890578683));
#36034=CARTESIAN_POINT('Origin',(-24.5,239.341883169277,-22.7432890578683));
#36035=CARTESIAN_POINT('Origin',(-22.5,190.828431883169,-19.1700672509895));
#36036=CARTESIAN_POINT('',(-22.5,193.328431883169,-19.1700672509895));
#36037=CARTESIAN_POINT('Origin',(-22.5,190.828431883169,-19.1700672509895));
#36038=CARTESIAN_POINT('',(-24.5,193.328431883169,-19.1700672509894));
#36039=CARTESIAN_POINT('',(-22.5,193.328431883169,-19.1700672509895));
#36040=CARTESIAN_POINT('Origin',(-24.5,190.828431883169,-19.1700672509895));
#36041=CARTESIAN_POINT('Origin',(-22.5,221.602473620571,0.886420913981474));
#36042=CARTESIAN_POINT('',(-22.5,224.069224693659,0.886420913981474));
#36043=CARTESIAN_POINT('Origin',(-22.5,221.602473620571,0.886420913981474));
#36044=CARTESIAN_POINT('',(-24.5,224.069224693659,0.886420913981474));
#36045=CARTESIAN_POINT('',(-22.5,224.069224693659,0.886420913981474));
#36046=CARTESIAN_POINT('Origin',(-24.5,221.602473620571,0.886420913981474));
#36047=CARTESIAN_POINT('Origin',(-22.5,190.828431883169,20.8299327490105));
#36048=CARTESIAN_POINT('',(-22.5,193.328431883169,20.8299327490105));
#36049=CARTESIAN_POINT('Origin',(-22.5,190.828431883169,20.8299327490105));
#36050=CARTESIAN_POINT('',(-24.5,193.328431883169,20.8299327490105));
#36051=CARTESIAN_POINT('',(-22.5,193.328431883169,20.8299327490105));
#36052=CARTESIAN_POINT('Origin',(-24.5,190.828431883169,20.8299327490105));
#36053=CARTESIAN_POINT('Origin',(-22.5,201.657861025925,0.886420913981472));
#36054=CARTESIAN_POINT('',(-22.5,204.124612099013,0.886420913981471));
#36055=CARTESIAN_POINT('Origin',(-22.5,201.657861025925,0.886420913981472));
#36056=CARTESIAN_POINT('',(-24.5,204.124612099013,0.886420913981472));
#36057=CARTESIAN_POINT('',(-22.5,204.124612099013,0.886420913981472));
#36058=CARTESIAN_POINT('Origin',(-24.5,201.657861025925,0.886420913981472));
#36059=CARTESIAN_POINT('Origin',(-22.5,201.657861025925,-19.1135790860185));
#36060=CARTESIAN_POINT('',(-22.5,204.124612099013,-19.1135790860185));
#36061=CARTESIAN_POINT('Origin',(-22.5,201.657861025925,-19.1135790860185));
#36062=CARTESIAN_POINT('',(-24.5,204.124612099013,-19.1135790860185));
#36063=CARTESIAN_POINT('',(-22.5,204.124612099013,-19.1135790860185));
#36064=CARTESIAN_POINT('Origin',(-24.5,201.657861025925,-19.1135790860185));
#36065=CARTESIAN_POINT('Origin',(-22.5,185.310957034312,-2.74328905786827));
#36066=CARTESIAN_POINT('',(-22.5,185.310957034312,-2.74328905786827));
#36067=CARTESIAN_POINT('',(-22.5,185.310957034312,3.98277551978598));
#36068=CARTESIAN_POINT('',(-22.5,185.310957034312,3.98277551978598));
#36069=CARTESIAN_POINT('',(-24.5,185.310957034312,3.98277551978598));
#36070=CARTESIAN_POINT('',(-22.5,185.310957034312,3.98277551978598));
#36071=CARTESIAN_POINT('',(-24.5,185.310957034312,-2.74328905786827));
#36072=CARTESIAN_POINT('',(-24.5,185.310957034312,3.98277551978598));
#36073=CARTESIAN_POINT('',(-22.5,185.310957034312,-2.74328905786827));
#36074=CARTESIAN_POINT('Origin',(-22.5,183.91845147722,-2.74328905786827));
#36075=CARTESIAN_POINT('',(-22.5,182.525945920127,-2.74328905786827));
#36076=CARTESIAN_POINT('Origin',(-22.5,183.91845147722,-2.74328905786827));
#36077=CARTESIAN_POINT('',(-24.5,182.525945920127,-2.74328905786827));
#36078=CARTESIAN_POINT('Origin',(-24.5,183.91845147722,-2.74328905786827));
#36079=CARTESIAN_POINT('',(-22.5,182.525945920127,-2.74328905786827));
#36080=CARTESIAN_POINT('Origin',(-22.5,182.525945920127,3.98277551978598));
#36081=CARTESIAN_POINT('',(-22.5,182.525945920127,3.98277551978598));
#36082=CARTESIAN_POINT('',(-22.5,182.525945920127,-2.74328905786827));
#36083=CARTESIAN_POINT('',(-24.5,182.525945920127,3.98277551978598));
#36084=CARTESIAN_POINT('',(-24.5,182.525945920127,-2.74328905786827));
#36085=CARTESIAN_POINT('',(-22.5,182.525945920127,3.98277551978598));
#36086=CARTESIAN_POINT('Origin',(-22.5,183.91845147722,3.98277551978598));
#36087=CARTESIAN_POINT('Origin',(-22.5,183.91845147722,3.98277551978598));
#36088=CARTESIAN_POINT('Origin',(-24.5,183.91845147722,3.98277551978598));
#36089=CARTESIAN_POINT('Origin',(-22.5,232.431902763327,20.8299327490105));
#36090=CARTESIAN_POINT('',(-22.5,234.931902763327,20.8299327490105));
#36091=CARTESIAN_POINT('Origin',(-22.5,232.431902763327,20.8299327490105));
#36092=CARTESIAN_POINT('',(-24.5,234.931902763327,20.8299327490105));
#36093=CARTESIAN_POINT('',(-22.5,234.931902763327,20.8299327490105));
#36094=CARTESIAN_POINT('Origin',(-24.5,232.431902763327,20.8299327490105));
#36095=CARTESIAN_POINT('Origin',(-22.5,221.602473620571,20.8864209139815));
#36096=CARTESIAN_POINT('',(-22.5,224.069224693659,20.8864209139815));
#36097=CARTESIAN_POINT('Origin',(-22.5,221.602473620571,20.8864209139815));
#36098=CARTESIAN_POINT('',(-24.5,224.069224693659,20.8864209139815));
#36099=CARTESIAN_POINT('',(-22.5,224.069224693659,20.8864209139815));
#36100=CARTESIAN_POINT('Origin',(-24.5,221.602473620571,20.8864209139815));
#36101=CARTESIAN_POINT('Origin',(-22.5,237.949377612184,3.98277551978598));
#36102=CARTESIAN_POINT('',(-22.5,237.949377612184,3.98277551978598));
#36103=CARTESIAN_POINT('',(-22.5,237.949377612184,-2.74328905786827));
#36104=CARTESIAN_POINT('',(-22.5,237.949377612184,3.98277551978598));
#36105=CARTESIAN_POINT('',(-24.5,237.949377612184,-2.74328905786827));
#36106=CARTESIAN_POINT('',(-22.5,237.949377612184,-2.74328905786827));
#36107=CARTESIAN_POINT('',(-24.5,237.949377612184,3.98277551978598));
#36108=CARTESIAN_POINT('',(-24.5,237.949377612184,3.98277551978598));
#36109=CARTESIAN_POINT('',(-22.5,237.949377612184,3.98277551978598));
#36110=CARTESIAN_POINT('Origin',(-22.5,239.341883169277,3.98277551978598));
#36111=CARTESIAN_POINT('',(-22.5,240.734388726369,3.98277551978598));
#36112=CARTESIAN_POINT('Origin',(-22.5,239.341883169277,3.98277551978598));
#36113=CARTESIAN_POINT('',(-24.5,240.734388726369,3.98277551978598));
#36114=CARTESIAN_POINT('Origin',(-24.5,239.341883169277,3.98277551978598));
#36115=CARTESIAN_POINT('',(-22.5,240.734388726369,3.98277551978598));
#36116=CARTESIAN_POINT('Origin',(-22.5,240.734388726369,-2.74328905786827));
#36117=CARTESIAN_POINT('',(-22.5,240.734388726369,-2.74328905786827));
#36118=CARTESIAN_POINT('',(-22.5,240.734388726369,-2.74328905786827));
#36119=CARTESIAN_POINT('',(-24.5,240.734388726369,-2.74328905786827));
#36120=CARTESIAN_POINT('',(-24.5,240.734388726369,-2.74328905786827));
#36121=CARTESIAN_POINT('',(-22.5,240.734388726369,-2.74328905786827));
#36122=CARTESIAN_POINT('Origin',(-22.5,239.341883169277,-2.74328905786827));
#36123=CARTESIAN_POINT('Origin',(-22.5,239.341883169277,-2.74328905786827));
#36124=CARTESIAN_POINT('Origin',(-24.5,239.341883169277,-2.74328905786827));
#36125=CARTESIAN_POINT('Origin',(-22.5,185.310957034312,-22.7432890578683));
#36126=CARTESIAN_POINT('',(-22.5,185.310957034312,-22.7432890578683));
#36127=CARTESIAN_POINT('',(-22.5,185.310957034312,-16.017224480214));
#36128=CARTESIAN_POINT('',(-22.5,185.310957034312,-16.017224480214));
#36129=CARTESIAN_POINT('',(-24.5,185.310957034312,-16.017224480214));
#36130=CARTESIAN_POINT('',(-22.5,185.310957034312,-16.017224480214));
#36131=CARTESIAN_POINT('',(-24.5,185.310957034312,-22.7432890578683));
#36132=CARTESIAN_POINT('',(-24.5,185.310957034312,-16.017224480214));
#36133=CARTESIAN_POINT('',(-22.5,185.310957034312,-22.7432890578683));
#36134=CARTESIAN_POINT('Origin',(-22.5,183.91845147722,-22.7432890578683));
#36135=CARTESIAN_POINT('',(-22.5,182.525945920127,-22.7432890578683));
#36136=CARTESIAN_POINT('Origin',(-22.5,183.91845147722,-22.7432890578683));
#36137=CARTESIAN_POINT('',(-24.5,182.525945920127,-22.7432890578683));
#36138=CARTESIAN_POINT('Origin',(-24.5,183.91845147722,-22.7432890578683));
#36139=CARTESIAN_POINT('',(-22.5,182.525945920127,-22.7432890578683));
#36140=CARTESIAN_POINT('Origin',(-22.5,182.525945920127,-16.017224480214));
#36141=CARTESIAN_POINT('',(-22.5,182.525945920127,-16.017224480214));
#36142=CARTESIAN_POINT('',(-22.5,182.525945920127,-22.7432890578683));
#36143=CARTESIAN_POINT('',(-24.5,182.525945920127,-16.017224480214));
#36144=CARTESIAN_POINT('',(-24.5,182.525945920127,-22.7432890578683));
#36145=CARTESIAN_POINT('',(-22.5,182.525945920127,-16.017224480214));
#36146=CARTESIAN_POINT('Origin',(-22.5,183.91845147722,-16.017224480214));
#36147=CARTESIAN_POINT('Origin',(-22.5,183.91845147722,-16.017224480214));
#36148=CARTESIAN_POINT('Origin',(-24.5,183.91845147722,-16.017224480214));
#36149=CARTESIAN_POINT('Origin',(-22.5,237.949377612184,23.982775519786));
#36150=CARTESIAN_POINT('',(-22.5,237.949377612184,23.982775519786));
#36151=CARTESIAN_POINT('',(-22.5,237.949377612184,17.2567109421317));
#36152=CARTESIAN_POINT('',(-22.5,237.949377612184,23.982775519786));
#36153=CARTESIAN_POINT('',(-24.5,237.949377612184,17.2567109421317));
#36154=CARTESIAN_POINT('',(-22.5,237.949377612184,17.2567109421317));
#36155=CARTESIAN_POINT('',(-24.5,237.949377612184,23.982775519786));
#36156=CARTESIAN_POINT('',(-24.5,237.949377612184,23.982775519786));
#36157=CARTESIAN_POINT('',(-22.5,237.949377612184,23.982775519786));
#36158=CARTESIAN_POINT('Origin',(-22.5,239.341883169277,23.982775519786));
#36159=CARTESIAN_POINT('',(-22.5,240.734388726369,23.982775519786));
#36160=CARTESIAN_POINT('Origin',(-22.5,239.341883169277,23.982775519786));
#36161=CARTESIAN_POINT('',(-24.5,240.734388726369,23.982775519786));
#36162=CARTESIAN_POINT('Origin',(-24.5,239.341883169277,23.982775519786));
#36163=CARTESIAN_POINT('',(-22.5,240.734388726369,23.982775519786));
#36164=CARTESIAN_POINT('Origin',(-22.5,240.734388726369,17.2567109421317));
#36165=CARTESIAN_POINT('',(-22.5,240.734388726369,17.2567109421317));
#36166=CARTESIAN_POINT('',(-22.5,240.734388726369,17.2567109421317));
#36167=CARTESIAN_POINT('',(-24.5,240.734388726369,17.2567109421317));
#36168=CARTESIAN_POINT('',(-24.5,240.734388726369,17.2567109421317));
#36169=CARTESIAN_POINT('',(-22.5,240.734388726369,17.2567109421317));
#36170=CARTESIAN_POINT('Origin',(-22.5,239.341883169277,17.2567109421317));
#36171=CARTESIAN_POINT('Origin',(-22.5,239.341883169277,17.2567109421317));
#36172=CARTESIAN_POINT('Origin',(-24.5,239.341883169277,17.2567109421317));
#36173=CARTESIAN_POINT('Origin',(-22.5,228.852638933588,10.7107295366928));
#36174=CARTESIAN_POINT('',(-22.5,228.852638933588,10.7107295366928));
#36175=CARTESIAN_POINT('',(-22.5,228.852638933588,-9.36247421041762));
#36176=CARTESIAN_POINT('',(-22.5,228.852638933588,10.7107295366928));
#36177=CARTESIAN_POINT('',(-24.5,228.852638933588,-9.36247421041762));
#36178=CARTESIAN_POINT('',(-22.5,228.852638933588,-9.36247421041762));
#36179=CARTESIAN_POINT('',(-24.5,228.852638933588,10.7107295366928));
#36180=CARTESIAN_POINT('',(-24.5,228.852638933588,10.7107295366928));
#36181=CARTESIAN_POINT('',(-22.5,228.852638933588,10.7107295366928));
#36182=CARTESIAN_POINT('Origin',(-22.5,231.552543531152,10.7107295366928));
#36183=CARTESIAN_POINT('',(-22.5,234.252448128717,10.7107295366928));
#36184=CARTESIAN_POINT('Origin',(-22.5,231.552543531152,10.7107295366928));
#36185=CARTESIAN_POINT('',(-24.5,234.252448128717,10.7107295366928));
#36186=CARTESIAN_POINT('Origin',(-24.5,231.552543531152,10.7107295366928));
#36187=CARTESIAN_POINT('',(-22.5,234.252448128717,10.7107295366928));
#36188=CARTESIAN_POINT('Origin',(-22.5,234.252448128717,-9.36247421041762));
#36189=CARTESIAN_POINT('',(-22.5,234.252448128717,-9.36247421041762));
#36190=CARTESIAN_POINT('',(-22.5,234.252448128717,-9.36247421041762));
#36191=CARTESIAN_POINT('',(-24.5,234.252448128717,-9.36247421041762));
#36192=CARTESIAN_POINT('',(-24.5,234.252448128717,-9.36247421041762));
#36193=CARTESIAN_POINT('',(-22.5,234.252448128717,-9.36247421041762));
#36194=CARTESIAN_POINT('Origin',(-22.5,231.552543531152,-9.36247421041762));
#36195=CARTESIAN_POINT('Origin',(-22.5,231.552543531152,-9.36247421041762));
#36196=CARTESIAN_POINT('Origin',(-24.5,231.552543531152,-9.36247421041762));
#36197=CARTESIAN_POINT('Origin',(-22.5,211.657861025925,-9.11357908601853));
#36198=CARTESIAN_POINT('',(-22.5,214.124612099013,-9.11357908601853));
#36199=CARTESIAN_POINT('Origin',(-22.5,211.657861025925,-9.11357908601853));
#36200=CARTESIAN_POINT('',(-24.5,214.124612099013,-9.11357908601853));
#36201=CARTESIAN_POINT('',(-22.5,214.124612099013,-9.11357908601853));
#36202=CARTESIAN_POINT('Origin',(-24.5,211.657861025925,-9.11357908601853));
#36203=CARTESIAN_POINT('Origin',(-22.5,211.657861025925,10.8864209139815));
#36204=CARTESIAN_POINT('',(-22.5,214.124612099013,10.8864209139815));
#36205=CARTESIAN_POINT('Origin',(-22.5,211.657861025925,10.8864209139815));
#36206=CARTESIAN_POINT('',(-24.5,214.124612099013,10.8864209139815));
#36207=CARTESIAN_POINT('',(-22.5,214.124612099013,10.8864209139815));
#36208=CARTESIAN_POINT('Origin',(-24.5,211.657861025925,10.8864209139815));
#36209=CARTESIAN_POINT('Origin',(-22.5,241.399687575155,-32.0121872517985));
#36210=CARTESIAN_POINT('',(-22.5,181.860647071341,-32.0121872517985));
#36211=CARTESIAN_POINT('',(-22.5,241.399687575155,-32.0121872517985));
#36212=CARTESIAN_POINT('',(-22.5,181.860647071341,-32.0121872517985));
#36213=CARTESIAN_POINT('',(-24.5,181.860647071341,-32.0121872517985));
#36214=CARTESIAN_POINT('',(-22.5,181.860647071341,-32.0121872517985));
#36215=CARTESIAN_POINT('',(-24.5,241.399687575155,-32.0121872517985));
#36216=CARTESIAN_POINT('',(-24.5,181.860647071341,-32.0121872517985));
#36217=CARTESIAN_POINT('',(-22.5,241.399687575155,-32.0121872517985));
#36218=CARTESIAN_POINT('Origin',(-22.5,241.399687575155,-29.0121872517985));
#36219=CARTESIAN_POINT('',(-22.5,244.399687575155,-29.0121872517985));
#36220=CARTESIAN_POINT('Origin',(-22.5,241.399687575155,-29.0121872517985));
#36221=CARTESIAN_POINT('',(-24.5,244.399687575155,-29.0121872517985));
#36222=CARTESIAN_POINT('Origin',(-24.5,241.399687575155,-29.0121872517985));
#36223=CARTESIAN_POINT('',(-22.5,244.399687575155,-29.0121872517985));
#36224=CARTESIAN_POINT('Origin',(-22.5,244.399687575155,30.5413729944905));
#36225=CARTESIAN_POINT('',(-22.5,244.399687575155,30.5413729944905));
#36226=CARTESIAN_POINT('',(-22.5,244.399687575155,-29.0121872517985));
#36227=CARTESIAN_POINT('',(-24.5,244.399687575155,30.5413729944905));
#36228=CARTESIAN_POINT('',(-24.5,244.399687575155,-29.0121872517985));
#36229=CARTESIAN_POINT('',(-22.5,244.399687575155,30.5413729944905));
#36230=CARTESIAN_POINT('Origin',(-22.5,241.399687575155,30.5413729944905));
#36231=CARTESIAN_POINT('',(-22.5,241.399687575155,33.5413729944905));
#36232=CARTESIAN_POINT('Origin',(-22.5,241.399687575155,30.5413729944905));
#36233=CARTESIAN_POINT('',(-24.5,241.399687575155,33.5413729944905));
#36234=CARTESIAN_POINT('Origin',(-24.5,241.399687575155,30.5413729944905));
#36235=CARTESIAN_POINT('',(-22.5,241.399687575155,33.5413729944905));
#36236=CARTESIAN_POINT('Origin',(-22.5,181.860647071341,33.5413729944905));
#36237=CARTESIAN_POINT('',(-22.5,181.860647071341,33.5413729944905));
#36238=CARTESIAN_POINT('',(-22.5,241.399687575155,33.5413729944905));
#36239=CARTESIAN_POINT('',(-24.5,181.860647071341,33.5413729944905));
#36240=CARTESIAN_POINT('',(-24.5,241.399687575155,33.5413729944905));
#36241=CARTESIAN_POINT('',(-22.5,181.860647071341,33.5413729944905));
#36242=CARTESIAN_POINT('Origin',(-22.5,181.860647071341,30.5413729944905));
#36243=CARTESIAN_POINT('',(-22.5,178.860647071341,30.5413729944905));
#36244=CARTESIAN_POINT('Origin',(-22.5,181.860647071341,30.5413729944905));
#36245=CARTESIAN_POINT('',(-24.5,178.860647071341,30.5413729944905));
#36246=CARTESIAN_POINT('Origin',(-24.5,181.860647071341,30.5413729944905));
#36247=CARTESIAN_POINT('',(-22.5,178.860647071341,30.5413729944905));
#36248=CARTESIAN_POINT('Origin',(-22.5,178.860647071341,-29.0121872517985));
#36249=CARTESIAN_POINT('',(-22.5,178.860647071341,-29.0121872517985));
#36250=CARTESIAN_POINT('',(-22.5,178.860647071341,30.5413729944905));
#36251=CARTESIAN_POINT('',(-24.5,178.860647071341,-29.0121872517985));
#36252=CARTESIAN_POINT('',(-24.5,178.860647071341,30.5413729944905));
#36253=CARTESIAN_POINT('',(-22.5,178.860647071341,-29.0121872517985));
#36254=CARTESIAN_POINT('Origin',(-22.5,181.860647071341,-29.0121872517985));
#36255=CARTESIAN_POINT('Origin',(-22.5,181.860647071341,-29.0121872517985));
#36256=CARTESIAN_POINT('Origin',(-24.5,181.860647071341,-29.0121872517985));
#36257=CARTESIAN_POINT('Origin',(-24.5,211.630167323248,0.764592871346017));
#36258=CARTESIAN_POINT('Origin',(-22.5,211.630167323248,0.764592871346017));
#36259=CARTESIAN_POINT('',(0.,0.,0.));
#36260=CARTESIAN_POINT('Origin',(10.,493.005151372827,-9.99999999999999));
#36261=CARTESIAN_POINT('',(7.49999999999999,493.005151372827,-9.99999999999999));
#36262=CARTESIAN_POINT('Origin',(10.,493.005151372827,-9.99999999999999));
#36263=CARTESIAN_POINT('',(7.49999999999999,493.005151372827,-13.));
#36264=CARTESIAN_POINT('',(7.49999999999999,493.005151372827,-9.99999999999999));
#36265=CARTESIAN_POINT('Origin',(10.,493.005151372827,-13.));
#36266=CARTESIAN_POINT('Origin',(-10.,473.005151372827,-9.99999999999999));
#36267=CARTESIAN_POINT('',(-12.5,473.005151372827,-9.99999999999999));
#36268=CARTESIAN_POINT('Origin',(-10.,473.005151372827,-9.99999999999999));
#36269=CARTESIAN_POINT('',(-12.5,473.005151372827,-13.));
#36270=CARTESIAN_POINT('',(-12.5,473.005151372827,-9.99999999999999));
#36271=CARTESIAN_POINT('Origin',(-10.,473.005151372827,-13.));
#36272=CARTESIAN_POINT('Origin',(-9.99999999999998,520.056498641762,-9.99999999999999));
#36273=CARTESIAN_POINT('',(-13.175,520.056498641762,-9.99999999999999));
#36274=CARTESIAN_POINT('Origin',(-9.99999999999998,520.056498641762,-9.99999999999999));
#36275=CARTESIAN_POINT('',(-13.175,520.056498641762,-13.));
#36276=CARTESIAN_POINT('',(-13.175,520.056498641762,-9.99999999999999));
#36277=CARTESIAN_POINT('Origin',(-9.99999999999998,520.056498641762,-13.));
#36278=CARTESIAN_POINT('Origin',(-10.,493.005151372827,-9.99999999999999));
#36279=CARTESIAN_POINT('',(-12.5,493.005151372827,-9.99999999999999));
#36280=CARTESIAN_POINT('Origin',(-10.,493.005151372827,-9.99999999999999));
#36281=CARTESIAN_POINT('',(-12.5,493.005151372827,-13.));
#36282=CARTESIAN_POINT('',(-12.5,493.005151372827,-9.99999999999999));
#36283=CARTESIAN_POINT('Origin',(-10.,493.005151372827,-13.));
#36284=CARTESIAN_POINT('Origin',(10.,473.005151372827,-9.99999999999999));
#36285=CARTESIAN_POINT('',(7.49999999999999,473.005151372827,-9.99999999999999));
#36286=CARTESIAN_POINT('Origin',(10.,473.005151372827,-9.99999999999999));
#36287=CARTESIAN_POINT('',(7.49999999999999,473.005151372827,-13.));
#36288=CARTESIAN_POINT('',(7.49999999999999,473.005151372827,-9.99999999999999));
#36289=CARTESIAN_POINT('Origin',(10.,473.005151372827,-13.));
#36290=CARTESIAN_POINT('Origin',(-15.,463.536269734217,-9.99999999999999));
#36291=CARTESIAN_POINT('',(-20.,463.536269734217,-9.99999999999999));
#36292=CARTESIAN_POINT('',(-15.,458.536269734217,-9.99999999999999));
#36293=CARTESIAN_POINT('Origin',(-15.,463.536269734217,-9.99999999999999));
#36294=CARTESIAN_POINT('',(-20.,463.536269734217,-13.));
#36295=CARTESIAN_POINT('',(-20.,463.536269734217,-9.99999999999999));
#36296=CARTESIAN_POINT('',(-15.,458.536269734217,-13.));
#36297=CARTESIAN_POINT('Origin',(-15.,463.536269734217,-13.));
#36298=CARTESIAN_POINT('',(-15.,458.536269734217,-9.99999999999999));
#36299=CARTESIAN_POINT('Origin',(15.,458.536269734217,-9.99999999999999));
#36300=CARTESIAN_POINT('',(15.,458.536269734217,-9.99999999999999));
#36301=CARTESIAN_POINT('',(15.,458.536269734217,-9.99999999999999));
#36302=CARTESIAN_POINT('',(15.,458.536269734217,-13.));
#36303=CARTESIAN_POINT('',(15.,458.536269734217,-13.));
#36304=CARTESIAN_POINT('',(15.,458.536269734217,-9.99999999999999));
#36305=CARTESIAN_POINT('Origin',(15.,463.536269734217,-9.99999999999999));
#36306=CARTESIAN_POINT('',(19.9999999999999,463.536269734217,-9.99999999999999));
#36307=CARTESIAN_POINT('Origin',(15.,463.536269734217,-9.99999999999999));
#36308=CARTESIAN_POINT('',(19.9999999999999,463.536269734217,-13.));
#36309=CARTESIAN_POINT('Origin',(15.,463.536269734217,-13.));
#36310=CARTESIAN_POINT('',(19.9999999999999,463.536269734217,-9.99999999999999));
#36311=CARTESIAN_POINT('Origin',(20.,532.759985569887,-9.99999999999999));
#36312=CARTESIAN_POINT('',(20.,532.759985569887,-9.99999999999999));
#36313=CARTESIAN_POINT('',(20.,532.759985569887,-9.99999999999999));
#36314=CARTESIAN_POINT('',(20.,532.759985569887,-13.));
#36315=CARTESIAN_POINT('',(20.,532.759985569887,-13.));
#36316=CARTESIAN_POINT('',(20.,532.759985569887,-9.99999999999999));
#36317=CARTESIAN_POINT('Origin',(15.,532.759985569887,-9.99999999999999));
#36318=CARTESIAN_POINT('',(15.,537.759985569887,-9.99999999999999));
#36319=CARTESIAN_POINT('Origin',(15.,532.759985569887,-9.99999999999999));
#36320=CARTESIAN_POINT('',(15.,537.759985569887,-13.));
#36321=CARTESIAN_POINT('Origin',(15.,532.759985569887,-13.));
#36322=CARTESIAN_POINT('',(15.,537.759985569887,-9.99999999999999));
#36323=CARTESIAN_POINT('Origin',(-15.,537.759985569887,-9.99999999999999));
#36324=CARTESIAN_POINT('',(-15.,537.759985569887,-9.99999999999999));
#36325=CARTESIAN_POINT('',(-15.,537.759985569887,-9.99999999999999));
#36326=CARTESIAN_POINT('',(-15.,537.759985569887,-13.));
#36327=CARTESIAN_POINT('',(-15.,537.759985569887,-13.));
#36328=CARTESIAN_POINT('',(-15.,537.759985569887,-9.99999999999999));
#36329=CARTESIAN_POINT('Origin',(-15.,532.759985569887,-9.99999999999999));
#36330=CARTESIAN_POINT('',(-20.,532.759985569887,-9.99999999999999));
#36331=CARTESIAN_POINT('Origin',(-15.,532.759985569887,-9.99999999999999));
#36332=CARTESIAN_POINT('',(-20.,532.759985569887,-13.));
#36333=CARTESIAN_POINT('Origin',(-15.,532.759985569887,-13.));
#36334=CARTESIAN_POINT('',(-20.,532.759985569887,-9.99999999999999));
#36335=CARTESIAN_POINT('Origin',(-20.,463.536269734217,-9.99999999999999));
#36336=CARTESIAN_POINT('',(-20.,463.536269734217,-9.99999999999999));
#36337=CARTESIAN_POINT('',(-20.,463.536269734217,-13.));
#36338=CARTESIAN_POINT('Origin',(-7.58590136239051E-15,498.148127652052,
-9.99999999999999));
#36339=CARTESIAN_POINT('Origin',(-7.58590136239051E-15,498.148127652052,
-13.));
#36340=CARTESIAN_POINT('',(0.,0.,0.));
#36341=CARTESIAN_POINT('Origin',(-8.06355459534025E-15,0.,-29.75462));
#36342=CARTESIAN_POINT('',(2.45049999999999,3.00099698131059E-16,-29.599539985206));
#36343=CARTESIAN_POINT('Origin',(-8.02085592265385E-15,0.,-29.599539985206));
#36344=CARTESIAN_POINT('',(2.00924,-2.46060933471884E-16,-30.));
#36345=CARTESIAN_POINT('',(2.27961999999997,2.79172933627226E-16,-29.75462));
#36346=CARTESIAN_POINT('Origin',(-8.13111584955928E-15,0.,-30.));
#36347=CARTESIAN_POINT('Origin',(7.38127335647334E-17,0.,-0.200000000000542));
#36348=CARTESIAN_POINT('',(2.4505,3.00099698131059E-16,-0.200000000000543));
#36349=CARTESIAN_POINT('Origin',(7.38127335647334E-17,0.,-0.200000000000542));
#36350=CARTESIAN_POINT('',(2.6505,-3.24592634114006E-16,-5.43004329167852E-13));
#36351=CARTESIAN_POINT('Origin',(2.6505,-3.24592634114006E-16,-0.200000000000543));
#36352=CARTESIAN_POINT('Origin',(1.28879368350801E-16,0.,-5.4227455859035E-13));
#36353=CARTESIAN_POINT('Origin',(-2.5,0.,-5.41596033937917E-13));
#36354=CARTESIAN_POINT('',(-4.75,0.,-1.02889918807136E-12));
#36355=CARTESIAN_POINT('Origin',(1.28879368350667E-16,0.,-1.03020702064753E-12));
#36356=CARTESIAN_POINT('Origin',(-4.00111824060424E-15,0.,-15.0000000000003));
#36357=CARTESIAN_POINT('',(2.4505,-3.00099698131059E-16,-15.0000000000003));
#36358=CARTESIAN_POINT('Origin',(2.77555756156289E-16,-1.73205080756888,
1.19));
#36359=CARTESIAN_POINT('',(2.77555756156289E-16,-1.73205080756888,1.19));
#36360=CARTESIAN_POINT('',(4.16333634234434E-16,-1.11022302462516E-15,1.05876700471111));
#36361=CARTESIAN_POINT('',(4.16333634234434E-16,-1.3015097128034,1.15737901843634));
#36362=CARTESIAN_POINT('',(1.5,-0.866025403784439,1.19));
#36363=CARTESIAN_POINT('',(2.67440770322657E-16,-1.73205080756888,1.19));
#36364=CARTESIAN_POINT('',(1.12714047455993,-0.650754856401699,1.15737901843634));
#36365=CARTESIAN_POINT('Origin',(1.5,-0.866025403784439,1.19));
#36366=CARTESIAN_POINT('',(1.5,0.866025403784438,1.19));
#36367=CARTESIAN_POINT('',(1.5,-0.866025403784439,1.19));
#36368=CARTESIAN_POINT('',(1.12714047455993,0.650754856401699,1.15737901843634));
#36369=CARTESIAN_POINT('Origin',(1.5,0.866025403784438,1.19));
#36370=CARTESIAN_POINT('',(0.,1.73205080756888,1.19));
#36371=CARTESIAN_POINT('',(1.5,0.866025403784438,1.19));
#36372=CARTESIAN_POINT('',(-2.77555756156289E-16,1.3015097128034,1.15737901843634));
#36373=CARTESIAN_POINT('Origin',(0.,1.73205080756888,1.19));
#36374=CARTESIAN_POINT('',(-1.5,0.866025403784439,1.19));
#36375=CARTESIAN_POINT('',(-6.93889390390723E-17,1.73205080756888,1.19));
#36376=CARTESIAN_POINT('',(-1.12714047455993,0.6507548564017,1.15737901843634));
#36377=CARTESIAN_POINT('Origin',(-1.5,0.866025403784439,1.19));
#36378=CARTESIAN_POINT('',(-1.5,-0.866025403784438,1.19));
#36379=CARTESIAN_POINT('',(-1.5,0.866025403784439,1.19));
#36380=CARTESIAN_POINT('',(-1.12714047455993,-0.650754856401698,1.15737901843634));
#36381=CARTESIAN_POINT('Origin',(-1.5,-0.866025403784438,1.19));
#36382=CARTESIAN_POINT('',(-1.5,-0.866025403784438,1.19));
#36383=CARTESIAN_POINT('Origin',(1.5,-0.866025403784439,2.75));
#36384=CARTESIAN_POINT('',(1.5,-0.866025403784439,2.75));
#36385=CARTESIAN_POINT('',(2.77555756156289E-16,-1.73205080756888,2.75));
#36386=CARTESIAN_POINT('',(0.393750000000001,-1.50471913907546,2.74999999999968));
#36387=CARTESIAN_POINT('',(1.5,-0.866025403784439,2.75));
#36388=CARTESIAN_POINT('',(2.77555756156289E-16,-1.73205080756888,2.75));
#36389=CARTESIAN_POINT('Origin',(1.5,0.866025403784438,2.75));
#36390=CARTESIAN_POINT('',(1.5,0.866025403784438,2.75));
#36391=CARTESIAN_POINT('',(1.5,0.433012701892219,2.74999999999967));
#36392=CARTESIAN_POINT('',(1.5,0.866025403784438,2.75));
#36393=CARTESIAN_POINT('Origin',(0.,1.73205080756888,2.75));
#36394=CARTESIAN_POINT('',(-6.93889390390723E-17,1.73205080756888,2.75));
#36395=CARTESIAN_POINT('',(-0.35625,1.93773184096768,2.74999999999968));
#36396=CARTESIAN_POINT('',(-6.93889390390723E-17,1.73205080756888,2.75));
#36397=CARTESIAN_POINT('Origin',(-1.5,0.866025403784439,2.75));
#36398=CARTESIAN_POINT('',(-1.5,0.866025403784439,2.75));
#36399=CARTESIAN_POINT('',(-1.85625,0.660344370385635,2.74999999999968));
#36400=CARTESIAN_POINT('',(-1.5,0.866025403784439,2.75));
#36401=CARTESIAN_POINT('Origin',(-1.5,-0.866025403784438,2.75));
#36402=CARTESIAN_POINT('',(-1.5,-0.866025403784438,2.75));
#36403=CARTESIAN_POINT('',(-1.5,-0.433012701892219,2.74999999999968));
#36404=CARTESIAN_POINT('',(-1.5,-0.866025403784438,2.75));
#36405=CARTESIAN_POINT('Origin',(2.77555756156289E-16,-1.73205080756888,
2.75));
#36406=CARTESIAN_POINT('',(-1.10625,-1.09335707227785,2.74999999999968));
#36407=CARTESIAN_POINT('Origin',(-8.04911692853238E-15,0.,-30.));
#36408=CARTESIAN_POINT('Origin',(-1.95,0.,2.74999999999968));
#36409=CARTESIAN_POINT('',(-1.95,0.,2.74999999999968));
#36410=CARTESIAN_POINT('Origin',(8.86045596659299E-16,0.,2.74999999999968));
#36411=CARTESIAN_POINT('Origin',(-5.55111512312578E-16,0.,-2.03590909090889));
#36412=CARTESIAN_POINT('Origin',(-5.55111512312578E-16,0.,-2.03590909090889));
#36413=CARTESIAN_POINT('',(-10.,-32.9435013582377,-23.0190000000001));
#36414=CARTESIAN_POINT('',(-24.5,232.431902763327,-19.1700672509895));
#36415=CARTESIAN_POINT('',(0.,0.,0.));
#36416=CARTESIAN_POINT('',(0.,41.6,-6.20571341877076E-15));
#36417=CARTESIAN_POINT('',(0.,0.,-40.));
#36418=CARTESIAN_POINT('',(0.,41.6,-40.));
#36419=CARTESIAN_POINT('',(0.,0.,0.));
#36420=CARTESIAN_POINT('',(0.,0.,0.));
#36421=CARTESIAN_POINT('',(0.,0.,0.));
#36422=CARTESIAN_POINT('',(0.,0.,0.));
#36423=CARTESIAN_POINT('',(0.,0.,0.));
#36424=CARTESIAN_POINT('',(0.,0.,0.));
#36425=CARTESIAN_POINT('',(0.,0.,0.));
#36426=CARTESIAN_POINT('',(-24.5,190.828431883169,-19.1700672509895));
#36427=CARTESIAN_POINT('',(-24.5,232.431902763327,20.8299327490105));
#36428=CARTESIAN_POINT('',(-24.5,190.828431883169,20.8299327490105));
#36429=UNCERTAINTY_MEASURE_WITH_UNIT(LENGTH_MEASURE(0.01),#36461,
'DISTANCE_ACCURACY_VALUE',
'Maximum model space distance between geometric entities at asserted c
onnectivities');
#36430=UNCERTAINTY_MEASURE_WITH_UNIT(LENGTH_MEASURE(0.01),#36461,
'DISTANCE_ACCURACY_VALUE',
'Maximum model space distance between geometric entities at asserted c
onnectivities');
#36431=UNCERTAINTY_MEASURE_WITH_UNIT(LENGTH_MEASURE(0.01),#36461,
'DISTANCE_ACCURACY_VALUE',
'Maximum model space distance between geometric entities at asserted c
onnectivities');
#36432=UNCERTAINTY_MEASURE_WITH_UNIT(LENGTH_MEASURE(0.01),#36461,
'DISTANCE_ACCURACY_VALUE',
'Maximum model space distance between geometric entities at asserted c
onnectivities');
#36433=UNCERTAINTY_MEASURE_WITH_UNIT(LENGTH_MEASURE(0.01),#36461,
'DISTANCE_ACCURACY_VALUE',
'Maximum model space distance between geometric entities at asserted c
onnectivities');
#36434=UNCERTAINTY_MEASURE_WITH_UNIT(LENGTH_MEASURE(0.01),#36461,
'DISTANCE_ACCURACY_VALUE',
'Maximum model space distance between geometric entities at asserted c
onnectivities');
#36435=UNCERTAINTY_MEASURE_WITH_UNIT(LENGTH_MEASURE(0.01),#36461,
'DISTANCE_ACCURACY_VALUE',
'Maximum model space distance between geometric entities at asserted c
onnectivities');
#36436=UNCERTAINTY_MEASURE_WITH_UNIT(LENGTH_MEASURE(0.01),#36461,
'DISTANCE_ACCURACY_VALUE',
'Maximum model space distance between geometric entities at asserted c
onnectivities');
#36437=UNCERTAINTY_MEASURE_WITH_UNIT(LENGTH_MEASURE(0.01),#36461,
'DISTANCE_ACCURACY_VALUE',
'Maximum model space distance between geometric entities at asserted c
onnectivities');
#36438=UNCERTAINTY_MEASURE_WITH_UNIT(LENGTH_MEASURE(0.01),#36461,
'DISTANCE_ACCURACY_VALUE',
'Maximum model space distance between geometric entities at asserted c
onnectivities');
#36439=UNCERTAINTY_MEASURE_WITH_UNIT(LENGTH_MEASURE(0.01),#36461,
'DISTANCE_ACCURACY_VALUE',
'Maximum model space distance between geometric entities at asserted c
onnectivities');
#36440=UNCERTAINTY_MEASURE_WITH_UNIT(LENGTH_MEASURE(0.01),#36461,
'DISTANCE_ACCURACY_VALUE',
'Maximum model space distance between geometric entities at asserted c
onnectivities');
#36441=UNCERTAINTY_MEASURE_WITH_UNIT(LENGTH_MEASURE(0.01),#36461,
'DISTANCE_ACCURACY_VALUE',
'Maximum model space distance between geometric entities at asserted c
onnectivities');
#36442=UNCERTAINTY_MEASURE_WITH_UNIT(LENGTH_MEASURE(0.01),#36461,
'DISTANCE_ACCURACY_VALUE',
'Maximum model space distance between geometric entities at asserted c
onnectivities');
#36443=UNCERTAINTY_MEASURE_WITH_UNIT(LENGTH_MEASURE(0.01),#36461,
'DISTANCE_ACCURACY_VALUE',
'Maximum model space distance between geometric entities at asserted c
onnectivities');
#36444=UNCERTAINTY_MEASURE_WITH_UNIT(LENGTH_MEASURE(0.01),#36461,
'DISTANCE_ACCURACY_VALUE',
'Maximum model space distance between geometric entities at asserted c
onnectivities');
#36445=(
GEOMETRIC_REPRESENTATION_CONTEXT(3)
GLOBAL_UNCERTAINTY_ASSIGNED_CONTEXT((#36429))
GLOBAL_UNIT_ASSIGNED_CONTEXT((#36461,#36463,#36464))
REPRESENTATION_CONTEXT('','3D')
);
#36446=(
GEOMETRIC_REPRESENTATION_CONTEXT(3)
GLOBAL_UNCERTAINTY_ASSIGNED_CONTEXT((#36430))
GLOBAL_UNIT_ASSIGNED_CONTEXT((#36461,#36463,#36464))
REPRESENTATION_CONTEXT('','3D')
);
#36447=(
GEOMETRIC_REPRESENTATION_CONTEXT(3)
GLOBAL_UNCERTAINTY_ASSIGNED_CONTEXT((#36431))
GLOBAL_UNIT_ASSIGNED_CONTEXT((#36461,#36463,#36464))
REPRESENTATION_CONTEXT('','3D')
);
#36448=(
GEOMETRIC_REPRESENTATION_CONTEXT(3)
GLOBAL_UNCERTAINTY_ASSIGNED_CONTEXT((#36432))
GLOBAL_UNIT_ASSIGNED_CONTEXT((#36461,#36463,#36464))
REPRESENTATION_CONTEXT('','3D')
);
#36449=(
GEOMETRIC_REPRESENTATION_CONTEXT(3)
GLOBAL_UNCERTAINTY_ASSIGNED_CONTEXT((#36433))
GLOBAL_UNIT_ASSIGNED_CONTEXT((#36461,#36463,#36464))
REPRESENTATION_CONTEXT('','3D')
);
#36450=(
GEOMETRIC_REPRESENTATION_CONTEXT(3)
GLOBAL_UNCERTAINTY_ASSIGNED_CONTEXT((#36434))
GLOBAL_UNIT_ASSIGNED_CONTEXT((#36461,#36463,#36464))
REPRESENTATION_CONTEXT('','3D')
);
#36451=(
GEOMETRIC_REPRESENTATION_CONTEXT(3)
GLOBAL_UNCERTAINTY_ASSIGNED_CONTEXT((#36435))
GLOBAL_UNIT_ASSIGNED_CONTEXT((#36461,#36463,#36464))
REPRESENTATION_CONTEXT('','3D')
);
#36452=(
GEOMETRIC_REPRESENTATION_CONTEXT(3)
GLOBAL_UNCERTAINTY_ASSIGNED_CONTEXT((#36436))
GLOBAL_UNIT_ASSIGNED_CONTEXT((#36461,#36463,#36464))
REPRESENTATION_CONTEXT('','3D')
);
#36453=(
GEOMETRIC_REPRESENTATION_CONTEXT(3)
GLOBAL_UNCERTAINTY_ASSIGNED_CONTEXT((#36437))
GLOBAL_UNIT_ASSIGNED_CONTEXT((#36461,#36463,#36464))
REPRESENTATION_CONTEXT('','3D')
);
#36454=(
GEOMETRIC_REPRESENTATION_CONTEXT(3)
GLOBAL_UNCERTAINTY_ASSIGNED_CONTEXT((#36438))
GLOBAL_UNIT_ASSIGNED_CONTEXT((#36461,#36463,#36464))
REPRESENTATION_CONTEXT('','3D')
);
#36455=(
GEOMETRIC_REPRESENTATION_CONTEXT(3)
GLOBAL_UNCERTAINTY_ASSIGNED_CONTEXT((#36439))
GLOBAL_UNIT_ASSIGNED_CONTEXT((#36461,#36463,#36464))
REPRESENTATION_CONTEXT('','3D')
);
#36456=(
GEOMETRIC_REPRESENTATION_CONTEXT(3)
GLOBAL_UNCERTAINTY_ASSIGNED_CONTEXT((#36440))
GLOBAL_UNIT_ASSIGNED_CONTEXT((#36461,#36463,#36464))
REPRESENTATION_CONTEXT('','3D')
);
#36457=(
GEOMETRIC_REPRESENTATION_CONTEXT(3)
GLOBAL_UNCERTAINTY_ASSIGNED_CONTEXT((#36441))
GLOBAL_UNIT_ASSIGNED_CONTEXT((#36461,#36463,#36464))
REPRESENTATION_CONTEXT('','3D')
);
#36458=(
GEOMETRIC_REPRESENTATION_CONTEXT(3)
GLOBAL_UNCERTAINTY_ASSIGNED_CONTEXT((#36442))
GLOBAL_UNIT_ASSIGNED_CONTEXT((#36461,#36463,#36464))
REPRESENTATION_CONTEXT('','3D')
);
#36459=(
GEOMETRIC_REPRESENTATION_CONTEXT(3)
GLOBAL_UNCERTAINTY_ASSIGNED_CONTEXT((#36443))
GLOBAL_UNIT_ASSIGNED_CONTEXT((#36461,#36463,#36464))
REPRESENTATION_CONTEXT('','3D')
);
#36460=(
GEOMETRIC_REPRESENTATION_CONTEXT(3)
GLOBAL_UNCERTAINTY_ASSIGNED_CONTEXT((#36444))
GLOBAL_UNIT_ASSIGNED_CONTEXT((#36461,#36463,#36464))
REPRESENTATION_CONTEXT('','3D')
);
#36461=(
LENGTH_UNIT()
NAMED_UNIT(*)
SI_UNIT(.MILLI.,.METRE.)
);
#36462=(
LENGTH_UNIT()
NAMED_UNIT(*)
SI_UNIT($,.METRE.)
);
#36463=(
NAMED_UNIT(*)
PLANE_ANGLE_UNIT()
SI_UNIT($,.RADIAN.)
);
#36464=(
NAMED_UNIT(*)
SI_UNIT($,.STERADIAN.)
SOLID_ANGLE_UNIT()
);
#36465=SHAPE_DEFINITION_REPRESENTATION(#36480,#36516);
#36466=SHAPE_DEFINITION_REPRESENTATION(#36481,#36517);
#36467=SHAPE_DEFINITION_REPRESENTATION(#36482,#36518);
#36468=SHAPE_DEFINITION_REPRESENTATION(#36483,#36519);
#36469=SHAPE_DEFINITION_REPRESENTATION(#36484,#36520);
#36470=SHAPE_DEFINITION_REPRESENTATION(#36485,#36521);
#36471=SHAPE_DEFINITION_REPRESENTATION(#36486,#36522);
#36472=SHAPE_DEFINITION_REPRESENTATION(#36492,#36523);
#36473=SHAPE_DEFINITION_REPRESENTATION(#36493,#36524);
#36474=SHAPE_DEFINITION_REPRESENTATION(#36494,#36525);
#36475=SHAPE_DEFINITION_REPRESENTATION(#36495,#36526);
#36476=SHAPE_DEFINITION_REPRESENTATION(#36496,#36527);
#36477=SHAPE_DEFINITION_REPRESENTATION(#36497,#36528);
#36478=SHAPE_DEFINITION_REPRESENTATION(#36498,#36529);
#36479=SHAPE_DEFINITION_REPRESENTATION(#36499,#36530);
#36480=PRODUCT_DEFINITION_SHAPE('',$,#36532);
#36481=PRODUCT_DEFINITION_SHAPE('',$,#36533);
#36482=PRODUCT_DEFINITION_SHAPE('',$,#36534);
#36483=PRODUCT_DEFINITION_SHAPE('',$,#36535);
#36484=PRODUCT_DEFINITION_SHAPE('',$,#36536);
#36485=PRODUCT_DEFINITION_SHAPE('',$,#36537);
#36486=PRODUCT_DEFINITION_SHAPE('',$,#36538);
#36487=PRODUCT_DEFINITION_SHAPE($,$,#74);
#36488=PRODUCT_DEFINITION_SHAPE($,$,#75);
#36489=PRODUCT_DEFINITION_SHAPE($,$,#76);
#36490=PRODUCT_DEFINITION_SHAPE($,$,#77);
#36491=PRODUCT_DEFINITION_SHAPE($,$,#78);
#36492=PRODUCT_DEFINITION_SHAPE('',$,#36539);
#36493=PRODUCT_DEFINITION_SHAPE('',$,#36540);
#36494=PRODUCT_DEFINITION_SHAPE('',$,#36541);
#36495=PRODUCT_DEFINITION_SHAPE('',$,#36542);
#36496=PRODUCT_DEFINITION_SHAPE('',$,#36543);
#36497=PRODUCT_DEFINITION_SHAPE('',$,#36544);
#36498=PRODUCT_DEFINITION_SHAPE('',$,#36545);
#36499=PRODUCT_DEFINITION_SHAPE('',$,#36546);
#36500=PRODUCT_DEFINITION_SHAPE($,$,#79);
#36501=PRODUCT_DEFINITION_SHAPE($,$,#80);
#36502=PRODUCT_DEFINITION_SHAPE($,$,#81);
#36503=PRODUCT_DEFINITION_SHAPE($,$,#82);
#36504=PRODUCT_DEFINITION_SHAPE($,$,#83);
#36505=PRODUCT_DEFINITION_SHAPE($,$,#84);
#36506=PRODUCT_DEFINITION_SHAPE($,$,#85);
#36507=PRODUCT_DEFINITION_SHAPE($,$,#86);
#36508=PRODUCT_DEFINITION_SHAPE($,$,#87);
#36509=PRODUCT_DEFINITION_SHAPE($,$,#88);
#36510=PRODUCT_DEFINITION_SHAPE($,$,#89);
#36511=PRODUCT_DEFINITION_SHAPE($,$,#90);
#36512=PRODUCT_DEFINITION_SHAPE($,$,#91);
#36513=PRODUCT_DEFINITION_SHAPE($,$,#92);
#36514=PRODUCT_DEFINITION_SHAPE($,$,#93);
#36515=PRODUCT_DEFINITION_SHAPE($,$,#94);
#36516=SHAPE_REPRESENTATION('',(#11438,#12421,#12422,#12423,#12424,#12425,
#12426,#12427,#12428,#12429,#12430,#12431,#12432,#12433,#12434,#12435,#12436),
#36445);
#36517=SHAPE_REPRESENTATION('',(#11439),#36446);
#36518=SHAPE_REPRESENTATION('',(#11887,#12004,#12005,#12006,#12007,#12008),
#36447);
#36519=SHAPE_REPRESENTATION('',(#11888),#36448);
#36520=SHAPE_REPRESENTATION('',(#11901),#36449);
#36521=SHAPE_REPRESENTATION('',(#11910),#36450);
#36522=SHAPE_REPRESENTATION('',(#11930),#36451);
#36523=SHAPE_REPRESENTATION('',(#12009),#36452);
#36524=SHAPE_REPRESENTATION('',(#12118),#36453);
#36525=SHAPE_REPRESENTATION('',(#12135),#36454);
#36526=SHAPE_REPRESENTATION('',(#12189),#36455);
#36527=SHAPE_REPRESENTATION('',(#12212),#36456);
#36528=SHAPE_REPRESENTATION('',(#12231),#36457);
#36529=SHAPE_REPRESENTATION('',(#12359),#36458);
#36530=SHAPE_REPRESENTATION('',(#12393),#36459);
#36531=PRODUCT_DEFINITION_CONTEXT('part definition',#36578,'design');
#36532=PRODUCT_DEFINITION('MAS-264','MAS-264',#36547,#36531);
#36533=PRODUCT_DEFINITION('Reference_design_envelope_Motor',
'Reference_design_envelope_Motor',#36548,#36531);
#36534=PRODUCT_DEFINITION('V_Wheel','V_Wheel',#36549,#36531);
#36535=PRODUCT_DEFINITION('Rubber','Rubber',#36550,#36531);
#36536=PRODUCT_DEFINITION('spacer','Spacer',#36551,#36531);
#36537=PRODUCT_DEFINITION('DIN 439-2 - M5 x 0.8 Steel 6 Plain',
'Hexagon Thin Nut DIN 439-2 - M5 x 0.8 Steel 6 Plain v1',#36552,#36531);
#36538=PRODUCT_DEFINITION(
'5908K51_Highly Corrosion-Resistant 316 Stainless Steel Ball Bearing',
'5908K51_Highly Corrosion-Resistant 316 Stainless Steel Ball Bearing',#36553,
#36531);
#36539=PRODUCT_DEFINITION('V-Slot 20x40','V-Slot 20x40',#36554,#36531);
#36540=PRODUCT_DEFINITION('pulley','Pulley',#36555,#36531);
#36541=PRODUCT_DEFINITION('Bracket_Motor','Bracket_Motor',#36556,#36531);
#36542=PRODUCT_DEFINITION('Pulley_Motor','Pulley_Motor',#36557,#36531);
#36543=PRODUCT_DEFINITION('GT2_Belt','GT2_Belt',#36558,#36531);
#36544=PRODUCT_DEFINITION('Bracket_Middle','Bracket_Middle',#36559,#36531);
#36545=PRODUCT_DEFINITION('Bracket','Bracket',#36560,#36531);
#36546=PRODUCT_DEFINITION(
'BHSBHCS ASME B18.3.4M - M5 x 0.8 x 30 Steel Grade 2 Plain',
'BHSBHCS ASME B18.3.4M - M5 x 0.8 x 30 Steel Grade 2 Plain',#36561,#36531);
#36547=PRODUCT_DEFINITION_FORMATION('',$,#36580);
#36548=PRODUCT_DEFINITION_FORMATION('',$,#36581);
#36549=PRODUCT_DEFINITION_FORMATION('',$,#36582);
#36550=PRODUCT_DEFINITION_FORMATION('',$,#36583);
#36551=PRODUCT_DEFINITION_FORMATION('',$,#36584);
#36552=PRODUCT_DEFINITION_FORMATION('',$,#36585);
#36553=PRODUCT_DEFINITION_FORMATION('',$,#36586);
#36554=PRODUCT_DEFINITION_FORMATION('',$,#36587);
#36555=PRODUCT_DEFINITION_FORMATION('',$,#36588);
#36556=PRODUCT_DEFINITION_FORMATION('',$,#36589);
#36557=PRODUCT_DEFINITION_FORMATION('',$,#36590);
#36558=PRODUCT_DEFINITION_FORMATION('',$,#36591);
#36559=PRODUCT_DEFINITION_FORMATION('',$,#36592);
#36560=PRODUCT_DEFINITION_FORMATION('',$,#36593);
#36561=PRODUCT_DEFINITION_FORMATION('',$,#36594);
#36562=PRODUCT_RELATED_PRODUCT_CATEGORY('MAS-264','MAS-264',(#36580));
#36563=PRODUCT_RELATED_PRODUCT_CATEGORY(
'Reference_design_envelope_Motor','Reference_design_envelope_Motor',(#36581));
#36564=PRODUCT_RELATED_PRODUCT_CATEGORY('V_Wheel','V_Wheel',(#36582));
#36565=PRODUCT_RELATED_PRODUCT_CATEGORY('Rubber','Rubber',(#36583));
#36566=PRODUCT_RELATED_PRODUCT_CATEGORY('Spacer','Spacer',(#36584));
#36567=PRODUCT_RELATED_PRODUCT_CATEGORY(
'Hexagon Thin Nut DIN 439-2 - M5 x 0.8 Steel 6 Plain v1',
'Hexagon Thin Nut DIN 439-2 - M5 x 0.8 Steel 6 Plain v1',(#36585));
#36568=PRODUCT_RELATED_PRODUCT_CATEGORY(
'5908K51_Highly Corrosion-Resistant 316 Stainless Steel Ball Bearing',
'5908K51_Highly Corrosion-Resistant 316 Stainless Steel Ball Bearing',(#36586));
#36569=PRODUCT_RELATED_PRODUCT_CATEGORY('V-Slot 20x40','V-Slot 20x40',(#36587));
#36570=PRODUCT_RELATED_PRODUCT_CATEGORY('Pulley','Pulley',(#36588));
#36571=PRODUCT_RELATED_PRODUCT_CATEGORY('Bracket_Motor','Bracket_Motor',
(#36589));
#36572=PRODUCT_RELATED_PRODUCT_CATEGORY('Pulley_Motor','Pulley_Motor',(#36590));
#36573=PRODUCT_RELATED_PRODUCT_CATEGORY('GT2_Belt','GT2_Belt',(#36591));
#36574=PRODUCT_RELATED_PRODUCT_CATEGORY('Bracket_Middle',
'Bracket_Middle',(#36592));
#36575=PRODUCT_RELATED_PRODUCT_CATEGORY('Bracket','Bracket',(#36593));
#36576=PRODUCT_RELATED_PRODUCT_CATEGORY(
'BHSBHCS ASME B18.3.4M - M5 x 0.8 x 30 Steel Grade 2 Plain',
'BHSBHCS ASME B18.3.4M - M5 x 0.8 x 30 Steel Grade 2 Plain',(#36594));
#36577=APPLICATION_PROTOCOL_DEFINITION('international standard',
'automotive_design',2009,#36578);
#36578=APPLICATION_CONTEXT(
'Core Data for Automotive Mechanical Design Process');
#36579=PRODUCT_CONTEXT('part definition',#36578,'mechanical');
#36580=PRODUCT('MAS-264','MAS-264',$,(#36579));
#36581=PRODUCT('Reference_design_envelope_Motor',
'Reference_design_envelope_Motor',$,(#36579));
#36582=PRODUCT('V_Wheel','V_Wheel',$,(#36579));
#36583=PRODUCT('Rubber','Rubber',$,(#36579));
#36584=PRODUCT('spacer','Spacer',$,(#36579));
#36585=PRODUCT('DIN 439-2 - M5 x 0.8 Steel 6 Plain',
'Hexagon Thin Nut DIN 439-2 - M5 x 0.8 Steel 6 Plain v1',
'Hexagon Thin Nut DIN 439-2 - M5 x 0.8',(#36579));
#36586=PRODUCT(
'5908K51_Highly Corrosion-Resistant 316 Stainless Steel Ball Bearing',
'5908K51_Highly Corrosion-Resistant 316 Stainless Steel Ball Bearing',$,
(#36579));
#36587=PRODUCT('V-Slot 20x40','V-Slot 20x40',$,(#36579));
#36588=PRODUCT('pulley','Pulley',$,(#36579));
#36589=PRODUCT('Bracket_Motor','Bracket_Motor',$,(#36579));
#36590=PRODUCT('Pulley_Motor','Pulley_Motor',$,(#36579));
#36591=PRODUCT('GT2_Belt','GT2_Belt',$,(#36579));
#36592=PRODUCT('Bracket_Middle','Bracket_Middle',$,(#36579));
#36593=PRODUCT('Bracket','Bracket',$,(#36579));
#36594=PRODUCT(
'BHSBHCS ASME B18.3.4M - M5 x 0.8 x 30 Steel Grade 2 Plain',
'BHSBHCS ASME B18.3.4M - M5 x 0.8 x 30 Steel Grade 2 Plain',
'Broached Hexagon Socket Button Head Cap Screw ASME B18.3.4M - M5 x 0.
8 x 30',(#36579));
#36595=PRESENTATION_STYLE_ASSIGNMENT((#36600));
#36596=PRESENTATION_STYLE_ASSIGNMENT((#36601));
#36597=PRESENTATION_STYLE_ASSIGNMENT((#36602));
#36598=PRESENTATION_STYLE_ASSIGNMENT((#36603));
#36599=PRESENTATION_STYLE_ASSIGNMENT((#36604));
#36600=SURFACE_STYLE_USAGE(.BOTH.,#36605);
#36601=SURFACE_STYLE_USAGE(.BOTH.,#36606);
#36602=SURFACE_STYLE_USAGE(.BOTH.,#36607);
#36603=SURFACE_STYLE_USAGE(.BOTH.,#36608);
#36604=SURFACE_STYLE_USAGE(.BOTH.,#36609);
#36605=SURFACE_SIDE_STYLE('',(#36610));
#36606=SURFACE_SIDE_STYLE('',(#36611));
#36607=SURFACE_SIDE_STYLE('',(#36612));
#36608=SURFACE_SIDE_STYLE('',(#36613));
#36609=SURFACE_SIDE_STYLE('',(#36614));
#36610=SURFACE_STYLE_FILL_AREA(#36615);
#36611=SURFACE_STYLE_FILL_AREA(#36616);
#36612=SURFACE_STYLE_FILL_AREA(#36617);
#36613=SURFACE_STYLE_FILL_AREA(#36618);
#36614=SURFACE_STYLE_FILL_AREA(#36619);
#36615=FILL_AREA_STYLE('Steel - Satin',(#36620));
#36616=FILL_AREA_STYLE('Opaque(160,160,160)',(#36621));
#36617=FILL_AREA_STYLE('Opaque(39,39,39)',(#36622));
#36618=FILL_AREA_STYLE('Opaque(245,245,246)',(#36623));
#36619=FILL_AREA_STYLE('Opaque(203,203,203)',(#36624));
#36620=FILL_AREA_STYLE_COLOUR('Steel - Satin',#36625);
#36621=FILL_AREA_STYLE_COLOUR('Opaque(160,160,160)',#36626);
#36622=FILL_AREA_STYLE_COLOUR('Opaque(39,39,39)',#36627);
#36623=FILL_AREA_STYLE_COLOUR('Opaque(245,245,246)',#36628);
#36624=FILL_AREA_STYLE_COLOUR('Opaque(203,203,203)',#36629);
#36625=COLOUR_RGB('Steel - Satin', 0.09019608, 0.27058824, 0.51372549);
#36626=COLOUR_RGB('Opaque(160,160,160)', 0.09019608, 0.27058824, 0.51372549);
#36627=COLOUR_RGB('Opaque(39,39,39)', 0.31764706, 0.68627451, 0.89019608);
#36628=COLOUR_RGB('Opaque(245,245,246)', 0.40784314, 0.44705882, 0.49803922);
#36629=COLOUR_RGB('Opaque(203,203,203)', 0.72549020, 0.75294118, 0.79215686);
ENDSEC;
END-ISO-10303-21;
